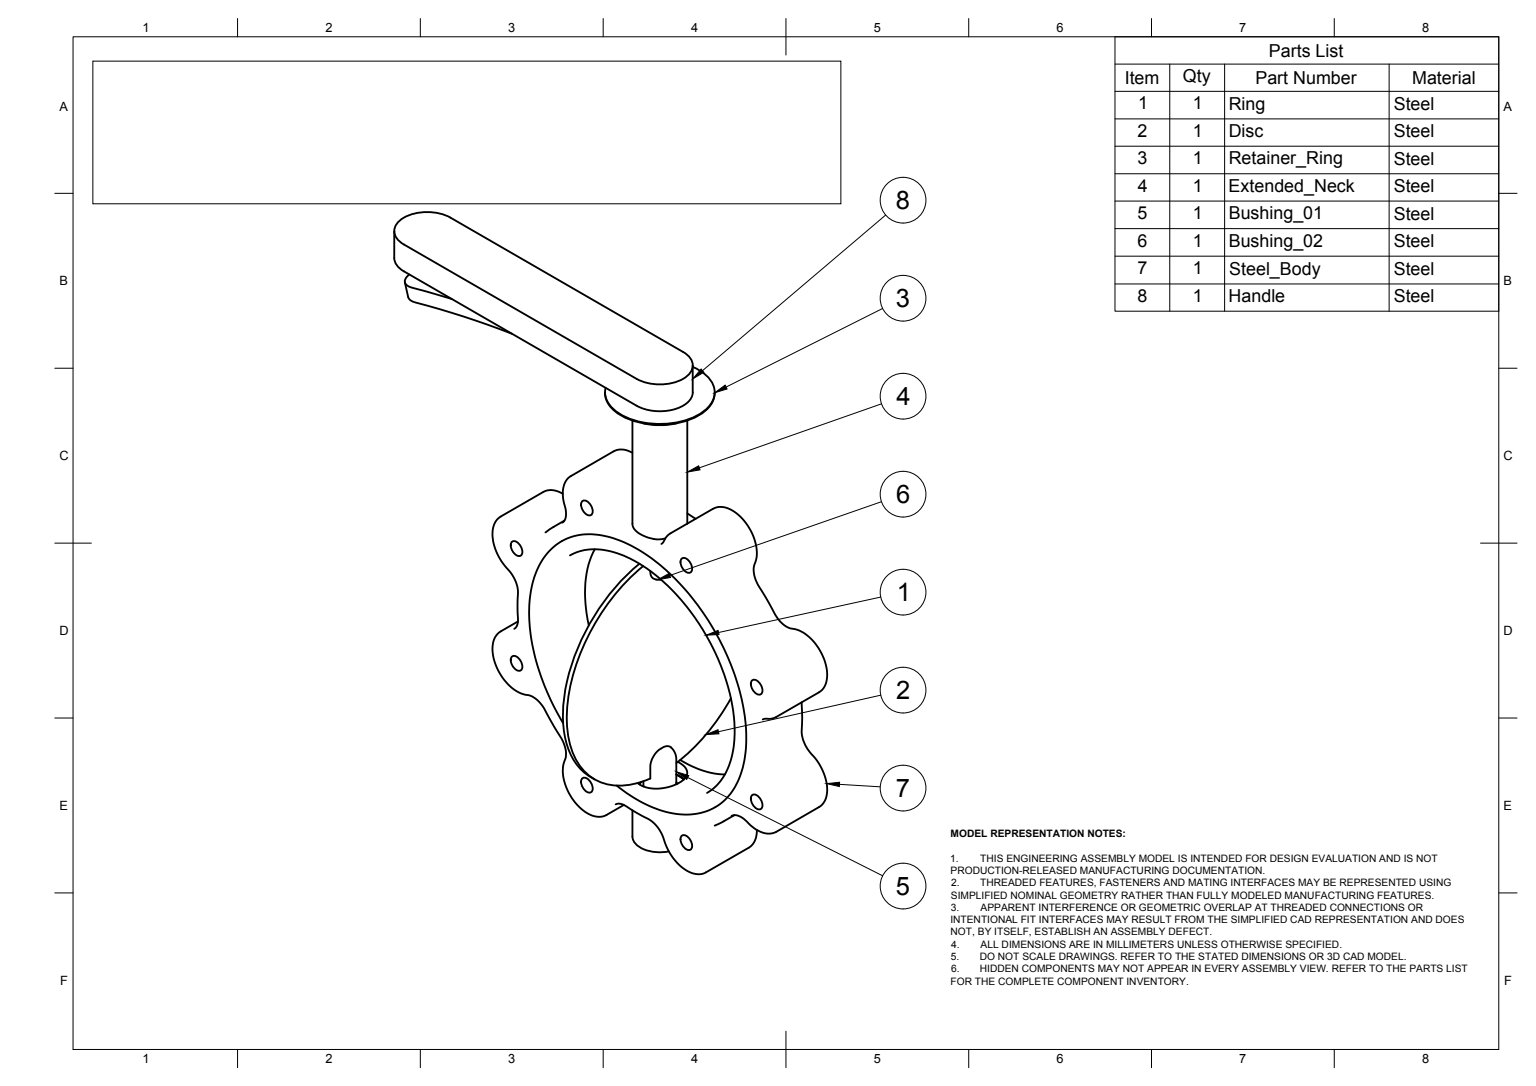
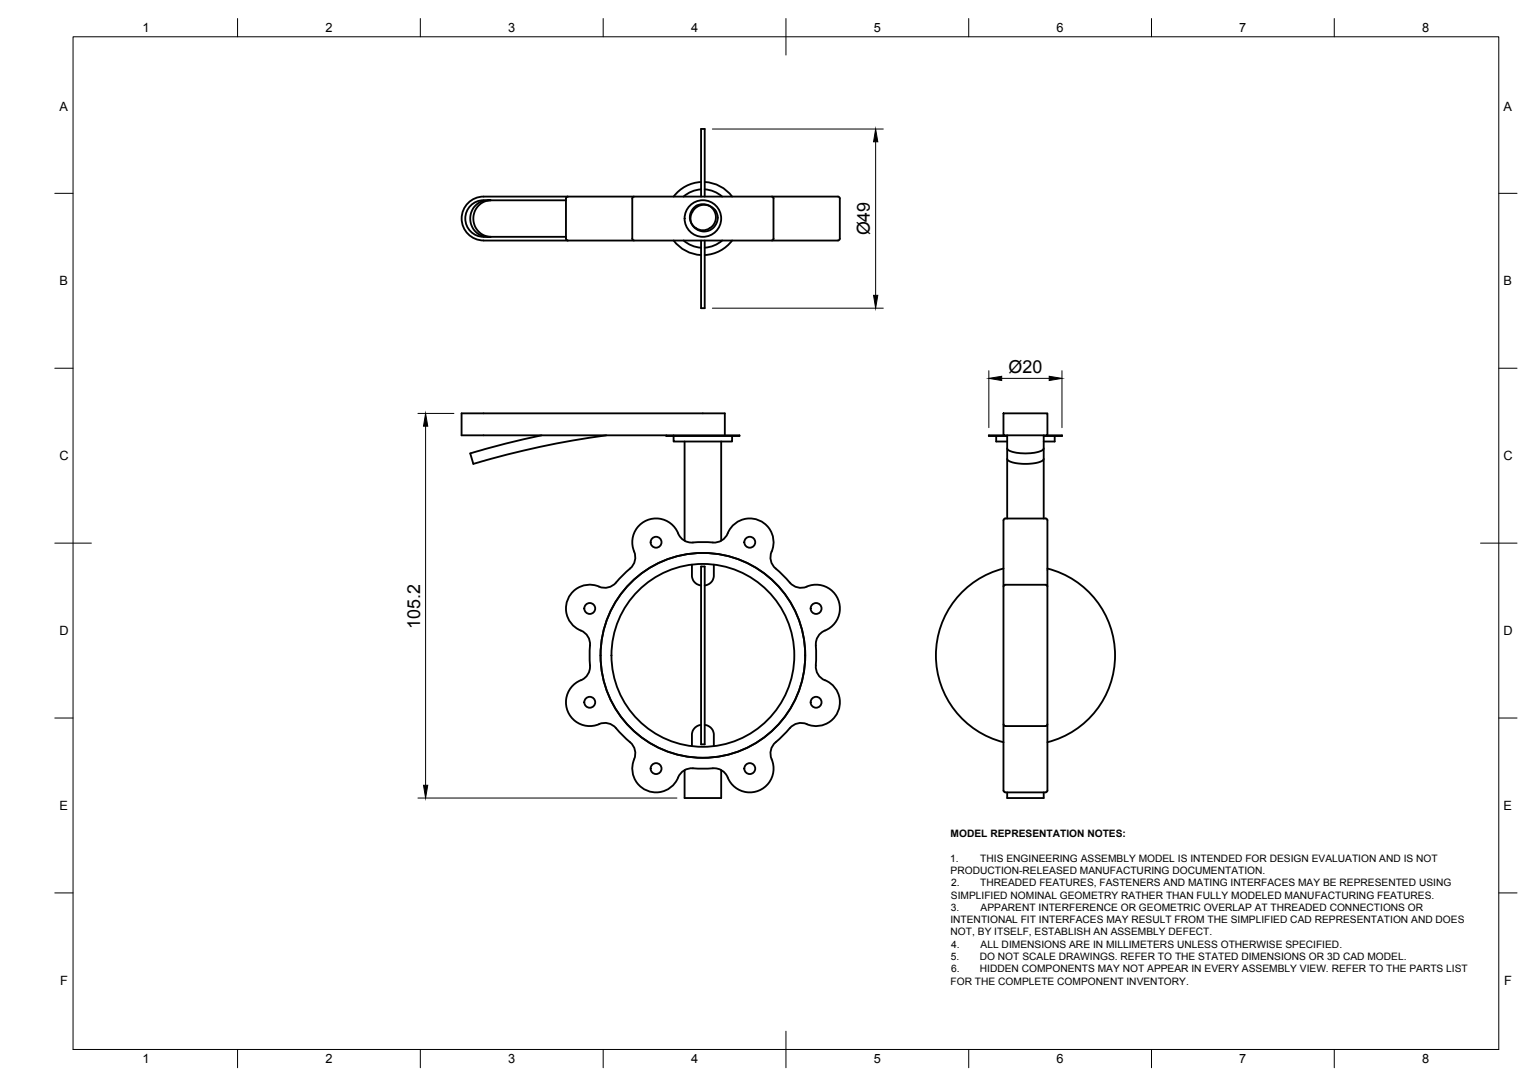
ISO-10303-21;
HEADER;
/* Generated by software containing ST-Developer
 * from STEP Tools, Inc. (www.steptools.com) 
 */

FILE_DESCRIPTION(
/* description */ (''),
/* implementation_level */ '2;1');

FILE_NAME(
/* name */ 'BR-303',
/* time_stamp */ '2026-10-06T12:52:28-07:00',
/* author */ (''),
/* organization */ (''),
/* preprocessor_version */ 'ST-DEVELOPER v20.2',
/* originating_system */ 'Autodesk Translation Framework v15.15.0.0',
/* authorisation */ '');

FILE_SCHEMA (('AUTOMOTIVE_DESIGN { 1 0 10303 214 3 1 1 }'));
ENDSEC;

DATA;
#10=MECHANICAL_DESIGN_GEOMETRIC_PRESENTATION_REPRESENTATION('',(#73,#74,
#75,#76,#77,#78,#79,#80),#34403);
#11=ITEM_DEFINED_TRANSFORMATION($,$,#4480,#4995);
#12=ITEM_DEFINED_TRANSFORMATION($,$,#4507,#4996);
#13=ITEM_DEFINED_TRANSFORMATION($,$,#4513,#4997);
#14=ITEM_DEFINED_TRANSFORMATION($,$,#4522,#4998);
#15=ITEM_DEFINED_TRANSFORMATION($,$,#4557,#4999);
#16=ITEM_DEFINED_TRANSFORMATION($,$,#4579,#5000);
#17=ITEM_DEFINED_TRANSFORMATION($,$,#4604,#5001);
#18=ITEM_DEFINED_TRANSFORMATION($,$,#4956,#5002);
#19=(
REPRESENTATION_RELATIONSHIP($,$,#34435,#34434)
REPRESENTATION_RELATIONSHIP_WITH_TRANSFORMATION(#11)
SHAPE_REPRESENTATION_RELATIONSHIP()
);
#20=(
REPRESENTATION_RELATIONSHIP($,$,#34436,#34434)
REPRESENTATION_RELATIONSHIP_WITH_TRANSFORMATION(#12)
SHAPE_REPRESENTATION_RELATIONSHIP()
);
#21=(
REPRESENTATION_RELATIONSHIP($,$,#34437,#34434)
REPRESENTATION_RELATIONSHIP_WITH_TRANSFORMATION(#13)
SHAPE_REPRESENTATION_RELATIONSHIP()
);
#22=(
REPRESENTATION_RELATIONSHIP($,$,#34438,#34434)
REPRESENTATION_RELATIONSHIP_WITH_TRANSFORMATION(#14)
SHAPE_REPRESENTATION_RELATIONSHIP()
);
#23=(
REPRESENTATION_RELATIONSHIP($,$,#34439,#34434)
REPRESENTATION_RELATIONSHIP_WITH_TRANSFORMATION(#15)
SHAPE_REPRESENTATION_RELATIONSHIP()
);
#24=(
REPRESENTATION_RELATIONSHIP($,$,#34440,#34434)
REPRESENTATION_RELATIONSHIP_WITH_TRANSFORMATION(#16)
SHAPE_REPRESENTATION_RELATIONSHIP()
);
#25=(
REPRESENTATION_RELATIONSHIP($,$,#34441,#34434)
REPRESENTATION_RELATIONSHIP_WITH_TRANSFORMATION(#17)
SHAPE_REPRESENTATION_RELATIONSHIP()
);
#26=(
REPRESENTATION_RELATIONSHIP($,$,#34442,#34434)
REPRESENTATION_RELATIONSHIP_WITH_TRANSFORMATION(#18)
SHAPE_REPRESENTATION_RELATIONSHIP()
);
#27=CONTEXT_DEPENDENT_SHAPE_REPRESENTATION(#19,#34426);
#28=CONTEXT_DEPENDENT_SHAPE_REPRESENTATION(#20,#34427);
#29=CONTEXT_DEPENDENT_SHAPE_REPRESENTATION(#21,#34428);
#30=CONTEXT_DEPENDENT_SHAPE_REPRESENTATION(#22,#34429);
#31=CONTEXT_DEPENDENT_SHAPE_REPRESENTATION(#23,#34430);
#32=CONTEXT_DEPENDENT_SHAPE_REPRESENTATION(#24,#34431);
#33=CONTEXT_DEPENDENT_SHAPE_REPRESENTATION(#25,#34432);
#34=CONTEXT_DEPENDENT_SHAPE_REPRESENTATION(#26,#34433);
#35=NEXT_ASSEMBLY_USAGE_OCCURRENCE('Ring:1','Ring:1','Ring:1',#34444,#34445,
'Ring:1');
#36=NEXT_ASSEMBLY_USAGE_OCCURRENCE('Disc:1','Disc:1','Disc:1',#34444,#34446,
'Disc:1');
#37=NEXT_ASSEMBLY_USAGE_OCCURRENCE('Retainer_Ring:1','Retainer_Ring:1',
'Retainer_Ring:1',#34444,#34447,'Retainer_Ring:1');
#38=NEXT_ASSEMBLY_USAGE_OCCURRENCE('Extended_Neck:1','Extended_Neck:1',
'Extended_Neck:1',#34444,#34448,'Extended_Neck:1');
#39=NEXT_ASSEMBLY_USAGE_OCCURRENCE('Bushing_01:1','Bushing_01:1',
'Bushing_01:1',#34444,#34449,'Bushing_01:1');
#40=NEXT_ASSEMBLY_USAGE_OCCURRENCE('Bushing_02:1','Bushing_02:1',
'Bushing_02:1',#34444,#34450,'Bushing_02:1');
#41=NEXT_ASSEMBLY_USAGE_OCCURRENCE('Steel_Body:1','Steel_Body:1',
'Steel_Body:1',#34444,#34451,'Steel_Body:1');
#42=NEXT_ASSEMBLY_USAGE_OCCURRENCE('Handle:1','Handle:1','Handle:1',#34444,
#34452,'Handle:1');
#43=ELLIPSE('',#4958,16.4522491302287,5.);
#44=ELLIPSE('',#4959,16.4522491302287,5.);
#45=B_SPLINE_SURFACE_WITH_KNOTS('',3,3,((#12810,#12811,#12812,#12813,#12814,
#12815,#12816,#12817,#12818,#12819,#12820,#12821,#12822,#12823,#12824,#12825,
#12826,#12827,#12828,#12829,#12830,#12831,#12832,#12833,#12834,#12835,#12836,
#12837,#12838,#12839,#12840,#12841,#12842,#12843,#12844,#12845,#12846,#12847,
#12848,#12849,#12850,#12851,#12852,#12853,#12854,#12855,#12856,#12857,#12858,
#12859,#12860,#12861,#12862,#12863,#12864,#12865),(#12866,#12867,#12868,
#12869,#12870,#12871,#12872,#12873,#12874,#12875,#12876,#12877,#12878,#12879,
#12880,#12881,#12882,#12883,#12884,#12885,#12886,#12887,#12888,#12889,#12890,
#12891,#12892,#12893,#12894,#12895,#12896,#12897,#12898,#12899,#12900,#12901,
#12902,#12903,#12904,#12905,#12906,#12907,#12908,#12909,#12910,#12911,#12912,
#12913,#12914,#12915,#12916,#12917,#12918,#12919,#12920,#12921),(#12922,
#12923,#12924,#12925,#12926,#12927,#12928,#12929,#12930,#12931,#12932,#12933,
#12934,#12935,#12936,#12937,#12938,#12939,#12940,#12941,#12942,#12943,#12944,
#12945,#12946,#12947,#12948,#12949,#12950,#12951,#12952,#12953,#12954,#12955,
#12956,#12957,#12958,#12959,#12960,#12961,#12962,#12963,#12964,#12965,#12966,
#12967,#12968,#12969,#12970,#12971,#12972,#12973,#12974,#12975,#12976,#12977),
(#12978,#12979,#12980,#12981,#12982,#12983,#12984,#12985,#12986,#12987,
#12988,#12989,#12990,#12991,#12992,#12993,#12994,#12995,#12996,#12997,#12998,
#12999,#13000,#13001,#13002,#13003,#13004,#13005,#13006,#13007,#13008,#13009,
#13010,#13011,#13012,#13013,#13014,#13015,#13016,#13017,#13018,#13019,#13020,
#13021,#13022,#13023,#13024,#13025,#13026,#13027,#13028,#13029,#13030,#13031,
#13032,#13033)),.UNSPECIFIED.,.F.,.F.,.F.,(4,4),(4,1,1,1,1,1,1,1,1,1,1,
1,1,1,1,1,1,1,1,1,1,1,1,1,1,1,1,1,1,1,1,1,1,1,1,1,1,1,1,1,1,1,1,1,1,1,1,
1,1,1,1,1,1,4),(-0.00052867975577478,0.0806738746488675),(15.627449007124,
16.6139235895809,17.6003981720377,18.5868727544945,19.5733473369513,20.5598219194081,
21.5462965018649,22.5327710843217,23.5192456667785,24.5057202492353,25.4921948316921,
26.4786694141489,27.4651439966058,28.4516185790626,29.4380931615194,30.4245677439762,
31.411042326433,32.3975169088898,33.3839914913466,34.3704660738034,35.3569406562602,
36.343415238717,37.3298898211739,38.3163644036307,39.3028389860875,40.2893135685443,
41.2757881510011,42.2622627334579,43.2487373159147,44.2352118983715,45.2216864808283,
46.2081610632851,47.1946356457419,48.1811102281988,49.1675848106556,50.1540593931124,
51.1405339755692,52.127008558026,53.1134831404828,54.0999577229396,55.0864323053964,
56.0729068878532,57.05938147031,58.0458560527669,59.0323306352237,60.0188052176805,
61.0052798001373,61.9917543825941,62.9782289650509,63.9647035475077,64.9511781299645,
65.9376527124213,66.9241272948781,67.9106018773349),.UNSPECIFIED.);
#46=B_SPLINE_SURFACE_WITH_KNOTS('',3,3,((#13314,#13315,#13316,#13317,#13318,
#13319,#13320,#13321,#13322,#13323,#13324,#13325,#13326,#13327,#13328,#13329,
#13330,#13331,#13332,#13333,#13334,#13335,#13336,#13337,#13338,#13339,#13340,
#13341,#13342,#13343,#13344,#13345,#13346,#13347,#13348,#13349,#13350,#13351,
#13352,#13353,#13354,#13355,#13356,#13357,#13358,#13359,#13360,#13361,#13362,
#13363,#13364,#13365,#13366,#13367,#13368,#13369),(#13370,#13371,#13372,
#13373,#13374,#13375,#13376,#13377,#13378,#13379,#13380,#13381,#13382,#13383,
#13384,#13385,#13386,#13387,#13388,#13389,#13390,#13391,#13392,#13393,#13394,
#13395,#13396,#13397,#13398,#13399,#13400,#13401,#13402,#13403,#13404,#13405,
#13406,#13407,#13408,#13409,#13410,#13411,#13412,#13413,#13414,#13415,#13416,
#13417,#13418,#13419,#13420,#13421,#13422,#13423,#13424,#13425),(#13426,
#13427,#13428,#13429,#13430,#13431,#13432,#13433,#13434,#13435,#13436,#13437,
#13438,#13439,#13440,#13441,#13442,#13443,#13444,#13445,#13446,#13447,#13448,
#13449,#13450,#13451,#13452,#13453,#13454,#13455,#13456,#13457,#13458,#13459,
#13460,#13461,#13462,#13463,#13464,#13465,#13466,#13467,#13468,#13469,#13470,
#13471,#13472,#13473,#13474,#13475,#13476,#13477,#13478,#13479,#13480,#13481),
(#13482,#13483,#13484,#13485,#13486,#13487,#13488,#13489,#13490,#13491,
#13492,#13493,#13494,#13495,#13496,#13497,#13498,#13499,#13500,#13501,#13502,
#13503,#13504,#13505,#13506,#13507,#13508,#13509,#13510,#13511,#13512,#13513,
#13514,#13515,#13516,#13517,#13518,#13519,#13520,#13521,#13522,#13523,#13524,
#13525,#13526,#13527,#13528,#13529,#13530,#13531,#13532,#13533,#13534,#13535,
#13536,#13537)),.UNSPECIFIED.,.F.,.F.,.F.,(4,4),(4,1,1,1,1,1,1,1,1,1,1,
1,1,1,1,1,1,1,1,1,1,1,1,1,1,1,1,1,1,1,1,1,1,1,1,1,1,1,1,1,1,1,1,1,1,1,1,
1,1,1,1,1,1,4),(-0.000393360025247636,0.0809589398657946),(18.1690368310252,
19.155511413482,20.1419859959388,21.1284605783956,22.1149351608524,23.1014097433092,
24.087884325766,25.0743589082228,26.0608334906796,27.0473080731364,28.0337826555933,
29.0202572380501,30.0067318205069,30.9932064029637,31.9796809854205,32.9661555678773,
33.9526301503341,34.9391047327909,35.9255793152477,36.9120538977045,37.8985284801614,
38.8850030626182,39.871477645075,40.8579522275318,41.8444268099886,42.8309013924454,
43.8173759749022,44.803850557359,45.7903251398158,46.7767997222726,47.7632743047295,
48.7497488871863,49.7362234696431,50.7226980520999,51.7091726345567,52.6956472170135,
53.6821217994703,54.6685963819271,55.6550709643839,56.6415455468407,57.6280201292976,
58.6144947117544,59.6009692942112,60.587443876668,61.5739184591248,62.5603930415816,
63.5468676240384,64.5333422064952,65.519816788952,66.5062913714088,67.4927659538656,
68.4792405363225,69.4657151187793,70.452868086171),.UNSPECIFIED.);
#47=B_SPLINE_SURFACE_WITH_KNOTS('',3,3,((#18145,#18146,#18147,#18148,#18149,
#18150,#18151,#18152,#18153),(#18154,#18155,#18156,#18157,#18158,#18159,
#18160,#18161,#18162),(#18163,#18164,#18165,#18166,#18167,#18168,#18169,
#18170,#18171),(#18172,#18173,#18174,#18175,#18176,#18177,#18178,#18179,
#18180),(#18181,#18182,#18183,#18184,#18185,#18186,#18187,#18188,#18189)),
 .UNSPECIFIED.,.F.,.F.,.F.,(4,1,4),(4,1,1,1,1,1,4),(-2.31295147948379E-5,
0.571428571428571,1.),(-0.0392722280793192,-0.0280568740573752,-0.00562616601348723,
0.00558918800845676,0.0168045420304008,0.0280198960523448,0.0392352500742888),
 .UNSPECIFIED.);
#48=B_SPLINE_SURFACE_WITH_KNOTS('',3,3,((#18360,#18361,#18362,#18363,#18364,
#18365,#18366,#18367,#18368,#18369),(#18370,#18371,#18372,#18373,#18374,
#18375,#18376,#18377,#18378,#18379),(#18380,#18381,#18382,#18383,#18384,
#18385,#18386,#18387,#18388,#18389),(#18390,#18391,#18392,#18393,#18394,
#18395,#18396,#18397,#18398,#18399),(#18400,#18401,#18402,#18403,#18404,
#18405,#18406,#18407,#18408,#18409)),.UNSPECIFIED.,.F.,.F.,.F.,(4,1,4),
(4,1,1,1,1,1,1,4),(-2.35337788502184E-5,0.571428571428571,1.),(-0.0392722280793192,
-0.0280568740573752,-0.0168415200354311,-0.00562616601348712,0.0055891880084569,
0.0168045420304009,0.0280198960523449,0.0392352500742889),.UNSPECIFIED.);
#49=B_SPLINE_SURFACE_WITH_KNOTS('',3,3,((#18444,#18445,#18446,#18447,#18448,
#18449,#18450,#18451,#18452,#18453,#18454,#18455,#18456,#18457,#18458,#18459,
#18460,#18461,#18462,#18463,#18464,#18465,#18466,#18467,#18468,#18469,#18470,
#18471,#18472,#18473,#18474,#18475,#18476,#18477,#18478,#18479,#18480,#18481,
#18482,#18483,#18484,#18485,#18486,#18487,#18488,#18489),(#18490,#18491,
#18492,#18493,#18494,#18495,#18496,#18497,#18498,#18499,#18500,#18501,#18502,
#18503,#18504,#18505,#18506,#18507,#18508,#18509,#18510,#18511,#18512,#18513,
#18514,#18515,#18516,#18517,#18518,#18519,#18520,#18521,#18522,#18523,#18524,
#18525,#18526,#18527,#18528,#18529,#18530,#18531,#18532,#18533,#18534,#18535),
(#18536,#18537,#18538,#18539,#18540,#18541,#18542,#18543,#18544,#18545,
#18546,#18547,#18548,#18549,#18550,#18551,#18552,#18553,#18554,#18555,#18556,
#18557,#18558,#18559,#18560,#18561,#18562,#18563,#18564,#18565,#18566,#18567,
#18568,#18569,#18570,#18571,#18572,#18573,#18574,#18575,#18576,#18577,#18578,
#18579,#18580,#18581),(#18582,#18583,#18584,#18585,#18586,#18587,#18588,
#18589,#18590,#18591,#18592,#18593,#18594,#18595,#18596,#18597,#18598,#18599,
#18600,#18601,#18602,#18603,#18604,#18605,#18606,#18607,#18608,#18609,#18610,
#18611,#18612,#18613,#18614,#18615,#18616,#18617,#18618,#18619,#18620,#18621,
#18622,#18623,#18624,#18625,#18626,#18627)),.UNSPECIFIED.,.F.,.F.,.F.,(4,
4),(4,1,1,1,1,1,1,1,1,1,1,1,1,1,1,1,1,1,1,1,1,1,1,1,1,1,1,1,1,1,1,1,1,1,
1,1,1,1,1,1,1,1,1,4),(-0.000633807887895752,0.0823317564776454),(8.31473274985803,
9.29783943738047,10.2809461249029,11.2640528124254,12.2471594999478,13.2302661874702,
14.2133728749927,15.1964795625151,16.1795862500376,17.16269293756,18.1457996250825,
19.1289063126049,20.1120130001274,21.0951196876498,22.0782263751723,23.0613330626947,
24.0444397502171,25.0275464377396,26.010653125262,26.9937598127845,27.9768665003069,
28.9599731878294,29.9430798753518,30.9261865628743,31.9092932503967,32.8923999379191,
33.8755066254416,34.858613312964,35.8417200004865,36.8248266880089,37.8079333755314,
38.7910400630538,39.7741467505763,40.7572534380987,41.7403601256211,42.7234668131436,
43.706573500666,44.6896801881885,45.6727868757109,46.6558935632334,47.6390002507558,
48.6221069382783,49.6052136258007,50.5889541212111),.UNSPECIFIED.);
#50=B_SPLINE_SURFACE_WITH_KNOTS('',3,3,((#18809,#18810,#18811,#18812,#18813,
#18814,#18815,#18816,#18817,#18818,#18819,#18820,#18821,#18822,#18823,#18824,
#18825,#18826,#18827,#18828,#18829,#18830,#18831,#18832,#18833,#18834,#18835,
#18836,#18837,#18838,#18839,#18840,#18841,#18842,#18843,#18844,#18845,#18846,
#18847,#18848,#18849,#18850,#18851,#18852,#18853,#18854),(#18855,#18856,
#18857,#18858,#18859,#18860,#18861,#18862,#18863,#18864,#18865,#18866,#18867,
#18868,#18869,#18870,#18871,#18872,#18873,#18874,#18875,#18876,#18877,#18878,
#18879,#18880,#18881,#18882,#18883,#18884,#18885,#18886,#18887,#18888,#18889,
#18890,#18891,#18892,#18893,#18894,#18895,#18896,#18897,#18898,#18899,#18900),
(#18901,#18902,#18903,#18904,#18905,#18906,#18907,#18908,#18909,#18910,
#18911,#18912,#18913,#18914,#18915,#18916,#18917,#18918,#18919,#18920,#18921,
#18922,#18923,#18924,#18925,#18926,#18927,#18928,#18929,#18930,#18931,#18932,
#18933,#18934,#18935,#18936,#18937,#18938,#18939,#18940,#18941,#18942,#18943,
#18944,#18945,#18946),(#18947,#18948,#18949,#18950,#18951,#18952,#18953,
#18954,#18955,#18956,#18957,#18958,#18959,#18960,#18961,#18962,#18963,#18964,
#18965,#18966,#18967,#18968,#18969,#18970,#18971,#18972,#18973,#18974,#18975,
#18976,#18977,#18978,#18979,#18980,#18981,#18982,#18983,#18984,#18985,#18986,
#18987,#18988,#18989,#18990,#18991,#18992)),.UNSPECIFIED.,.F.,.F.,.F.,(4,
4),(4,1,1,1,1,1,1,1,1,1,1,1,1,1,1,1,1,1,1,1,1,1,1,1,1,1,1,1,1,1,1,1,1,1,
1,1,1,1,1,1,1,1,1,4),(-0.000319018948610172,0.0826465308545402),(11.6145803026385,
12.5983209152772,13.5814276027996,14.564534290322,15.5476409778445,16.5307476653669,
17.5138543528894,18.4969610404118,19.4800677279343,20.4631744154567,21.4462811029792,
22.4293877905016,23.4124944780241,24.3956011655465,25.3787078530689,26.3618145405914,
27.3449212281138,28.3280279156363,29.3111346031587,30.2942412906812,31.2773479782036,
32.2604546657261,33.2435613532485,34.226668040771,35.2097747282934,36.1928814158158,
37.1759881033383,38.1590947908607,39.1422014783832,40.1253081659056,41.1084148534281,
42.0915215409505,43.074628228473,44.0577349159954,45.0408416035178,46.0239482910403,
47.0070549785627,47.9901616660852,48.9732683536076,49.9563750411301,50.9394817286525,
51.922588416175,52.9056951036974,53.8888017912198),.UNSPECIFIED.);
#51=B_SPLINE_SURFACE_WITH_KNOTS('',3,3,((#24901,#24902,#24903,#24904,#24905,
#24906,#24907,#24908,#24909),(#24910,#24911,#24912,#24913,#24914,#24915,
#24916,#24917,#24918),(#24919,#24920,#24921,#24922,#24923,#24924,#24925,
#24926,#24927),(#24928,#24929,#24930,#24931,#24932,#24933,#24934,#24935,
#24936),(#24937,#24938,#24939,#24940,#24941,#24942,#24943,#24944,#24945)),
 .UNSPECIFIED.,.F.,.F.,.F.,(4,1,4),(4,1,1,1,1,1,4),(-2.3129491492736E-5,
0.571428571428571,1.),(-0.0392722361364195,-0.0280568820761978,-0.00562617395575443,
0.00558918010446727,0.016804534164689,0.0280198882249107,0.0392352422851324),
 .UNSPECIFIED.);
#52=B_SPLINE_SURFACE_WITH_KNOTS('',3,3,((#25116,#25117,#25118,#25119,#25120,
#25121,#25122,#25123,#25124,#25125),(#25126,#25127,#25128,#25129,#25130,
#25131,#25132,#25133,#25134,#25135),(#25136,#25137,#25138,#25139,#25140,
#25141,#25142,#25143,#25144,#25145),(#25146,#25147,#25148,#25149,#25150,
#25151,#25152,#25153,#25154,#25155),(#25156,#25157,#25158,#25159,#25160,
#25161,#25162,#25163,#25164,#25165)),.UNSPECIFIED.,.F.,.F.,.F.,(4,1,4),
(4,1,1,1,1,1,1,4),(-2.35337502838191E-5,0.571428571428571,1.),(-0.0392722361364195,
-0.0280568820761979,-0.0168415280159762,-0.00562617395575452,0.00558918010446715,
0.0168045341646888,0.0280198882249105,0.0392352422851322),.UNSPECIFIED.);
#53=B_SPLINE_SURFACE_WITH_KNOTS('',3,3,((#25200,#25201,#25202,#25203,#25204,
#25205,#25206,#25207,#25208,#25209,#25210,#25211,#25212,#25213,#25214,#25215,
#25216,#25217,#25218,#25219,#25220,#25221,#25222,#25223,#25224,#25225,#25226,
#25227,#25228,#25229,#25230,#25231,#25232,#25233,#25234,#25235,#25236,#25237,
#25238,#25239,#25240,#25241,#25242,#25243,#25244,#25245,#25246,#25247,#25248,
#25249,#25250,#25251,#25252,#25253,#25254,#25255),(#25256,#25257,#25258,
#25259,#25260,#25261,#25262,#25263,#25264,#25265,#25266,#25267,#25268,#25269,
#25270,#25271,#25272,#25273,#25274,#25275,#25276,#25277,#25278,#25279,#25280,
#25281,#25282,#25283,#25284,#25285,#25286,#25287,#25288,#25289,#25290,#25291,
#25292,#25293,#25294,#25295,#25296,#25297,#25298,#25299,#25300,#25301,#25302,
#25303,#25304,#25305,#25306,#25307,#25308,#25309,#25310,#25311),(#25312,
#25313,#25314,#25315,#25316,#25317,#25318,#25319,#25320,#25321,#25322,#25323,
#25324,#25325,#25326,#25327,#25328,#25329,#25330,#25331,#25332,#25333,#25334,
#25335,#25336,#25337,#25338,#25339,#25340,#25341,#25342,#25343,#25344,#25345,
#25346,#25347,#25348,#25349,#25350,#25351,#25352,#25353,#25354,#25355,#25356,
#25357,#25358,#25359,#25360,#25361,#25362,#25363,#25364,#25365,#25366,#25367),
(#25368,#25369,#25370,#25371,#25372,#25373,#25374,#25375,#25376,#25377,
#25378,#25379,#25380,#25381,#25382,#25383,#25384,#25385,#25386,#25387,#25388,
#25389,#25390,#25391,#25392,#25393,#25394,#25395,#25396,#25397,#25398,#25399,
#25400,#25401,#25402,#25403,#25404,#25405,#25406,#25407,#25408,#25409,#25410,
#25411,#25412,#25413,#25414,#25415,#25416,#25417,#25418,#25419,#25420,#25421,
#25422,#25423)),.UNSPECIFIED.,.F.,.F.,.F.,(4,4),(4,1,1,1,1,1,1,1,1,1,1,
1,1,1,1,1,1,1,1,1,1,1,1,1,1,1,1,1,1,1,1,1,1,1,1,1,1,1,1,1,1,1,1,1,1,1,1,
1,1,1,1,1,1,4),(-0.000662226835936772,0.0823162805313219),(-97.5343202090122,
-96.5415235325365,-95.5487268560609,-94.5559301795852,-93.5631335031096,
-92.570336826634,-91.5775401501583,-90.5847434736827,-89.591946797207,-88.5991501207314,
-87.6063534442557,-86.6135567677801,-85.6207600913045,-84.6279634148288,
-83.6351667383532,-82.6423700618775,-81.6495733854019,-80.6567767089262,
-79.6639800324506,-78.671183355975,-77.6783866794993,-76.6855900030237,
-75.692793326548,-74.6999966500724,-73.7071999735967,-72.7144032971211,
-71.7216066206455,-70.7288099441698,-69.7360132676942,-68.7432165912185,
-67.7504199147429,-66.7576232382672,-65.7648265617916,-64.772029885316,
-63.7792332088403,-62.7864365323647,-61.793639855889,-60.8008431794134,
-59.8080465029377,-58.8152498264621,-57.8224531499865,-56.8296564735108,
-55.8368597970352,-54.8440631205595,-53.8512664440839,-52.8584697676082,
-51.8656730911326,-50.872876414657,-49.8800797381813,-48.8872830617057,
-47.89448638523,-46.9016897087544,-45.9088930322787,-44.9154341289673),
 .UNSPECIFIED.);
#54=B_SPLINE_SURFACE_WITH_KNOTS('',3,3,((#25626,#25627,#25628,#25629,#25630,
#25631,#25632,#25633,#25634,#25635,#25636,#25637,#25638,#25639,#25640,#25641,
#25642,#25643,#25644,#25645,#25646,#25647,#25648,#25649,#25650,#25651,#25652,
#25653,#25654,#25655,#25656,#25657,#25658,#25659,#25660,#25661,#25662,#25663,
#25664,#25665,#25666,#25667,#25668,#25669,#25670,#25671,#25672,#25673,#25674,
#25675,#25676,#25677,#25678,#25679,#25680,#25681),(#25682,#25683,#25684,
#25685,#25686,#25687,#25688,#25689,#25690,#25691,#25692,#25693,#25694,#25695,
#25696,#25697,#25698,#25699,#25700,#25701,#25702,#25703,#25704,#25705,#25706,
#25707,#25708,#25709,#25710,#25711,#25712,#25713,#25714,#25715,#25716,#25717,
#25718,#25719,#25720,#25721,#25722,#25723,#25724,#25725,#25726,#25727,#25728,
#25729,#25730,#25731,#25732,#25733,#25734,#25735,#25736,#25737),(#25738,
#25739,#25740,#25741,#25742,#25743,#25744,#25745,#25746,#25747,#25748,#25749,
#25750,#25751,#25752,#25753,#25754,#25755,#25756,#25757,#25758,#25759,#25760,
#25761,#25762,#25763,#25764,#25765,#25766,#25767,#25768,#25769,#25770,#25771,
#25772,#25773,#25774,#25775,#25776,#25777,#25778,#25779,#25780,#25781,#25782,
#25783,#25784,#25785,#25786,#25787,#25788,#25789,#25790,#25791,#25792,#25793),
(#25794,#25795,#25796,#25797,#25798,#25799,#25800,#25801,#25802,#25803,
#25804,#25805,#25806,#25807,#25808,#25809,#25810,#25811,#25812,#25813,#25814,
#25815,#25816,#25817,#25818,#25819,#25820,#25821,#25822,#25823,#25824,#25825,
#25826,#25827,#25828,#25829,#25830,#25831,#25832,#25833,#25834,#25835,#25836,
#25837,#25838,#25839,#25840,#25841,#25842,#25843,#25844,#25845,#25846,#25847,
#25848,#25849)),.UNSPECIFIED.,.F.,.F.,.F.,(4,4),(4,1,1,1,1,1,1,1,1,1,1,
1,1,1,1,1,1,1,1,1,1,1,1,1,1,1,1,1,1,1,1,1,1,1,1,1,1,1,1,1,1,1,1,1,1,1,1,
1,1,1,1,1,1,4),(-0.000307057037193035,0.0826748885905267),(-94.2345010139676,
-93.2410420546399,-92.2482453781643,-91.2554487016887,-90.2626520252132,
-89.2698553487376,-88.277058672262,-87.2842619957864,-86.2914653193108,
-85.2986686428353,-84.3058719663597,-83.3130752898841,-82.3202786134085,
-81.327481936933,-80.3346852604574,-79.3418885839818,-78.3490919075062,
-77.3562952310307,-76.3634985545551,-75.3707018780795,-74.3779052016039,
-73.3851085251283,-72.3923118486528,-71.3995151721772,-70.4067184957016,
-69.413921819226,-68.4211251427505,-67.4283284662749,-66.4355317897993,
-65.4427351133237,-64.4499384368482,-63.4571417603726,-62.464345083897,
-61.4715484074214,-60.4787517309458,-59.4859550544703,-58.4931583779947,
-57.5003617015191,-56.5075650250435,-55.514768348568,-54.5219716720924,
-53.5291749956168,-52.5363783191412,-51.5435816426657,-50.5507849661901,
-49.5579882897145,-48.5651916132389,-47.5723949367633,-46.5795982602878,
-45.5868015838122,-44.5940049073366,-43.601208230861,-42.6084115543855,
-41.6156148779099),.UNSPECIFIED.);
#55=B_SPLINE_SURFACE_WITH_KNOTS('',3,3,((#32660,#32661,#32662,#32663,#32664,
#32665,#32666,#32667,#32668,#32669,#32670,#32671,#32672,#32673,#32674,#32675,
#32676,#32677,#32678,#32679,#32680,#32681,#32682,#32683,#32684,#32685,#32686,
#32687,#32688,#32689,#32690,#32691,#32692,#32693,#32694,#32695,#32696,#32697,
#32698,#32699,#32700,#32701,#32702,#32703,#32704,#32705,#32706,#32707,#32708,
#32709,#32710,#32711,#32712,#32713,#32714,#32715,#32716,#32717,#32718,#32719,
#32720),(#32721,#32722,#32723,#32724,#32725,#32726,#32727,#32728,#32729,
#32730,#32731,#32732,#32733,#32734,#32735,#32736,#32737,#32738,#32739,#32740,
#32741,#32742,#32743,#32744,#32745,#32746,#32747,#32748,#32749,#32750,#32751,
#32752,#32753,#32754,#32755,#32756,#32757,#32758,#32759,#32760,#32761,#32762,
#32763,#32764,#32765,#32766,#32767,#32768,#32769,#32770,#32771,#32772,#32773,
#32774,#32775,#32776,#32777,#32778,#32779,#32780,#32781),(#32782,#32783,
#32784,#32785,#32786,#32787,#32788,#32789,#32790,#32791,#32792,#32793,#32794,
#32795,#32796,#32797,#32798,#32799,#32800,#32801,#32802,#32803,#32804,#32805,
#32806,#32807,#32808,#32809,#32810,#32811,#32812,#32813,#32814,#32815,#32816,
#32817,#32818,#32819,#32820,#32821,#32822,#32823,#32824,#32825,#32826,#32827,
#32828,#32829,#32830,#32831,#32832,#32833,#32834,#32835,#32836,#32837,#32838,
#32839,#32840,#32841,#32842),(#32843,#32844,#32845,#32846,#32847,#32848,
#32849,#32850,#32851,#32852,#32853,#32854,#32855,#32856,#32857,#32858,#32859,
#32860,#32861,#32862,#32863,#32864,#32865,#32866,#32867,#32868,#32869,#32870,
#32871,#32872,#32873,#32874,#32875,#32876,#32877,#32878,#32879,#32880,#32881,
#32882,#32883,#32884,#32885,#32886,#32887,#32888,#32889,#32890,#32891,#32892,
#32893,#32894,#32895,#32896,#32897,#32898,#32899,#32900,#32901,#32902,#32903)),
 .UNSPECIFIED.,.F.,.F.,.F.,(4,4),(4,1,1,1,1,1,1,1,1,1,1,1,1,1,1,1,1,1,1,
1,1,1,1,1,1,1,1,1,1,1,1,1,1,1,1,1,1,1,1,1,1,1,1,1,1,1,1,1,1,1,1,1,1,1,1,
1,1,1,4),(-0.000677904662105755,0.0806892635940671),(11.8568599181543,12.8456361179191,
13.8337344130217,14.8218327081244,15.8099310032271,16.7980292983297,17.7861275934324,
18.774225888535,19.7623241836377,20.7504224787404,21.738520773843,22.7266190689457,
23.7147173640484,24.702815659151,25.6909139542537,26.6790122493564,27.667110544459,
28.6552088395617,29.6433071346644,30.631405429767,31.6195037248697,32.6076020199723,
33.595700315075,34.5837986101777,35.5718969052803,36.559995200383,37.5480934954857,
38.5361917905883,39.524290085691,40.5123883807937,41.5004866758963,42.488584970999,
43.4766832661016,44.4647815612043,45.452879856307,46.4409781514096,47.4290764465123,
48.417174741615,49.4052730367176,50.3933713318203,51.381469626923,52.3695679220256,
53.3576662171283,54.345764512231,55.3338628073336,56.3219611024363,57.3100593975389,
58.2981576926416,59.2862559877443,60.2743542828469,61.2624525779496,62.2505508730523,
63.2386491681549,64.2267474632576,65.2148457583603,66.2029440534629,67.1910423485656,
68.1791406436682,69.1672389387709),.UNSPECIFIED.);
#56=B_SPLINE_SURFACE_WITH_KNOTS('',3,3,((#33092,#33093,#33094,#33095,#33096,
#33097,#33098,#33099,#33100,#33101,#33102,#33103,#33104,#33105,#33106,#33107,
#33108,#33109,#33110,#33111,#33112,#33113,#33114,#33115,#33116,#33117,#33118,
#33119,#33120,#33121,#33122,#33123,#33124,#33125,#33126,#33127,#33128,#33129,
#33130,#33131,#33132,#33133,#33134,#33135,#33136,#33137,#33138,#33139,#33140,
#33141,#33142,#33143,#33144,#33145,#33146,#33147,#33148,#33149,#33150,#33151,
#33152),(#33153,#33154,#33155,#33156,#33157,#33158,#33159,#33160,#33161,
#33162,#33163,#33164,#33165,#33166,#33167,#33168,#33169,#33170,#33171,#33172,
#33173,#33174,#33175,#33176,#33177,#33178,#33179,#33180,#33181,#33182,#33183,
#33184,#33185,#33186,#33187,#33188,#33189,#33190,#33191,#33192,#33193,#33194,
#33195,#33196,#33197,#33198,#33199,#33200,#33201,#33202,#33203,#33204,#33205,
#33206,#33207,#33208,#33209,#33210,#33211,#33212,#33213),(#33214,#33215,
#33216,#33217,#33218,#33219,#33220,#33221,#33222,#33223,#33224,#33225,#33226,
#33227,#33228,#33229,#33230,#33231,#33232,#33233,#33234,#33235,#33236,#33237,
#33238,#33239,#33240,#33241,#33242,#33243,#33244,#33245,#33246,#33247,#33248,
#33249,#33250,#33251,#33252,#33253,#33254,#33255,#33256,#33257,#33258,#33259,
#33260,#33261,#33262,#33263,#33264,#33265,#33266,#33267,#33268,#33269,#33270,
#33271,#33272,#33273,#33274),(#33275,#33276,#33277,#33278,#33279,#33280,
#33281,#33282,#33283,#33284,#33285,#33286,#33287,#33288,#33289,#33290,#33291,
#33292,#33293,#33294,#33295,#33296,#33297,#33298,#33299,#33300,#33301,#33302,
#33303,#33304,#33305,#33306,#33307,#33308,#33309,#33310,#33311,#33312,#33313,
#33314,#33315,#33316,#33317,#33318,#33319,#33320,#33321,#33322,#33323,#33324,
#33325,#33326,#33327,#33328,#33329,#33330,#33331,#33332,#33333,#33334,#33335)),
 .UNSPECIFIED.,.F.,.F.,.F.,(4,4),(4,1,1,1,1,1,1,1,1,1,1,1,1,1,1,1,1,1,1,
1,1,1,1,1,1,1,1,1,1,1,1,1,1,1,1,1,1,1,1,1,1,1,1,1,1,1,1,1,1,1,1,1,1,1,1,
1,1,1,4),(-0.000408738892527466,0.0809585600709479),(14.3991256467175,15.3872239418202,
16.3753222369229,17.3634205320255,18.3515188271282,19.3396171222308,20.3277154173335,
21.3158137124362,22.3039120075388,23.2920103026415,24.2801085977442,25.2682068928468,
26.2563051879495,27.2444034830521,28.2325017781548,29.2206000732575,30.2086983683601,
31.1967966634628,32.1848949585655,33.1729932536681,34.1610915487708,35.1491898438735,
36.1372881389761,37.1253864340788,38.1134847291814,39.1015830242841,40.0896813193868,
41.0777796144894,42.0658779095921,43.0539762046948,44.0420744997974,45.0301727949001,
46.0182710900028,47.0063693851054,47.9944676802081,48.9825659753107,49.9706642704134,
50.9587625655161,51.9468608606187,52.9349591557214,53.9230574508241,54.9111557459267,
55.8992540410294,56.8873523361321,57.8754506312347,58.8635489263374,59.85164722144,
60.8397455165427,61.8278438116454,62.815942106748,63.8040404018507,64.7921386969534,
65.780236992056,66.7683352871587,67.7564335822614,68.744531877364,69.7326301724667,
70.7207284675693,71.7095047678121),.UNSPECIFIED.);
#57=SHAPE_REPRESENTATION_RELATIONSHIP('SRR','None',#34435,#65);
#58=SHAPE_REPRESENTATION_RELATIONSHIP('SRR','None',#34436,#66);
#59=SHAPE_REPRESENTATION_RELATIONSHIP('SRR','None',#34437,#67);
#60=SHAPE_REPRESENTATION_RELATIONSHIP('SRR','None',#34438,#68);
#61=SHAPE_REPRESENTATION_RELATIONSHIP('SRR','None',#34439,#69);
#62=SHAPE_REPRESENTATION_RELATIONSHIP('SRR','None',#34440,#70);
#63=SHAPE_REPRESENTATION_RELATIONSHIP('SRR','None',#34441,#71);
#64=SHAPE_REPRESENTATION_RELATIONSHIP('SRR','None',#34442,#72);
#65=ADVANCED_BREP_SHAPE_REPRESENTATION('',(#81),#34395);
#66=ADVANCED_BREP_SHAPE_REPRESENTATION('',(#82),#34396);
#67=ADVANCED_BREP_SHAPE_REPRESENTATION('',(#83),#34397);
#68=ADVANCED_BREP_SHAPE_REPRESENTATION('',(#84),#34398);
#69=ADVANCED_BREP_SHAPE_REPRESENTATION('',(#85),#34399);
#70=ADVANCED_BREP_SHAPE_REPRESENTATION('',(#86),#34400);
#71=ADVANCED_BREP_SHAPE_REPRESENTATION('',(#87),#34401);
#72=ADVANCED_BREP_SHAPE_REPRESENTATION('',(#88),#34402);
#73=STYLED_ITEM('',(#34484),#81);
#74=STYLED_ITEM('',(#34484),#82);
#75=STYLED_ITEM('',(#34484),#83);
#76=STYLED_ITEM('',(#34484),#84);
#77=STYLED_ITEM('',(#34484),#85);
#78=STYLED_ITEM('',(#34484),#86);
#79=STYLED_ITEM('',(#34484),#87);
#80=STYLED_ITEM('',(#34484),#88);
#81=MANIFOLD_SOLID_BREP('Body1',#4382);
#82=MANIFOLD_SOLID_BREP('Body1',#4383);
#83=MANIFOLD_SOLID_BREP('Body1',#4384);
#84=MANIFOLD_SOLID_BREP('Body1',#4385);
#85=MANIFOLD_SOLID_BREP('Body1',#4386);
#86=MANIFOLD_SOLID_BREP('Body1',#4387);
#87=MANIFOLD_SOLID_BREP('Body1',#4388);
#88=MANIFOLD_SOLID_BREP('Body1',#4389);
#89=FACE_BOUND('',#751,.T.);
#90=FACE_BOUND('',#753,.T.);
#91=FACE_BOUND('',#754,.T.);
#92=FACE_BOUND('',#757,.T.);
#93=FACE_BOUND('',#758,.T.);
#94=FACE_BOUND('',#761,.T.);
#95=FACE_BOUND('',#769,.T.);
#96=FACE_BOUND('',#771,.T.);
#97=FACE_BOUND('',#795,.T.);
#98=FACE_BOUND('',#797,.T.);
#99=FACE_BOUND('',#800,.T.);
#100=FACE_BOUND('',#818,.T.);
#101=FACE_BOUND('',#839,.T.);
#102=FACE_BOUND('',#855,.T.);
#103=FACE_BOUND('',#858,.T.);
#104=FACE_BOUND('',#914,.T.);
#105=FACE_BOUND('',#915,.T.);
#106=FACE_BOUND('',#916,.T.);
#107=FACE_BOUND('',#917,.T.);
#108=FACE_BOUND('',#918,.T.);
#109=FACE_BOUND('',#919,.T.);
#110=FACE_BOUND('',#920,.T.);
#111=FACE_BOUND('',#921,.T.);
#112=FACE_BOUND('',#922,.T.);
#113=FACE_BOUND('',#970,.T.);
#114=FACE_BOUND('',#971,.T.);
#115=FACE_BOUND('',#972,.T.);
#116=FACE_BOUND('',#973,.T.);
#117=FACE_BOUND('',#974,.T.);
#118=FACE_BOUND('',#975,.T.);
#119=FACE_BOUND('',#976,.T.);
#120=FACE_BOUND('',#977,.T.);
#121=FACE_BOUND('',#978,.T.);
#122=FACE_BOUND('',#981,.T.);
#123=FACE_BOUND('',#982,.T.);
#124=FACE_BOUND('',#1013,.T.);
#125=PLANE('',#4488);
#126=PLANE('',#4503);
#127=PLANE('',#4511);
#128=PLANE('',#4512);
#129=PLANE('',#4520);
#130=PLANE('',#4521);
#131=PLANE('',#4547);
#132=PLANE('',#4551);
#133=PLANE('',#4553);
#134=PLANE('',#4556);
#135=PLANE('',#4570);
#136=PLANE('',#4574);
#137=PLANE('',#4577);
#138=PLANE('',#4578);
#139=PLANE('',#4595);
#140=PLANE('',#4601);
#141=PLANE('',#4602);
#142=PLANE('',#4603);
#143=PLANE('',#4620);
#144=PLANE('',#4625);
#145=PLANE('',#4794);
#146=PLANE('',#4928);
#147=PLANE('',#4957);
#148=PLANE('',#4971);
#149=PLANE('',#4972);
#150=PLANE('',#4973);
#151=PLANE('',#4974);
#152=PLANE('',#4976);
#153=PLANE('',#4977);
#154=PLANE('',#4980);
#155=PLANE('',#4984);
#156=PLANE('',#4985);
#157=PLANE('',#4989);
#158=PLANE('',#4993);
#159=PLANE('',#4994);
#160=CIRCLE('',#4484,25.5);
#161=CIRCLE('',#4485,0.5);
#162=CIRCLE('',#4486,25.);
#163=CIRCLE('',#4487,25.);
#164=CIRCLE('',#4489,27.5);
#165=CIRCLE('',#4491,25.);
#166=CIRCLE('',#4492,25.);
#167=CIRCLE('',#4494,0.5);
#168=CIRCLE('',#4495,28.);
#169=CIRCLE('',#4496,28.);
#170=CIRCLE('',#4498,28.);
#171=CIRCLE('',#4499,28.);
#172=CIRCLE('',#4501,27.5);
#173=CIRCLE('',#4502,0.5);
#174=CIRCLE('',#4504,25.5);
#175=CIRCLE('',#4506,0.5);
#176=CIRCLE('',#4509,24.5);
#177=CIRCLE('',#4510,24.5);
#178=CIRCLE('',#4515,4.);
#179=CIRCLE('',#4516,4.);
#180=CIRCLE('',#4518,10.);
#181=CIRCLE('',#4519,10.);
#182=CIRCLE('',#4524,4.085);
#183=CIRCLE('',#4532,4.085);
#184=CIRCLE('',#4534,3.38975);
#185=CIRCLE('',#4542,3.38975);
#186=CIRCLE('',#4543,3.38975);
#187=CIRCLE('',#4544,3.38975);
#188=CIRCLE('',#4549,8.);
#189=CIRCLE('',#4550,8.);
#190=CIRCLE('',#4552,5.);
#191=CIRCLE('',#4554,5.);
#192=CIRCLE('',#4559,3.22275);
#193=CIRCLE('',#4566,3.933);
#194=CIRCLE('',#4567,3.933);
#195=CIRCLE('',#4569,3.22275);
#196=CIRCLE('',#4571,24.5);
#197=CIRCLE('',#4573,3.);
#198=CIRCLE('',#4575,24.5);
#199=CIRCLE('',#4581,3.22275);
#200=CIRCLE('',#4590,3.933);
#201=CIRCLE('',#4591,3.94307276060078);
#202=CIRCLE('',#4592,3.933);
#203=CIRCLE('',#4594,3.22275);
#204=CIRCLE('',#4596,24.5);
#205=CIRCLE('',#4598,3.);
#206=CIRCLE('',#4600,24.5);
#207=CIRCLE('',#4606,4.085);
#208=CIRCLE('',#4615,4.085);
#209=CIRCLE('',#4617,3.38975);
#210=CIRCLE('',#4618,3.38975);
#211=CIRCLE('',#4621,5.);
#212=CIRCLE('',#4622,5.);
#213=CIRCLE('',#4624,5.);
#214=CIRCLE('',#4630,4.);
#215=CIRCLE('',#4631,4.);
#216=CIRCLE('',#4633,31.);
#217=CIRCLE('',#4635,4.);
#218=CIRCLE('',#4636,4.);
#219=CIRCLE('',#4638,31.);
#220=CIRCLE('',#4640,0.499999999999994);
#221=CIRCLE('',#4641,4.5);
#222=CIRCLE('',#4642,0.5);
#223=CIRCLE('',#4644,0.5);
#224=CIRCLE('',#4645,6.5);
#225=CIRCLE('',#4646,6.);
#226=CIRCLE('',#4648,0.5);
#227=CIRCLE('',#4649,4.);
#228=CIRCLE('',#4650,4.5);
#229=CIRCLE('',#4652,0.5);
#230=CIRCLE('',#4653,31.);
#231=CIRCLE('',#4654,30.5);
#232=CIRCLE('',#4656,0.5);
#233=CIRCLE('',#4657,4.);
#234=CIRCLE('',#4658,4.5);
#235=CIRCLE('',#4660,0.5);
#236=CIRCLE('',#4661,6.5);
#237=CIRCLE('',#4662,6.);
#238=CIRCLE('',#4664,0.5);
#239=CIRCLE('',#4665,4.);
#240=CIRCLE('',#4666,4.5);
#241=CIRCLE('',#4668,0.5);
#242=CIRCLE('',#4669,31.);
#243=CIRCLE('',#4670,30.5);
#244=CIRCLE('',#4672,0.5);
#245=CIRCLE('',#4673,4.);
#246=CIRCLE('',#4674,4.5);
#247=CIRCLE('',#4676,0.5);
#248=CIRCLE('',#4677,6.5);
#249=CIRCLE('',#4678,6.);
#250=CIRCLE('',#4680,0.5);
#251=CIRCLE('',#4681,4.);
#252=CIRCLE('',#4682,4.5);
#253=CIRCLE('',#4684,0.5);
#254=CIRCLE('',#4685,31.);
#255=CIRCLE('',#4686,30.5);
#256=CIRCLE('',#4688,0.5);
#257=CIRCLE('',#4689,4.);
#258=CIRCLE('',#4690,4.5);
#259=CIRCLE('',#4692,0.5);
#260=CIRCLE('',#4693,6.5);
#261=CIRCLE('',#4694,6.);
#262=CIRCLE('',#4696,0.5);
#263=CIRCLE('',#4697,4.5);
#264=CIRCLE('',#4699,0.5);
#265=CIRCLE('',#4700,31.);
#266=CIRCLE('',#4701,30.5);
#267=CIRCLE('',#4703,0.5);
#268=CIRCLE('',#4704,4.);
#269=CIRCLE('',#4705,4.5);
#270=CIRCLE('',#4707,0.5);
#271=CIRCLE('',#4708,6.5);
#272=CIRCLE('',#4709,6.);
#273=CIRCLE('',#4711,0.5);
#274=CIRCLE('',#4712,4.);
#275=CIRCLE('',#4713,4.5);
#276=CIRCLE('',#4715,0.5);
#277=CIRCLE('',#4716,31.);
#278=CIRCLE('',#4717,30.5);
#279=CIRCLE('',#4719,0.5);
#280=CIRCLE('',#4720,4.);
#281=CIRCLE('',#4721,4.5);
#282=CIRCLE('',#4723,0.5);
#283=CIRCLE('',#4724,6.5);
#284=CIRCLE('',#4725,6.);
#285=CIRCLE('',#4727,0.5);
#286=CIRCLE('',#4728,4.);
#287=CIRCLE('',#4729,4.5);
#288=CIRCLE('',#4731,0.5);
#289=CIRCLE('',#4732,31.);
#290=CIRCLE('',#4733,30.5);
#291=CIRCLE('',#4735,0.5);
#292=CIRCLE('',#4736,4.);
#293=CIRCLE('',#4737,4.5);
#294=CIRCLE('',#4739,0.5);
#295=CIRCLE('',#4740,6.5);
#296=CIRCLE('',#4741,6.);
#297=CIRCLE('',#4743,0.5);
#298=CIRCLE('',#4744,4.);
#299=CIRCLE('',#4745,4.5);
#300=CIRCLE('',#4747,0.5);
#301=CIRCLE('',#4748,31.);
#302=CIRCLE('',#4749,30.5);
#303=CIRCLE('',#4751,0.5);
#304=CIRCLE('',#4752,4.);
#305=CIRCLE('',#4753,4.5);
#306=CIRCLE('',#4755,0.5);
#307=CIRCLE('',#4756,6.5);
#308=CIRCLE('',#4757,6.);
#309=CIRCLE('',#4759,0.5);
#310=CIRCLE('',#4760,4.);
#311=CIRCLE('',#4761,4.5);
#312=CIRCLE('',#4763,30.5);
#313=CIRCLE('',#4765,6.5);
#314=CIRCLE('',#4767,4.);
#315=CIRCLE('',#4769,31.);
#316=CIRCLE('',#4771,4.);
#317=CIRCLE('',#4773,6.5);
#318=CIRCLE('',#4775,4.);
#319=CIRCLE('',#4777,31.);
#320=CIRCLE('',#4779,4.);
#321=CIRCLE('',#4781,6.5);
#322=CIRCLE('',#4783,4.);
#323=CIRCLE('',#4785,31.);
#324=CIRCLE('',#4787,4.);
#325=CIRCLE('',#4789,6.5);
#326=CIRCLE('',#4791,4.);
#327=CIRCLE('',#4793,31.);
#328=CIRCLE('',#4795,28.5);
#329=CIRCLE('',#4796,1.5);
#330=CIRCLE('',#4797,1.5);
#331=CIRCLE('',#4798,1.5);
#332=CIRCLE('',#4799,1.5);
#333=CIRCLE('',#4800,1.5);
#334=CIRCLE('',#4801,1.5);
#335=CIRCLE('',#4802,1.5);
#336=CIRCLE('',#4803,1.5);
#337=CIRCLE('',#4805,0.500000000000001);
#338=CIRCLE('',#4806,4.5);
#339=CIRCLE('',#4807,0.5);
#340=CIRCLE('',#4808,4.);
#341=CIRCLE('',#4810,0.5);
#342=CIRCLE('',#4811,6.5);
#343=CIRCLE('',#4812,6.);
#344=CIRCLE('',#4814,0.5);
#345=CIRCLE('',#4815,4.5);
#346=CIRCLE('',#4817,0.5);
#347=CIRCLE('',#4818,30.5);
#348=CIRCLE('',#4820,0.5);
#349=CIRCLE('',#4821,4.5);
#350=CIRCLE('',#4823,0.5);
#351=CIRCLE('',#4824,6.);
#352=CIRCLE('',#4826,0.5);
#353=CIRCLE('',#4827,4.5);
#354=CIRCLE('',#4829,0.5);
#355=CIRCLE('',#4830,30.5);
#356=CIRCLE('',#4832,0.5);
#357=CIRCLE('',#4833,4.5);
#358=CIRCLE('',#4835,0.5);
#359=CIRCLE('',#4836,6.);
#360=CIRCLE('',#4838,0.5);
#361=CIRCLE('',#4839,4.5);
#362=CIRCLE('',#4841,0.5);
#363=CIRCLE('',#4842,30.5);
#364=CIRCLE('',#4844,0.5);
#365=CIRCLE('',#4845,4.5);
#366=CIRCLE('',#4847,0.5);
#367=CIRCLE('',#4848,6.);
#368=CIRCLE('',#4850,0.5);
#369=CIRCLE('',#4851,4.5);
#370=CIRCLE('',#4853,0.5);
#371=CIRCLE('',#4854,30.5);
#372=CIRCLE('',#4856,0.5);
#373=CIRCLE('',#4857,4.5);
#374=CIRCLE('',#4859,0.5);
#375=CIRCLE('',#4860,6.);
#376=CIRCLE('',#4862,0.5);
#377=CIRCLE('',#4863,4.);
#378=CIRCLE('',#4864,4.5);
#379=CIRCLE('',#4866,0.5);
#380=CIRCLE('',#4867,30.5);
#381=CIRCLE('',#4869,0.5);
#382=CIRCLE('',#4870,4.5);
#383=CIRCLE('',#4872,0.5);
#384=CIRCLE('',#4873,6.5);
#385=CIRCLE('',#4874,6.);
#386=CIRCLE('',#4876,0.5);
#387=CIRCLE('',#4877,4.);
#388=CIRCLE('',#4878,4.5);
#389=CIRCLE('',#4880,0.5);
#390=CIRCLE('',#4881,31.);
#391=CIRCLE('',#4882,30.5);
#392=CIRCLE('',#4884,0.5);
#393=CIRCLE('',#4885,4.);
#394=CIRCLE('',#4886,4.5);
#395=CIRCLE('',#4888,0.5);
#396=CIRCLE('',#4889,6.5);
#397=CIRCLE('',#4890,6.);
#398=CIRCLE('',#4892,0.5);
#399=CIRCLE('',#4893,4.);
#400=CIRCLE('',#4894,4.5);
#401=CIRCLE('',#4896,0.5);
#402=CIRCLE('',#4897,31.);
#403=CIRCLE('',#4898,30.5);
#404=CIRCLE('',#4900,0.5);
#405=CIRCLE('',#4901,4.);
#406=CIRCLE('',#4902,4.5);
#407=CIRCLE('',#4904,0.5);
#408=CIRCLE('',#4905,6.5);
#409=CIRCLE('',#4906,6.);
#410=CIRCLE('',#4908,0.5);
#411=CIRCLE('',#4909,4.);
#412=CIRCLE('',#4910,4.5);
#413=CIRCLE('',#4912,30.5);
#414=CIRCLE('',#4913,31.);
#415=CIRCLE('',#4929,28.5);
#416=CIRCLE('',#4930,1.5);
#417=CIRCLE('',#4931,1.5);
#418=CIRCLE('',#4932,1.5);
#419=CIRCLE('',#4933,1.5);
#420=CIRCLE('',#4934,1.5);
#421=CIRCLE('',#4935,1.5);
#422=CIRCLE('',#4936,1.5);
#423=CIRCLE('',#4937,1.5);
#424=CIRCLE('',#4939,0.5);
#425=CIRCLE('',#4940,28.);
#426=CIRCLE('',#4941,28.);
#427=CIRCLE('',#4943,28.);
#428=CIRCLE('',#4944,28.);
#429=CIRCLE('',#4946,0.5);
#430=CIRCLE('',#4961,241.305156942645);
#431=CIRCLE('',#4962,241.305156942645);
#432=CIRCLE('',#4963,241.305156942645);
#433=CIRCLE('',#4964,241.305156942645);
#434=CIRCLE('',#4967,238.305156942645);
#435=CIRCLE('',#4968,238.305156942645);
#436=CIRCLE('',#4969,238.305156942645);
#437=CIRCLE('',#4970,238.305156942645);
#438=CIRCLE('',#4975,5.);
#439=CIRCLE('',#4979,5.);
#440=CIRCLE('',#4982,5.);
#441=CIRCLE('',#4983,5.);
#442=CIRCLE('',#4987,6.);
#443=CIRCLE('',#4988,6.);
#444=CIRCLE('',#4991,6.);
#445=CIRCLE('',#4992,6.);
#446=TOROIDAL_SURFACE('',#4483,25.5,0.5);
#447=TOROIDAL_SURFACE('',#4493,27.5,0.5);
#448=TOROIDAL_SURFACE('',#4500,27.5,0.5);
#449=TOROIDAL_SURFACE('',#4505,25.5,0.5);
#450=TOROIDAL_SURFACE('',#4639,4.5,0.5);
#451=TOROIDAL_SURFACE('',#4643,6.,0.5);
#452=TOROIDAL_SURFACE('',#4647,4.5,0.5);
#453=TOROIDAL_SURFACE('',#4651,30.5,0.5);
#454=TOROIDAL_SURFACE('',#4655,4.5,0.5);
#455=TOROIDAL_SURFACE('',#4659,6.,0.5);
#456=TOROIDAL_SURFACE('',#4663,4.5,0.5);
#457=TOROIDAL_SURFACE('',#4667,30.5,0.5);
#458=TOROIDAL_SURFACE('',#4671,4.5,0.5);
#459=TOROIDAL_SURFACE('',#4675,6.,0.5);
#460=TOROIDAL_SURFACE('',#4679,4.5,0.5);
#461=TOROIDAL_SURFACE('',#4683,30.5,0.5);
#462=TOROIDAL_SURFACE('',#4687,4.5,0.5);
#463=TOROIDAL_SURFACE('',#4691,6.,0.5);
#464=TOROIDAL_SURFACE('',#4695,4.5,0.5);
#465=TOROIDAL_SURFACE('',#4698,30.5,0.5);
#466=TOROIDAL_SURFACE('',#4702,4.5,0.5);
#467=TOROIDAL_SURFACE('',#4706,6.,0.5);
#468=TOROIDAL_SURFACE('',#4710,4.5,0.5);
#469=TOROIDAL_SURFACE('',#4714,30.5,0.5);
#470=TOROIDAL_SURFACE('',#4718,4.5,0.5);
#471=TOROIDAL_SURFACE('',#4722,6.,0.5);
#472=TOROIDAL_SURFACE('',#4726,4.5,0.5);
#473=TOROIDAL_SURFACE('',#4730,30.5,0.5);
#474=TOROIDAL_SURFACE('',#4734,4.5,0.5);
#475=TOROIDAL_SURFACE('',#4738,6.,0.5);
#476=TOROIDAL_SURFACE('',#4742,4.5,0.5);
#477=TOROIDAL_SURFACE('',#4746,30.5,0.5);
#478=TOROIDAL_SURFACE('',#4750,4.5,0.5);
#479=TOROIDAL_SURFACE('',#4754,6.,0.5);
#480=TOROIDAL_SURFACE('',#4758,4.5,0.5);
#481=TOROIDAL_SURFACE('',#4762,30.5,0.5);
#482=TOROIDAL_SURFACE('',#4804,4.5,0.5);
#483=TOROIDAL_SURFACE('',#4809,6.,0.5);
#484=TOROIDAL_SURFACE('',#4813,4.5,0.5);
#485=TOROIDAL_SURFACE('',#4816,30.5,0.5);
#486=TOROIDAL_SURFACE('',#4819,4.5,0.5);
#487=TOROIDAL_SURFACE('',#4822,6.,0.5);
#488=TOROIDAL_SURFACE('',#4825,4.5,0.5);
#489=TOROIDAL_SURFACE('',#4828,30.5,0.5);
#490=TOROIDAL_SURFACE('',#4831,4.5,0.5);
#491=TOROIDAL_SURFACE('',#4834,6.,0.5);
#492=TOROIDAL_SURFACE('',#4837,4.5,0.5);
#493=TOROIDAL_SURFACE('',#4840,30.5,0.5);
#494=TOROIDAL_SURFACE('',#4843,4.5,0.5);
#495=TOROIDAL_SURFACE('',#4846,6.,0.5);
#496=TOROIDAL_SURFACE('',#4849,4.5,0.5);
#497=TOROIDAL_SURFACE('',#4852,30.5,0.5);
#498=TOROIDAL_SURFACE('',#4855,4.5,0.5);
#499=TOROIDAL_SURFACE('',#4858,6.,0.5);
#500=TOROIDAL_SURFACE('',#4861,4.5,0.5);
#501=TOROIDAL_SURFACE('',#4865,30.5,0.5);
#502=TOROIDAL_SURFACE('',#4868,4.5,0.5);
#503=TOROIDAL_SURFACE('',#4871,6.,0.5);
#504=TOROIDAL_SURFACE('',#4875,4.5,0.5);
#505=TOROIDAL_SURFACE('',#4879,30.5,0.5);
#506=TOROIDAL_SURFACE('',#4883,4.5,0.5);
#507=TOROIDAL_SURFACE('',#4887,6.,0.5);
#508=TOROIDAL_SURFACE('',#4891,4.5,0.5);
#509=TOROIDAL_SURFACE('',#4895,30.5,0.5);
#510=TOROIDAL_SURFACE('',#4899,4.5,0.5);
#511=TOROIDAL_SURFACE('',#4903,6.,0.5);
#512=TOROIDAL_SURFACE('',#4907,4.5,0.5);
#513=TOROIDAL_SURFACE('',#4911,30.5,0.5);
#514=TOROIDAL_SURFACE('',#4938,28.5,0.5);
#515=TOROIDAL_SURFACE('',#4945,28.5,0.5);
#516=FACE_OUTER_BOUND('',#747,.T.);
#517=FACE_OUTER_BOUND('',#748,.T.);
#518=FACE_OUTER_BOUND('',#749,.T.);
#519=FACE_OUTER_BOUND('',#750,.T.);
#520=FACE_OUTER_BOUND('',#752,.T.);
#521=FACE_OUTER_BOUND('',#755,.T.);
#522=FACE_OUTER_BOUND('',#756,.T.);
#523=FACE_OUTER_BOUND('',#759,.T.);
#524=FACE_OUTER_BOUND('',#760,.T.);
#525=FACE_OUTER_BOUND('',#762,.T.);
#526=FACE_OUTER_BOUND('',#763,.T.);
#527=FACE_OUTER_BOUND('',#764,.T.);
#528=FACE_OUTER_BOUND('',#765,.T.);
#529=FACE_OUTER_BOUND('',#766,.T.);
#530=FACE_OUTER_BOUND('',#767,.T.);
#531=FACE_OUTER_BOUND('',#768,.T.);
#532=FACE_OUTER_BOUND('',#770,.T.);
#533=FACE_OUTER_BOUND('',#772,.T.);
#534=FACE_OUTER_BOUND('',#773,.T.);
#535=FACE_OUTER_BOUND('',#774,.T.);
#536=FACE_OUTER_BOUND('',#775,.T.);
#537=FACE_OUTER_BOUND('',#776,.T.);
#538=FACE_OUTER_BOUND('',#777,.T.);
#539=FACE_OUTER_BOUND('',#778,.T.);
#540=FACE_OUTER_BOUND('',#779,.T.);
#541=FACE_OUTER_BOUND('',#780,.T.);
#542=FACE_OUTER_BOUND('',#781,.T.);
#543=FACE_OUTER_BOUND('',#782,.T.);
#544=FACE_OUTER_BOUND('',#783,.T.);
#545=FACE_OUTER_BOUND('',#784,.T.);
#546=FACE_OUTER_BOUND('',#785,.T.);
#547=FACE_OUTER_BOUND('',#786,.T.);
#548=FACE_OUTER_BOUND('',#787,.T.);
#549=FACE_OUTER_BOUND('',#788,.T.);
#550=FACE_OUTER_BOUND('',#789,.T.);
#551=FACE_OUTER_BOUND('',#790,.T.);
#552=FACE_OUTER_BOUND('',#791,.T.);
#553=FACE_OUTER_BOUND('',#792,.T.);
#554=FACE_OUTER_BOUND('',#793,.T.);
#555=FACE_OUTER_BOUND('',#794,.T.);
#556=FACE_OUTER_BOUND('',#796,.T.);
#557=FACE_OUTER_BOUND('',#798,.T.);
#558=FACE_OUTER_BOUND('',#799,.T.);
#559=FACE_OUTER_BOUND('',#801,.T.);
#560=FACE_OUTER_BOUND('',#802,.T.);
#561=FACE_OUTER_BOUND('',#803,.T.);
#562=FACE_OUTER_BOUND('',#804,.T.);
#563=FACE_OUTER_BOUND('',#805,.T.);
#564=FACE_OUTER_BOUND('',#806,.T.);
#565=FACE_OUTER_BOUND('',#807,.T.);
#566=FACE_OUTER_BOUND('',#808,.T.);
#567=FACE_OUTER_BOUND('',#809,.T.);
#568=FACE_OUTER_BOUND('',#810,.T.);
#569=FACE_OUTER_BOUND('',#811,.T.);
#570=FACE_OUTER_BOUND('',#812,.T.);
#571=FACE_OUTER_BOUND('',#813,.T.);
#572=FACE_OUTER_BOUND('',#814,.T.);
#573=FACE_OUTER_BOUND('',#815,.T.);
#574=FACE_OUTER_BOUND('',#816,.T.);
#575=FACE_OUTER_BOUND('',#817,.T.);
#576=FACE_OUTER_BOUND('',#819,.T.);
#577=FACE_OUTER_BOUND('',#820,.T.);
#578=FACE_OUTER_BOUND('',#821,.T.);
#579=FACE_OUTER_BOUND('',#822,.T.);
#580=FACE_OUTER_BOUND('',#823,.T.);
#581=FACE_OUTER_BOUND('',#824,.T.);
#582=FACE_OUTER_BOUND('',#825,.T.);
#583=FACE_OUTER_BOUND('',#826,.T.);
#584=FACE_OUTER_BOUND('',#827,.T.);
#585=FACE_OUTER_BOUND('',#828,.T.);
#586=FACE_OUTER_BOUND('',#829,.T.);
#587=FACE_OUTER_BOUND('',#830,.T.);
#588=FACE_OUTER_BOUND('',#831,.T.);
#589=FACE_OUTER_BOUND('',#832,.T.);
#590=FACE_OUTER_BOUND('',#833,.T.);
#591=FACE_OUTER_BOUND('',#834,.T.);
#592=FACE_OUTER_BOUND('',#835,.T.);
#593=FACE_OUTER_BOUND('',#836,.T.);
#594=FACE_OUTER_BOUND('',#837,.T.);
#595=FACE_OUTER_BOUND('',#838,.T.);
#596=FACE_OUTER_BOUND('',#840,.T.);
#597=FACE_OUTER_BOUND('',#841,.T.);
#598=FACE_OUTER_BOUND('',#842,.T.);
#599=FACE_OUTER_BOUND('',#843,.T.);
#600=FACE_OUTER_BOUND('',#844,.T.);
#601=FACE_OUTER_BOUND('',#845,.T.);
#602=FACE_OUTER_BOUND('',#846,.T.);
#603=FACE_OUTER_BOUND('',#847,.T.);
#604=FACE_OUTER_BOUND('',#848,.T.);
#605=FACE_OUTER_BOUND('',#849,.T.);
#606=FACE_OUTER_BOUND('',#850,.T.);
#607=FACE_OUTER_BOUND('',#851,.T.);
#608=FACE_OUTER_BOUND('',#852,.T.);
#609=FACE_OUTER_BOUND('',#853,.T.);
#610=FACE_OUTER_BOUND('',#854,.T.);
#611=FACE_OUTER_BOUND('',#856,.T.);
#612=FACE_OUTER_BOUND('',#857,.T.);
#613=FACE_OUTER_BOUND('',#859,.T.);
#614=FACE_OUTER_BOUND('',#860,.T.);
#615=FACE_OUTER_BOUND('',#861,.T.);
#616=FACE_OUTER_BOUND('',#862,.T.);
#617=FACE_OUTER_BOUND('',#863,.T.);
#618=FACE_OUTER_BOUND('',#864,.T.);
#619=FACE_OUTER_BOUND('',#865,.T.);
#620=FACE_OUTER_BOUND('',#866,.T.);
#621=FACE_OUTER_BOUND('',#867,.T.);
#622=FACE_OUTER_BOUND('',#868,.T.);
#623=FACE_OUTER_BOUND('',#869,.T.);
#624=FACE_OUTER_BOUND('',#870,.T.);
#625=FACE_OUTER_BOUND('',#871,.T.);
#626=FACE_OUTER_BOUND('',#872,.T.);
#627=FACE_OUTER_BOUND('',#873,.T.);
#628=FACE_OUTER_BOUND('',#874,.T.);
#629=FACE_OUTER_BOUND('',#875,.T.);
#630=FACE_OUTER_BOUND('',#876,.T.);
#631=FACE_OUTER_BOUND('',#877,.T.);
#632=FACE_OUTER_BOUND('',#878,.T.);
#633=FACE_OUTER_BOUND('',#879,.T.);
#634=FACE_OUTER_BOUND('',#880,.T.);
#635=FACE_OUTER_BOUND('',#881,.T.);
#636=FACE_OUTER_BOUND('',#882,.T.);
#637=FACE_OUTER_BOUND('',#883,.T.);
#638=FACE_OUTER_BOUND('',#884,.T.);
#639=FACE_OUTER_BOUND('',#885,.T.);
#640=FACE_OUTER_BOUND('',#886,.T.);
#641=FACE_OUTER_BOUND('',#887,.T.);
#642=FACE_OUTER_BOUND('',#888,.T.);
#643=FACE_OUTER_BOUND('',#889,.T.);
#644=FACE_OUTER_BOUND('',#890,.T.);
#645=FACE_OUTER_BOUND('',#891,.T.);
#646=FACE_OUTER_BOUND('',#892,.T.);
#647=FACE_OUTER_BOUND('',#893,.T.);
#648=FACE_OUTER_BOUND('',#894,.T.);
#649=FACE_OUTER_BOUND('',#895,.T.);
#650=FACE_OUTER_BOUND('',#896,.T.);
#651=FACE_OUTER_BOUND('',#897,.T.);
#652=FACE_OUTER_BOUND('',#898,.T.);
#653=FACE_OUTER_BOUND('',#899,.T.);
#654=FACE_OUTER_BOUND('',#900,.T.);
#655=FACE_OUTER_BOUND('',#901,.T.);
#656=FACE_OUTER_BOUND('',#902,.T.);
#657=FACE_OUTER_BOUND('',#903,.T.);
#658=FACE_OUTER_BOUND('',#904,.T.);
#659=FACE_OUTER_BOUND('',#905,.T.);
#660=FACE_OUTER_BOUND('',#906,.T.);
#661=FACE_OUTER_BOUND('',#907,.T.);
#662=FACE_OUTER_BOUND('',#908,.T.);
#663=FACE_OUTER_BOUND('',#909,.T.);
#664=FACE_OUTER_BOUND('',#910,.T.);
#665=FACE_OUTER_BOUND('',#911,.T.);
#666=FACE_OUTER_BOUND('',#912,.T.);
#667=FACE_OUTER_BOUND('',#913,.T.);
#668=FACE_OUTER_BOUND('',#923,.T.);
#669=FACE_OUTER_BOUND('',#924,.T.);
#670=FACE_OUTER_BOUND('',#925,.T.);
#671=FACE_OUTER_BOUND('',#926,.T.);
#672=FACE_OUTER_BOUND('',#927,.T.);
#673=FACE_OUTER_BOUND('',#928,.T.);
#674=FACE_OUTER_BOUND('',#929,.T.);
#675=FACE_OUTER_BOUND('',#930,.T.);
#676=FACE_OUTER_BOUND('',#931,.T.);
#677=FACE_OUTER_BOUND('',#932,.T.);
#678=FACE_OUTER_BOUND('',#933,.T.);
#679=FACE_OUTER_BOUND('',#934,.T.);
#680=FACE_OUTER_BOUND('',#935,.T.);
#681=FACE_OUTER_BOUND('',#936,.T.);
#682=FACE_OUTER_BOUND('',#937,.T.);
#683=FACE_OUTER_BOUND('',#938,.T.);
#684=FACE_OUTER_BOUND('',#939,.T.);
#685=FACE_OUTER_BOUND('',#940,.T.);
#686=FACE_OUTER_BOUND('',#941,.T.);
#687=FACE_OUTER_BOUND('',#942,.T.);
#688=FACE_OUTER_BOUND('',#943,.T.);
#689=FACE_OUTER_BOUND('',#944,.T.);
#690=FACE_OUTER_BOUND('',#945,.T.);
#691=FACE_OUTER_BOUND('',#946,.T.);
#692=FACE_OUTER_BOUND('',#947,.T.);
#693=FACE_OUTER_BOUND('',#948,.T.);
#694=FACE_OUTER_BOUND('',#949,.T.);
#695=FACE_OUTER_BOUND('',#950,.T.);
#696=FACE_OUTER_BOUND('',#951,.T.);
#697=FACE_OUTER_BOUND('',#952,.T.);
#698=FACE_OUTER_BOUND('',#953,.T.);
#699=FACE_OUTER_BOUND('',#954,.T.);
#700=FACE_OUTER_BOUND('',#955,.T.);
#701=FACE_OUTER_BOUND('',#956,.T.);
#702=FACE_OUTER_BOUND('',#957,.T.);
#703=FACE_OUTER_BOUND('',#958,.T.);
#704=FACE_OUTER_BOUND('',#959,.T.);
#705=FACE_OUTER_BOUND('',#960,.T.);
#706=FACE_OUTER_BOUND('',#961,.T.);
#707=FACE_OUTER_BOUND('',#962,.T.);
#708=FACE_OUTER_BOUND('',#963,.T.);
#709=FACE_OUTER_BOUND('',#964,.T.);
#710=FACE_OUTER_BOUND('',#965,.T.);
#711=FACE_OUTER_BOUND('',#966,.T.);
#712=FACE_OUTER_BOUND('',#967,.T.);
#713=FACE_OUTER_BOUND('',#968,.T.);
#714=FACE_OUTER_BOUND('',#969,.T.);
#715=FACE_OUTER_BOUND('',#979,.T.);
#716=FACE_OUTER_BOUND('',#980,.T.);
#717=FACE_OUTER_BOUND('',#983,.T.);
#718=FACE_OUTER_BOUND('',#984,.T.);
#719=FACE_OUTER_BOUND('',#985,.T.);
#720=FACE_OUTER_BOUND('',#986,.T.);
#721=FACE_OUTER_BOUND('',#987,.T.);
#722=FACE_OUTER_BOUND('',#988,.T.);
#723=FACE_OUTER_BOUND('',#989,.T.);
#724=FACE_OUTER_BOUND('',#990,.T.);
#725=FACE_OUTER_BOUND('',#991,.T.);
#726=FACE_OUTER_BOUND('',#992,.T.);
#727=FACE_OUTER_BOUND('',#993,.T.);
#728=FACE_OUTER_BOUND('',#994,.T.);
#729=FACE_OUTER_BOUND('',#995,.T.);
#730=FACE_OUTER_BOUND('',#996,.T.);
#731=FACE_OUTER_BOUND('',#997,.T.);
#732=FACE_OUTER_BOUND('',#998,.T.);
#733=FACE_OUTER_BOUND('',#999,.T.);
#734=FACE_OUTER_BOUND('',#1000,.T.);
#735=FACE_OUTER_BOUND('',#1001,.T.);
#736=FACE_OUTER_BOUND('',#1002,.T.);
#737=FACE_OUTER_BOUND('',#1003,.T.);
#738=FACE_OUTER_BOUND('',#1004,.T.);
#739=FACE_OUTER_BOUND('',#1005,.T.);
#740=FACE_OUTER_BOUND('',#1006,.T.);
#741=FACE_OUTER_BOUND('',#1007,.T.);
#742=FACE_OUTER_BOUND('',#1008,.T.);
#743=FACE_OUTER_BOUND('',#1009,.T.);
#744=FACE_OUTER_BOUND('',#1010,.T.);
#745=FACE_OUTER_BOUND('',#1011,.T.);
#746=FACE_OUTER_BOUND('',#1012,.T.);
#747=EDGE_LOOP('',(#2683,#2684,#2685,#2686,#2687,#2688));
#748=EDGE_LOOP('',(#2689,#2690,#2691,#2692,#2693,#2694));
#749=EDGE_LOOP('',(#2695,#2696,#2697,#2698,#2699));
#750=EDGE_LOOP('',(#2700));
#751=EDGE_LOOP('',(#2701));
#752=EDGE_LOOP('',(#2702,#2703,#2704,#2705,#2706,#2707));
#753=EDGE_LOOP('',(#2708,#2709));
#754=EDGE_LOOP('',(#2710,#2711));
#755=EDGE_LOOP('',(#2712,#2713,#2714,#2715,#2716));
#756=EDGE_LOOP('',(#2717,#2718,#2719,#2720,#2721,#2722));
#757=EDGE_LOOP('',(#2723,#2724));
#758=EDGE_LOOP('',(#2725,#2726));
#759=EDGE_LOOP('',(#2727,#2728,#2729,#2730,#2731));
#760=EDGE_LOOP('',(#2732));
#761=EDGE_LOOP('',(#2733));
#762=EDGE_LOOP('',(#2734,#2735,#2736,#2737,#2738));
#763=EDGE_LOOP('',(#2739,#2740,#2741,#2742));
#764=EDGE_LOOP('',(#2743));
#765=EDGE_LOOP('',(#2744));
#766=EDGE_LOOP('',(#2745,#2746,#2747,#2748));
#767=EDGE_LOOP('',(#2749,#2750,#2751,#2752));
#768=EDGE_LOOP('',(#2753));
#769=EDGE_LOOP('',(#2754));
#770=EDGE_LOOP('',(#2755));
#771=EDGE_LOOP('',(#2756));
#772=EDGE_LOOP('',(#2757,#2758,#2759,#2760));
#773=EDGE_LOOP('',(#2761,#2762,#2763,#2764,#2765,#2766));
#774=EDGE_LOOP('',(#2767,#2768,#2769,#2770,#2771,#2772));
#775=EDGE_LOOP('',(#2773,#2774,#2775,#2776,#2777,#2778));
#776=EDGE_LOOP('',(#2779,#2780,#2781,#2782,#2783,#2784));
#777=EDGE_LOOP('',(#2785,#2786,#2787,#2788,#2789,#2790));
#778=EDGE_LOOP('',(#2791,#2792,#2793,#2794,#2795,#2796));
#779=EDGE_LOOP('',(#2797,#2798,#2799,#2800,#2801,#2802));
#780=EDGE_LOOP('',(#2803,#2804,#2805,#2806,#2807,#2808));
#781=EDGE_LOOP('',(#2809,#2810,#2811,#2812,#2813,#2814));
#782=EDGE_LOOP('',(#2815,#2816,#2817,#2818,#2819,#2820));
#783=EDGE_LOOP('',(#2821,#2822,#2823,#2824,#2825));
#784=EDGE_LOOP('',(#2826,#2827,#2828,#2829,#2830,#2831));
#785=EDGE_LOOP('',(#2832,#2833,#2834,#2835,#2836));
#786=EDGE_LOOP('',(#2837,#2838,#2839,#2840,#2841,#2842));
#787=EDGE_LOOP('',(#2843,#2844,#2845,#2846,#2847,#2848,#2849,#2850));
#788=EDGE_LOOP('',(#2851,#2852,#2853,#2854,#2855));
#789=EDGE_LOOP('',(#2856,#2857,#2858,#2859,#2860,#2861));
#790=EDGE_LOOP('',(#2862,#2863,#2864,#2865,#2866,#2867,#2868,#2869,#2870,
#2871,#2872,#2873,#2874,#2875,#2876,#2877,#2878,#2879,#2880,#2881,#2882,
#2883,#2884,#2885,#2886,#2887,#2888,#2889,#2890,#2891,#2892,#2893,#2894,
#2895,#2896,#2897));
#791=EDGE_LOOP('',(#2898,#2899,#2900,#2901,#2902));
#792=EDGE_LOOP('',(#2903,#2904,#2905,#2906,#2907,#2908,#2909,#2910,#2911,
#2912,#2913,#2914,#2915,#2916,#2917,#2918,#2919,#2920,#2921,#2922,#2923,
#2924,#2925,#2926,#2927,#2928,#2929,#2930,#2931,#2932,#2933,#2934,#2935));
#793=EDGE_LOOP('',(#2936,#2937,#2938,#2939));
#794=EDGE_LOOP('',(#2940));
#795=EDGE_LOOP('',(#2941));
#796=EDGE_LOOP('',(#2942));
#797=EDGE_LOOP('',(#2943));
#798=EDGE_LOOP('',(#2944,#2945,#2946,#2947));
#799=EDGE_LOOP('',(#2948));
#800=EDGE_LOOP('',(#2949,#2950,#2951,#2952));
#801=EDGE_LOOP('',(#2953,#2954,#2955,#2956));
#802=EDGE_LOOP('',(#2957,#2958,#2959,#2960));
#803=EDGE_LOOP('',(#2961,#2962,#2963,#2964));
#804=EDGE_LOOP('',(#2965,#2966,#2967,#2968));
#805=EDGE_LOOP('',(#2969,#2970,#2971,#2972));
#806=EDGE_LOOP('',(#2973,#2974,#2975,#2976));
#807=EDGE_LOOP('',(#2977,#2978,#2979,#2980,#2981,#2982,#2983,#2984,#2985,
#2986,#2987,#2988,#2989,#2990,#2991,#2992,#2993,#2994));
#808=EDGE_LOOP('',(#2995,#2996,#2997,#2998));
#809=EDGE_LOOP('',(#2999,#3000,#3001,#3002));
#810=EDGE_LOOP('',(#3003,#3004,#3005,#3006,#3007,#3008));
#811=EDGE_LOOP('',(#3009,#3010,#3011,#3012,#3013,#3014,#3015,#3016,#3017,
#3018,#3019,#3020));
#812=EDGE_LOOP('',(#3021,#3022,#3023,#3024,#3025));
#813=EDGE_LOOP('',(#3026,#3027,#3028,#3029,#3030,#3031));
#814=EDGE_LOOP('',(#3032,#3033,#3034,#3035));
#815=EDGE_LOOP('',(#3036,#3037,#3038,#3039,#3040,#3041,#3042,#3043,#3044,
#3045,#3046,#3047,#3048,#3049,#3050,#3051,#3052,#3053));
#816=EDGE_LOOP('',(#3054,#3055,#3056,#3057,#3058,#3059,#3060,#3061,#3062,
#3063,#3064,#3065,#3066,#3067,#3068,#3069,#3070,#3071));
#817=EDGE_LOOP('',(#3072,#3073,#3074,#3075,#3076));
#818=EDGE_LOOP('',(#3077));
#819=EDGE_LOOP('',(#3078,#3079,#3080,#3081,#3082));
#820=EDGE_LOOP('',(#3083,#3084,#3085,#3086));
#821=EDGE_LOOP('',(#3087,#3088,#3089,#3090,#3091));
#822=EDGE_LOOP('',(#3092,#3093,#3094,#3095,#3096,#3097));
#823=EDGE_LOOP('',(#3098,#3099,#3100,#3101));
#824=EDGE_LOOP('',(#3102,#3103,#3104,#3105,#3106,#3107));
#825=EDGE_LOOP('',(#3108,#3109,#3110,#3111));
#826=EDGE_LOOP('',(#3112,#3113,#3114,#3115,#3116,#3117));
#827=EDGE_LOOP('',(#3118,#3119,#3120,#3121,#3122));
#828=EDGE_LOOP('',(#3123,#3124,#3125,#3126,#3127,#3128,#3129,#3130,#3131,
#3132,#3133,#3134,#3135,#3136,#3137,#3138,#3139,#3140,#3141,#3142,#3143));
#829=EDGE_LOOP('',(#3144,#3145,#3146,#3147,#3148));
#830=EDGE_LOOP('',(#3149,#3150,#3151,#3152));
#831=EDGE_LOOP('',(#3153,#3154,#3155,#3156,#3157,#3158));
#832=EDGE_LOOP('',(#3159,#3160,#3161,#3162,#3163,#3164,#3165,#3166,#3167,
#3168,#3169,#3170));
#833=EDGE_LOOP('',(#3171,#3172,#3173,#3174,#3175));
#834=EDGE_LOOP('',(#3176,#3177,#3178,#3179));
#835=EDGE_LOOP('',(#3180,#3181,#3182,#3183,#3184,#3185));
#836=EDGE_LOOP('',(#3186,#3187,#3188,#3189,#3190,#3191,#3192,#3193,#3194,
#3195,#3196,#3197,#3198,#3199,#3200,#3201,#3202,#3203,#3204,#3205,#3206,
#3207,#3208,#3209,#3210,#3211));
#837=EDGE_LOOP('',(#3212,#3213,#3214,#3215,#3216,#3217,#3218,#3219,#3220,
#3221,#3222,#3223,#3224,#3225,#3226,#3227,#3228,#3229,#3230,#3231,#3232,
#3233,#3234,#3235,#3236,#3237));
#838=EDGE_LOOP('',(#3238,#3239,#3240,#3241,#3242));
#839=EDGE_LOOP('',(#3243));
#840=EDGE_LOOP('',(#3244,#3245,#3246,#3247,#3248));
#841=EDGE_LOOP('',(#3249,#3250,#3251,#3252));
#842=EDGE_LOOP('',(#3253,#3254,#3255,#3256,#3257,#3258));
#843=EDGE_LOOP('',(#3259,#3260,#3261,#3262,#3263,#3264));
#844=EDGE_LOOP('',(#3265,#3266,#3267,#3268,#3269,#3270));
#845=EDGE_LOOP('',(#3271,#3272,#3273,#3274,#3275,#3276));
#846=EDGE_LOOP('',(#3277,#3278,#3279,#3280,#3281,#3282));
#847=EDGE_LOOP('',(#3283,#3284,#3285,#3286,#3287,#3288));
#848=EDGE_LOOP('',(#3289,#3290,#3291,#3292,#3293,#3294));
#849=EDGE_LOOP('',(#3295,#3296,#3297,#3298,#3299,#3300));
#850=EDGE_LOOP('',(#3301,#3302,#3303,#3304,#3305,#3306,#3307,#3308,#3309,
#3310,#3311,#3312,#3313,#3314,#3315));
#851=EDGE_LOOP('',(#3316,#3317,#3318,#3319,#3320,#3321));
#852=EDGE_LOOP('',(#3322,#3323,#3324,#3325,#3326,#3327,#3328,#3329,#3330,
#3331,#3332,#3333,#3334,#3335,#3336,#3337,#3338,#3339,#3340,#3341,#3342,
#3343,#3344,#3345,#3346,#3347,#3348,#3349));
#853=EDGE_LOOP('',(#3350,#3351,#3352,#3353,#3354,#3355,#3356,#3357,#3358,
#3359,#3360,#3361,#3362,#3363,#3364,#3365,#3366,#3367,#3368,#3369,#3370,
#3371,#3372,#3373,#3374,#3375,#3376));
#854=EDGE_LOOP('',(#3377,#3378));
#855=EDGE_LOOP('',(#3379,#3380,#3381,#3382));
#856=EDGE_LOOP('',(#3383,#3384,#3385,#3386,#3387,#3388,#3389,#3390));
#857=EDGE_LOOP('',(#3391));
#858=EDGE_LOOP('',(#3392,#3393,#3394,#3395));
#859=EDGE_LOOP('',(#3396,#3397));
#860=EDGE_LOOP('',(#3398,#3399));
#861=EDGE_LOOP('',(#3400,#3401,#3402,#3403,#3404,#3405,#3406,#3407));
#862=EDGE_LOOP('',(#3408,#3409,#3410,#3411,#3412,#3413,#3414));
#863=EDGE_LOOP('',(#3415,#3416,#3417,#3418));
#864=EDGE_LOOP('',(#3419,#3420,#3421,#3422,#3423,#3424,#3425));
#865=EDGE_LOOP('',(#3426,#3427,#3428,#3429));
#866=EDGE_LOOP('',(#3430,#3431,#3432,#3433));
#867=EDGE_LOOP('',(#3434,#3435,#3436,#3437));
#868=EDGE_LOOP('',(#3438,#3439,#3440,#3441));
#869=EDGE_LOOP('',(#3442,#3443,#3444,#3445));
#870=EDGE_LOOP('',(#3446,#3447,#3448,#3449));
#871=EDGE_LOOP('',(#3450,#3451,#3452,#3453));
#872=EDGE_LOOP('',(#3454,#3455,#3456,#3457));
#873=EDGE_LOOP('',(#3458,#3459,#3460,#3461));
#874=EDGE_LOOP('',(#3462,#3463,#3464,#3465));
#875=EDGE_LOOP('',(#3466,#3467,#3468,#3469));
#876=EDGE_LOOP('',(#3470,#3471,#3472,#3473));
#877=EDGE_LOOP('',(#3474,#3475,#3476,#3477));
#878=EDGE_LOOP('',(#3478,#3479,#3480,#3481));
#879=EDGE_LOOP('',(#3482,#3483,#3484,#3485));
#880=EDGE_LOOP('',(#3486,#3487,#3488,#3489));
#881=EDGE_LOOP('',(#3490,#3491,#3492,#3493));
#882=EDGE_LOOP('',(#3494,#3495,#3496,#3497));
#883=EDGE_LOOP('',(#3498,#3499,#3500,#3501));
#884=EDGE_LOOP('',(#3502,#3503,#3504,#3505));
#885=EDGE_LOOP('',(#3506,#3507,#3508,#3509));
#886=EDGE_LOOP('',(#3510,#3511,#3512,#3513));
#887=EDGE_LOOP('',(#3514,#3515,#3516,#3517));
#888=EDGE_LOOP('',(#3518,#3519,#3520,#3521));
#889=EDGE_LOOP('',(#3522,#3523,#3524,#3525));
#890=EDGE_LOOP('',(#3526,#3527,#3528,#3529));
#891=EDGE_LOOP('',(#3530,#3531,#3532,#3533));
#892=EDGE_LOOP('',(#3534,#3535,#3536,#3537));
#893=EDGE_LOOP('',(#3538,#3539,#3540,#3541));
#894=EDGE_LOOP('',(#3542,#3543,#3544,#3545));
#895=EDGE_LOOP('',(#3546,#3547,#3548,#3549));
#896=EDGE_LOOP('',(#3550,#3551,#3552,#3553));
#897=EDGE_LOOP('',(#3554,#3555,#3556,#3557));
#898=EDGE_LOOP('',(#3558,#3559,#3560,#3561));
#899=EDGE_LOOP('',(#3562,#3563,#3564,#3565));
#900=EDGE_LOOP('',(#3566,#3567,#3568,#3569));
#901=EDGE_LOOP('',(#3570,#3571,#3572,#3573));
#902=EDGE_LOOP('',(#3574,#3575,#3576,#3577));
#903=EDGE_LOOP('',(#3578,#3579,#3580,#3581));
#904=EDGE_LOOP('',(#3582,#3583,#3584,#3585));
#905=EDGE_LOOP('',(#3586,#3587,#3588,#3589));
#906=EDGE_LOOP('',(#3590,#3591,#3592,#3593));
#907=EDGE_LOOP('',(#3594,#3595,#3596,#3597));
#908=EDGE_LOOP('',(#3598,#3599,#3600,#3601));
#909=EDGE_LOOP('',(#3602,#3603,#3604,#3605));
#910=EDGE_LOOP('',(#3606,#3607,#3608,#3609));
#911=EDGE_LOOP('',(#3610,#3611,#3612,#3613,#3614,#3615));
#912=EDGE_LOOP('',(#3616,#3617,#3618,#3619));
#913=EDGE_LOOP('',(#3620,#3621,#3622,#3623,#3624,#3625,#3626,#3627,#3628,
#3629,#3630,#3631,#3632,#3633,#3634,#3635,#3636,#3637,#3638,#3639,#3640,
#3641,#3642,#3643,#3644,#3645,#3646,#3647,#3648,#3649,#3650,#3651));
#914=EDGE_LOOP('',(#3652));
#915=EDGE_LOOP('',(#3653));
#916=EDGE_LOOP('',(#3654));
#917=EDGE_LOOP('',(#3655));
#918=EDGE_LOOP('',(#3656));
#919=EDGE_LOOP('',(#3657));
#920=EDGE_LOOP('',(#3658));
#921=EDGE_LOOP('',(#3659));
#922=EDGE_LOOP('',(#3660));
#923=EDGE_LOOP('',(#3661,#3662,#3663,#3664));
#924=EDGE_LOOP('',(#3665,#3666,#3667,#3668));
#925=EDGE_LOOP('',(#3669,#3670,#3671,#3672));
#926=EDGE_LOOP('',(#3673,#3674,#3675,#3676));
#927=EDGE_LOOP('',(#3677,#3678,#3679,#3680));
#928=EDGE_LOOP('',(#3681,#3682,#3683,#3684));
#929=EDGE_LOOP('',(#3685,#3686,#3687,#3688));
#930=EDGE_LOOP('',(#3689,#3690,#3691,#3692));
#931=EDGE_LOOP('',(#3693,#3694,#3695,#3696));
#932=EDGE_LOOP('',(#3697,#3698,#3699,#3700));
#933=EDGE_LOOP('',(#3701,#3702,#3703,#3704));
#934=EDGE_LOOP('',(#3705,#3706,#3707,#3708));
#935=EDGE_LOOP('',(#3709,#3710,#3711,#3712));
#936=EDGE_LOOP('',(#3713,#3714,#3715,#3716));
#937=EDGE_LOOP('',(#3717,#3718,#3719,#3720));
#938=EDGE_LOOP('',(#3721,#3722,#3723,#3724));
#939=EDGE_LOOP('',(#3725,#3726,#3727,#3728));
#940=EDGE_LOOP('',(#3729,#3730,#3731,#3732));
#941=EDGE_LOOP('',(#3733,#3734,#3735,#3736));
#942=EDGE_LOOP('',(#3737,#3738,#3739,#3740));
#943=EDGE_LOOP('',(#3741,#3742,#3743,#3744));
#944=EDGE_LOOP('',(#3745,#3746,#3747,#3748));
#945=EDGE_LOOP('',(#3749,#3750,#3751,#3752));
#946=EDGE_LOOP('',(#3753,#3754,#3755,#3756));
#947=EDGE_LOOP('',(#3757,#3758,#3759,#3760));
#948=EDGE_LOOP('',(#3761,#3762,#3763,#3764));
#949=EDGE_LOOP('',(#3765,#3766,#3767,#3768));
#950=EDGE_LOOP('',(#3769,#3770,#3771,#3772));
#951=EDGE_LOOP('',(#3773,#3774,#3775,#3776));
#952=EDGE_LOOP('',(#3777,#3778,#3779,#3780));
#953=EDGE_LOOP('',(#3781,#3782,#3783,#3784));
#954=EDGE_LOOP('',(#3785,#3786,#3787,#3788));
#955=EDGE_LOOP('',(#3789,#3790,#3791,#3792,#3793,#3794));
#956=EDGE_LOOP('',(#3795,#3796,#3797,#3798));
#957=EDGE_LOOP('',(#3799,#3800,#3801,#3802));
#958=EDGE_LOOP('',(#3803,#3804,#3805,#3806));
#959=EDGE_LOOP('',(#3807,#3808,#3809,#3810));
#960=EDGE_LOOP('',(#3811,#3812,#3813,#3814));
#961=EDGE_LOOP('',(#3815,#3816,#3817,#3818));
#962=EDGE_LOOP('',(#3819,#3820,#3821,#3822));
#963=EDGE_LOOP('',(#3823,#3824,#3825,#3826));
#964=EDGE_LOOP('',(#3827,#3828,#3829,#3830));
#965=EDGE_LOOP('',(#3831,#3832,#3833,#3834));
#966=EDGE_LOOP('',(#3835,#3836,#3837,#3838));
#967=EDGE_LOOP('',(#3839,#3840,#3841,#3842));
#968=EDGE_LOOP('',(#3843,#3844,#3845,#3846));
#969=EDGE_LOOP('',(#3847,#3848,#3849,#3850,#3851,#3852,#3853,#3854,#3855,
#3856,#3857,#3858,#3859,#3860,#3861,#3862,#3863,#3864,#3865,#3866,#3867,
#3868,#3869,#3870,#3871,#3872,#3873,#3874,#3875,#3876,#3877,#3878));
#970=EDGE_LOOP('',(#3879));
#971=EDGE_LOOP('',(#3880));
#972=EDGE_LOOP('',(#3881));
#973=EDGE_LOOP('',(#3882));
#974=EDGE_LOOP('',(#3883));
#975=EDGE_LOOP('',(#3884));
#976=EDGE_LOOP('',(#3885));
#977=EDGE_LOOP('',(#3886));
#978=EDGE_LOOP('',(#3887));
#979=EDGE_LOOP('',(#3888,#3889,#3890,#3891,#3892));
#980=EDGE_LOOP('',(#3893,#3894,#3895,#3896,#3897,#3898));
#981=EDGE_LOOP('',(#3899));
#982=EDGE_LOOP('',(#3900,#3901));
#983=EDGE_LOOP('',(#3902,#3903,#3904,#3905,#3906));
#984=EDGE_LOOP('',(#3907,#3908,#3909,#3910));
#985=EDGE_LOOP('',(#3911,#3912,#3913,#3914));
#986=EDGE_LOOP('',(#3915,#3916,#3917,#3918));
#987=EDGE_LOOP('',(#3919,#3920,#3921,#3922));
#988=EDGE_LOOP('',(#3923,#3924,#3925,#3926));
#989=EDGE_LOOP('',(#3927,#3928,#3929,#3930));
#990=EDGE_LOOP('',(#3931,#3932,#3933,#3934));
#991=EDGE_LOOP('',(#3935,#3936,#3937,#3938));
#992=EDGE_LOOP('',(#3939,#3940,#3941,#3942));
#993=EDGE_LOOP('',(#3943,#3944,#3945,#3946,#3947,#3948));
#994=EDGE_LOOP('',(#3949,#3950,#3951,#3952,#3953,#3954));
#995=EDGE_LOOP('',(#3955,#3956,#3957,#3958));
#996=EDGE_LOOP('',(#3959,#3960,#3961,#3962,#3963,#3964));
#997=EDGE_LOOP('',(#3965,#3966,#3967,#3968));
#998=EDGE_LOOP('',(#3969,#3970,#3971,#3972));
#999=EDGE_LOOP('',(#3973,#3974,#3975,#3976));
#1000=EDGE_LOOP('',(#3977,#3978,#3979,#3980));
#1001=EDGE_LOOP('',(#3981,#3982,#3983,#3984));
#1002=EDGE_LOOP('',(#3985,#3986,#3987,#3988));
#1003=EDGE_LOOP('',(#3989,#3990,#3991,#3992));
#1004=EDGE_LOOP('',(#3993,#3994,#3995,#3996));
#1005=EDGE_LOOP('',(#3997,#3998,#3999,#4000,#4001,#4002));
#1006=EDGE_LOOP('',(#4003,#4004));
#1007=EDGE_LOOP('',(#4005,#4006,#4007,#4008));
#1008=EDGE_LOOP('',(#4009,#4010,#4011,#4012));
#1009=EDGE_LOOP('',(#4013,#4014,#4015,#4016));
#1010=EDGE_LOOP('',(#4017,#4018,#4019,#4020));
#1011=EDGE_LOOP('',(#4021,#4022,#4023,#4024));
#1012=EDGE_LOOP('',(#4025,#4026,#4027,#4028));
#1013=EDGE_LOOP('',(#4029,#4030,#4031,#4032,#4033,#4034,#4035,#4036));
#1014=LINE('',#6230,#1151);
#1015=LINE('',#6308,#1152);
#1016=LINE('',#6362,#1153);
#1017=LINE('',#6371,#1154);
#1018=LINE('',#6389,#1155);
#1019=LINE('',#6398,#1156);
#1020=LINE('',#6404,#1157);
#1021=LINE('',#6412,#1158);
#1022=LINE('',#6478,#1159);
#1023=LINE('',#6912,#1160);
#1024=LINE('',#7381,#1161);
#1025=LINE('',#7847,#1162);
#1026=LINE('',#8319,#1163);
#1027=LINE('',#8782,#1164);
#1028=LINE('',#9248,#1165);
#1029=LINE('',#9489,#1166);
#1030=LINE('',#9865,#1167);
#1031=LINE('',#10100,#1168);
#1032=LINE('',#10536,#1169);
#1033=LINE('',#10928,#1170);
#1034=LINE('',#11325,#1171);
#1035=LINE('',#11705,#1172);
#1036=LINE('',#11896,#1173);
#1037=LINE('',#11943,#1174);
#1038=LINE('',#13633,#1175);
#1039=LINE('',#13642,#1176);
#1040=LINE('',#13648,#1177);
#1041=LINE('',#13847,#1178);
#1042=LINE('',#14169,#1179);
#1043=LINE('',#14491,#1180);
#1044=LINE('',#14817,#1181);
#1045=LINE('',#15137,#1182);
#1046=LINE('',#18231,#1183);
#1047=LINE('',#18234,#1184);
#1048=LINE('',#18237,#1185);
#1049=LINE('',#18291,#1186);
#1050=LINE('',#18307,#1187);
#1051=LINE('',#18358,#1188);
#1052=LINE('',#18440,#1189);
#1053=LINE('',#19195,#1190);
#1054=LINE('',#19338,#1191);
#1055=LINE('',#19566,#1192);
#1056=LINE('',#19867,#1193);
#1057=LINE('',#20213,#1194);
#1058=LINE('',#20565,#1195);
#1059=LINE('',#20897,#1196);
#1060=LINE('',#21274,#1197);
#1061=LINE('',#24987,#1198);
#1062=LINE('',#24990,#1199);
#1063=LINE('',#24993,#1200);
#1064=LINE('',#25047,#1201);
#1065=LINE('',#25063,#1202);
#1066=LINE('',#25114,#1203);
#1067=LINE('',#25196,#1204);
#1068=LINE('',#26046,#1205);
#1069=LINE('',#26112,#1206);
#1070=LINE('',#26503,#1207);
#1071=LINE('',#26969,#1208);
#1072=LINE('',#27435,#1209);
#1073=LINE('',#27755,#1210);
#1074=LINE('',#28145,#1211);
#1075=LINE('',#28611,#1212);
#1076=LINE('',#29077,#1213);
#1077=LINE('',#33533,#1214);
#1078=LINE('',#33665,#1215);
#1079=LINE('',#33722,#1216);
#1080=LINE('',#33726,#1217);
#1081=LINE('',#33729,#1218);
#1082=LINE('',#33732,#1219);
#1083=LINE('',#33736,#1220);
#1084=LINE('',#33740,#1221);
#1085=LINE('',#33743,#1222);
#1086=LINE('',#33746,#1223);
#1087=LINE('',#33934,#1224);
#1088=LINE('',#33937,#1225);
#1089=LINE('',#33940,#1226);
#1090=LINE('',#33944,#1227);
#1091=LINE('',#33948,#1228);
#1092=LINE('',#33952,#1229);
#1093=LINE('',#33956,#1230);
#1094=LINE('',#33960,#1231);
#1095=LINE('',#33964,#1232);
#1096=LINE('',#33968,#1233);
#1097=LINE('',#33972,#1234);
#1098=LINE('',#33976,#1235);
#1099=LINE('',#33980,#1236);
#1100=LINE('',#33984,#1237);
#1101=LINE('',#33988,#1238);
#1102=LINE('',#34166,#1239);
#1103=LINE('',#34169,#1240);
#1104=LINE('',#34171,#1241);
#1105=LINE('',#34173,#1242);
#1106=LINE('',#34175,#1243);
#1107=LINE('',#34177,#1244);
#1108=LINE('',#34179,#1245);
#1109=LINE('',#34181,#1246);
#1110=LINE('',#34183,#1247);
#1111=LINE('',#34185,#1248);
#1112=LINE('',#34187,#1249);
#1113=LINE('',#34189,#1250);
#1114=LINE('',#34191,#1251);
#1115=LINE('',#34219,#1252);
#1116=LINE('',#34227,#1253);
#1117=LINE('',#34229,#1254);
#1118=LINE('',#34231,#1255);
#1119=LINE('',#34233,#1256);
#1120=LINE('',#34235,#1257);
#1121=LINE('',#34237,#1258);
#1122=LINE('',#34239,#1259);
#1123=LINE('',#34241,#1260);
#1124=LINE('',#34248,#1261);
#1125=LINE('',#34252,#1262);
#1126=LINE('',#34254,#1263);
#1127=LINE('',#34255,#1264);
#1128=LINE('',#34259,#1265);
#1129=LINE('',#34309,#1266);
#1130=LINE('',#34310,#1267);
#1131=LINE('',#34319,#1268);
#1132=LINE('',#34321,#1269);
#1133=LINE('',#34324,#1270);
#1134=LINE('',#34326,#1271);
#1135=LINE('',#34327,#1272);
#1136=LINE('',#34330,#1273);
#1137=LINE('',#34334,#1274);
#1138=LINE('',#34335,#1275);
#1139=LINE('',#34338,#1276);
#1140=LINE('',#34339,#1277);
#1141=LINE('',#34344,#1278);
#1142=LINE('',#34345,#1279);
#1143=LINE('',#34353,#1280);
#1144=LINE('',#34355,#1281);
#1145=LINE('',#34357,#1282);
#1146=LINE('',#34358,#1283);
#1147=LINE('',#34364,#1284);
#1148=LINE('',#34367,#1285);
#1149=LINE('',#34369,#1286);
#1150=LINE('',#34370,#1287);
#1151=VECTOR('',#5009,5.);
#1152=VECTOR('',#5012,5.);
#1153=VECTOR('',#5033,25.);
#1154=VECTOR('',#5044,28.);
#1155=VECTOR('',#5069,24.5);
#1156=VECTOR('',#5082,4.);
#1157=VECTOR('',#5089,10.);
#1158=VECTOR('',#5100,4.085);
#1159=VECTOR('',#5105,4.085);
#1160=VECTOR('',#5108,4.085);
#1161=VECTOR('',#5111,4.085);
#1162=VECTOR('',#5114,4.085);
#1163=VECTOR('',#5117,4.085);
#1164=VECTOR('',#5120,4.085);
#1165=VECTOR('',#5123,4.085);
#1166=VECTOR('',#5128,3.38975);
#1167=VECTOR('',#5133,3.38975);
#1168=VECTOR('',#5136,3.38975);
#1169=VECTOR('',#5139,3.38975);
#1170=VECTOR('',#5142,3.38975);
#1171=VECTOR('',#5145,3.38975);
#1172=VECTOR('',#5148,3.38975);
#1173=VECTOR('',#5153,3.38975);
#1174=VECTOR('',#5156,3.38975);
#1175=VECTOR('',#5169,8.);
#1176=VECTOR('',#5182,5.);
#1177=VECTOR('',#5189,3.22275);
#1178=VECTOR('',#5194,3.22275);
#1179=VECTOR('',#5197,3.22275);
#1180=VECTOR('',#5200,3.22275);
#1181=VECTOR('',#5203,3.22275);
#1182=VECTOR('',#5206,3.22275);
#1183=VECTOR('',#5217,10.);
#1184=VECTOR('',#5220,10.);
#1185=VECTOR('',#5223,10.);
#1186=VECTOR('',#5226,10.);
#1187=VECTOR('',#5227,10.);
#1188=VECTOR('',#5228,3.);
#1189=VECTOR('',#5231,10.);
#1190=VECTOR('',#5246,3.22275);
#1191=VECTOR('',#5251,3.22275);
#1192=VECTOR('',#5254,3.22275);
#1193=VECTOR('',#5257,3.22275);
#1194=VECTOR('',#5260,3.22275);
#1195=VECTOR('',#5263,3.22275);
#1196=VECTOR('',#5266,3.22275);
#1197=VECTOR('',#5269,3.22275);
#1198=VECTOR('',#5282,10.);
#1199=VECTOR('',#5285,10.);
#1200=VECTOR('',#5288,10.);
#1201=VECTOR('',#5291,10.);
#1202=VECTOR('',#5292,10.);
#1203=VECTOR('',#5293,3.);
#1204=VECTOR('',#5296,10.);
#1205=VECTOR('',#5311,4.085);
#1206=VECTOR('',#5316,4.085);
#1207=VECTOR('',#5319,4.085);
#1208=VECTOR('',#5322,4.085);
#1209=VECTOR('',#5325,4.085);
#1210=VECTOR('',#5328,4.085);
#1211=VECTOR('',#5331,4.085);
#1212=VECTOR('',#5334,4.085);
#1213=VECTOR('',#5337,4.085);
#1214=VECTOR('',#5358,5.);
#1215=VECTOR('',#5367,5.);
#1216=VECTOR('',#5370,10.);
#1217=VECTOR('',#5373,10.);
#1218=VECTOR('',#5376,10.);
#1219=VECTOR('',#5379,10.);
#1220=VECTOR('',#5384,10.);
#1221=VECTOR('',#5387,10.);
#1222=VECTOR('',#5390,10.);
#1223=VECTOR('',#5393,10.);
#1224=VECTOR('',#5648,10.);
#1225=VECTOR('',#5651,10.);
#1226=VECTOR('',#5654,10.);
#1227=VECTOR('',#5659,10.);
#1228=VECTOR('',#5664,10.);
#1229=VECTOR('',#5669,10.);
#1230=VECTOR('',#5674,10.);
#1231=VECTOR('',#5679,10.);
#1232=VECTOR('',#5684,10.);
#1233=VECTOR('',#5689,10.);
#1234=VECTOR('',#5694,10.);
#1235=VECTOR('',#5699,10.);
#1236=VECTOR('',#5704,10.);
#1237=VECTOR('',#5709,10.);
#1238=VECTOR('',#5714,10.);
#1239=VECTOR('',#5963,10.);
#1240=VECTOR('',#5968,10.);
#1241=VECTOR('',#5971,10.);
#1242=VECTOR('',#5974,10.);
#1243=VECTOR('',#5977,10.);
#1244=VECTOR('',#5980,10.);
#1245=VECTOR('',#5983,10.);
#1246=VECTOR('',#5986,10.);
#1247=VECTOR('',#5989,10.);
#1248=VECTOR('',#5992,10.);
#1249=VECTOR('',#5995,10.);
#1250=VECTOR('',#5998,10.);
#1251=VECTOR('',#6001,10.);
#1252=VECTOR('',#6032,28.);
#1253=VECTOR('',#6045,1.5);
#1254=VECTOR('',#6048,1.5);
#1255=VECTOR('',#6051,1.5);
#1256=VECTOR('',#6054,1.5);
#1257=VECTOR('',#6057,1.5);
#1258=VECTOR('',#6060,1.5);
#1259=VECTOR('',#6063,1.5);
#1260=VECTOR('',#6066,1.5);
#1261=VECTOR('',#6073,10.);
#1262=VECTOR('',#6076,10.);
#1263=VECTOR('',#6077,10.);
#1264=VECTOR('',#6078,10.);
#1265=VECTOR('',#6081,10.);
#1266=VECTOR('',#6092,10.);
#1267=VECTOR('',#6093,10.);
#1268=VECTOR('',#6106,10.);
#1269=VECTOR('',#6109,10.);
#1270=VECTOR('',#6112,10.);
#1271=VECTOR('',#6113,10.);
#1272=VECTOR('',#6114,10.);
#1273=VECTOR('',#6117,10.);
#1274=VECTOR('',#6122,10.);
#1275=VECTOR('',#6123,10.);
#1276=VECTOR('',#6126,10.);
#1277=VECTOR('',#6127,10.);
#1278=VECTOR('',#6134,10.);
#1279=VECTOR('',#6135,10.);
#1280=VECTOR('',#6146,10.);
#1281=VECTOR('',#6147,10.);
#1282=VECTOR('',#6148,10.);
#1283=VECTOR('',#6149,10.);
#1284=VECTOR('',#6156,10.);
#1285=VECTOR('',#6159,10.);
#1286=VECTOR('',#6160,10.);
#1287=VECTOR('',#6161,10.);
#1288=B_SPLINE_CURVE_WITH_KNOTS('',3,(#6193,#6194,#6195,#6196,#6197,#6198,
#6199,#6200,#6201,#6202,#6203,#6204,#6205,#6206,#6207,#6208,#6209,#6210),
 .UNSPECIFIED.,.F.,.F.,(4,2,2,2,2,2,2,2,4),(0.,0.188782577961406,0.377565155922812,
0.566341063168598,0.755116970414385,0.94389287766017,1.13266878490596,1.32145136286736,
1.51023394082877),.UNSPECIFIED.);
#1289=B_SPLINE_CURVE_WITH_KNOTS('',3,(#6211,#6212,#6213,#6214,#6215,#6216,
#6217,#6218,#6219,#6220,#6221,#6222,#6223,#6224,#6225,#6226,#6227,#6228),
 .UNSPECIFIED.,.F.,.F.,(4,2,2,2,2,2,2,2,4),(1.51023394082877,1.69901651879018,
1.88779909675158,2.07657500399737,2.26535091124315,2.45412681848894,2.64290272573473,
2.83168530369613,3.02046788165754),.UNSPECIFIED.);
#1290=B_SPLINE_CURVE_WITH_KNOTS('',3,(#6232,#6233,#6234,#6235,#6236,#6237,
#6238,#6239,#6240,#6241,#6242,#6243,#6244,#6245,#6246,#6247,#6248,#6249),
 .UNSPECIFIED.,.F.,.F.,(4,2,2,2,2,2,2,2,4),(-3.02227736861757,-2.83337974067247,
-2.64448211272738,-2.45559506959528,-2.26670802646318,-2.07782098333108,
-1.88893394019898,-1.70003631225388,-1.51113868430879),.UNSPECIFIED.);
#1291=B_SPLINE_CURVE_WITH_KNOTS('',3,(#6250,#6251,#6252,#6253,#6254,#6255,
#6256,#6257,#6258,#6259,#6260,#6261,#6262,#6263,#6264,#6265,#6266,#6267),
 .UNSPECIFIED.,.F.,.F.,(4,2,2,2,2,2,2,2,4),(-1.51113868430879,-1.32224105636369,
-1.13334342841859,-0.944456385286492,-0.755569342154393,-0.566682299022294,
-0.377795255890194,-0.188897627945097,0.),.UNSPECIFIED.);
#1292=B_SPLINE_CURVE_WITH_KNOTS('',3,(#6271,#6272,#6273,#6274,#6275,#6276,
#6277,#6278,#6279,#6280,#6281,#6282,#6283,#6284,#6285,#6286,#6287,#6288),
 .UNSPECIFIED.,.F.,.F.,(4,2,2,2,2,2,2,2,4),(-3.02227736861757,-2.83337974067247,
-2.64448211272738,-2.45559506959528,-2.26670802646318,-2.07782098333108,
-1.88893394019898,-1.70003631225388,-1.51113868430879),.UNSPECIFIED.);
#1293=B_SPLINE_CURVE_WITH_KNOTS('',3,(#6289,#6290,#6291,#6292,#6293,#6294,
#6295,#6296,#6297,#6298,#6299,#6300,#6301,#6302,#6303,#6304,#6305,#6306),
 .UNSPECIFIED.,.F.,.F.,(4,2,2,2,2,2,2,2,4),(-1.51113868430879,-1.32224105636369,
-1.13334342841859,-0.944456385286492,-0.755569342154393,-0.566682299022294,
-0.377795255890194,-0.188897627945097,0.),.UNSPECIFIED.);
#1294=B_SPLINE_CURVE_WITH_KNOTS('',3,(#6310,#6311,#6312,#6313,#6314,#6315,
#6316,#6317,#6318,#6319,#6320,#6321,#6322,#6323,#6324,#6325,#6326,#6327),
 .UNSPECIFIED.,.F.,.F.,(4,2,2,2,2,2,2,2,4),(0.,0.188782577961406,0.377565155922812,
0.566341063168599,0.755116970414385,0.943892877660171,1.13266878490596,
1.32145136286736,1.51023394082877),.UNSPECIFIED.);
#1295=B_SPLINE_CURVE_WITH_KNOTS('',3,(#6328,#6329,#6330,#6331,#6332,#6333,
#6334,#6335,#6336,#6337,#6338,#6339,#6340,#6341,#6342,#6343,#6344,#6345),
 .UNSPECIFIED.,.F.,.F.,(4,2,2,2,2,2,2,2,4),(1.51023394082877,1.69901651879018,
1.88779909675158,2.07657500399737,2.26535091124315,2.45412681848894,2.64290272573473,
2.83168530369613,3.02046788165754),.UNSPECIFIED.);
#1296=B_SPLINE_CURVE_WITH_KNOTS('',3,(#6414,#6415,#6416,#6417),
 .UNSPECIFIED.,.F.,.F.,(4,4),(66.9422038205255,67.9106018773349),
 .UNSPECIFIED.);
#1297=B_SPLINE_CURVE_WITH_KNOTS('',3,(#6420,#6421,#6422,#6423,#6424,#6425,
#6426,#6427,#6428,#6429,#6430,#6431,#6432,#6433,#6434,#6435,#6436,#6437,
#6438,#6439,#6440,#6441,#6442,#6443,#6444,#6445,#6446,#6447,#6448,#6449,
#6450,#6451,#6452,#6453,#6454,#6455,#6456,#6457,#6458,#6459,#6460,#6461,
#6462,#6463,#6464,#6465,#6466,#6467,#6468,#6469,#6470,#6471,#6472,#6473,
#6474),.UNSPECIFIED.,.F.,.F.,(4,3,3,3,3,3,3,3,3,3,3,3,3,3,3,3,3,3,4),(66.9424261296312,
67.0301287110664,67.11783680989,67.2055708646774,67.2933977991414,67.3812798406369,
67.4692836569234,67.4927659538656,67.5800588691701,67.6672436830704,67.7543439714456,
67.8413856927823,67.9283969745756,68.0153990026826,68.1024129513622,68.1895118069197,
68.276654508908,68.3639316760445,68.4345182397239),.UNSPECIFIED.);
#1298=B_SPLINE_CURVE_WITH_KNOTS('',3,(#6480,#6481,#6482,#6483,#6484,#6485,
#6486,#6487,#6488,#6489,#6490,#6491,#6492,#6493,#6494,#6495,#6496,#6497,
#6498,#6499,#6500,#6501,#6502,#6503,#6504,#6505,#6506,#6507,#6508,#6509,
#6510,#6511,#6512,#6513,#6514,#6515,#6516,#6517,#6518,#6519,#6520,#6521,
#6522,#6523,#6524,#6525,#6526,#6527,#6528,#6529,#6530,#6531,#6532,#6533,
#6534,#6535,#6536,#6537,#6538,#6539,#6540,#6541,#6542,#6543,#6544,#6545,
#6546,#6547,#6548,#6549,#6550,#6551,#6552,#6553,#6554,#6555,#6556,#6557,
#6558,#6559,#6560,#6561,#6562,#6563,#6564,#6565,#6566,#6567,#6568,#6569,
#6570,#6571,#6572,#6573,#6574,#6575,#6576,#6577,#6578,#6579,#6580,#6581,
#6582,#6583,#6584,#6585,#6586,#6587,#6588,#6589,#6590,#6591,#6592,#6593,
#6594,#6595,#6596,#6597,#6598,#6599,#6600,#6601,#6602,#6603,#6604,#6605,
#6606,#6607,#6608,#6609,#6610,#6611,#6612,#6613,#6614,#6615,#6616,#6617,
#6618,#6619,#6620,#6621,#6622,#6623,#6624,#6625,#6626,#6627,#6628,#6629,
#6630,#6631,#6632,#6633,#6634,#6635,#6636,#6637,#6638,#6639,#6640,#6641,
#6642,#6643,#6644,#6645,#6646,#6647,#6648,#6649,#6650,#6651,#6652,#6653,
#6654,#6655,#6656,#6657,#6658,#6659,#6660,#6661,#6662,#6663,#6664,#6665,
#6666,#6667,#6668,#6669,#6670,#6671,#6672,#6673,#6674,#6675),
 .UNSPECIFIED.,.F.,.F.,(4,3,3,3,3,3,3,3,3,3,3,3,3,3,3,3,3,3,3,3,3,3,3,3,
3,3,3,3,3,3,3,3,3,3,3,3,3,3,3,3,3,3,3,3,3,3,3,3,3,3,3,3,3,3,3,3,3,3,3,3,
3,3,3,3,3,4),(60.65863305798,60.7462805898925,60.8339724069765,60.9218056826776,
61.0052798001373,61.0931588658759,61.1809279562765,61.268609989713,61.3590030388232,
61.4465878063973,61.5341599134385,61.6217399433751,61.7093484801914,61.7970529682031,
61.8848150467633,61.9727002613834,61.9917543825941,62.0796342468088,62.1674043958499,
62.2550877431606,62.3454803958969,62.4330670954196,62.5206413585054,62.6082237650501,
62.6958348956645,62.783542281868,62.8713074397826,62.9591959709118,62.9782289650509,
63.0659959514938,63.1536528050209,63.2412225781541,63.3316576993233,63.4191308553117,
63.5065917826189,63.5940611841444,63.6815597638258,63.7691558290588,63.8568102574783,
63.944589744661,63.9647035475077,64.052716452029,64.1406191116994,64.2284342850664,
64.3187772656787,64.406493254731,64.4941956385468,64.581904856344,64.6742231747492,
64.7620556467768,64.8499453709517,64.9379542944654,64.9511781299645,65.039109056126,
65.1269316198708,65.2146686503736,65.3050416581296,65.3926847974272,65.4803164125707,
65.5679570124934,65.6556271074234,65.743394281365,65.8312197741986,65.9191689688196,
65.9376527124213,65.9734457253856),.UNSPECIFIED.);
#1299=B_SPLINE_CURVE_WITH_KNOTS('',3,(#6676,#6677,#6678,#6679,#6680),
 .UNSPECIFIED.,.F.,.F.,(4,1,4),(65.9734517999329,66.9241272948781,66.9422038205255),
 .UNSPECIFIED.);
#1300=B_SPLINE_CURVE_WITH_KNOTS('',3,(#6682,#6683,#6684,#6685,#6686,#6687,
#6688,#6689,#6690,#6691,#6692,#6693,#6694,#6695,#6696,#6697,#6698,#6699,
#6700,#6701,#6702,#6703,#6704,#6705,#6706,#6707,#6708,#6709,#6710,#6711,
#6712,#6713,#6714,#6715),.UNSPECIFIED.,.F.,.F.,(4,3,3,3,3,3,3,3,3,3,3,4),
(65.9734457253856,66.0635791722207,66.1537859784836,66.2441584095279,66.3346160682269,
66.4252650574005,66.5062913714088,66.5943110699188,66.6821978307666,66.7700074190229,
66.8577576382145,66.9424261296312),.UNSPECIFIED.);
#1301=B_SPLINE_CURVE_WITH_KNOTS('',3,(#6716,#6717,#6718,#6719,#6720,#6721,
#6722,#6723,#6724,#6725,#6726,#6727,#6728,#6729,#6730,#6731,#6732,#6733,
#6734,#6735,#6736,#6737,#6738,#6739,#6740,#6741,#6742,#6743,#6744,#6745,
#6746,#6747,#6748,#6749,#6750,#6751,#6752,#6753,#6754,#6755,#6756,#6757,
#6758,#6759,#6760,#6761,#6762,#6763,#6764,#6765,#6766,#6767,#6768,#6769,
#6770,#6771,#6772,#6773,#6774,#6775,#6776,#6777,#6778,#6779,#6780,#6781,
#6782,#6783,#6784,#6785,#6786,#6787,#6788,#6789,#6790,#6791,#6792,#6793,
#6794,#6795,#6796,#6797,#6798,#6799,#6800,#6801,#6802,#6803,#6804,#6805,
#6806,#6807,#6808,#6809,#6810,#6811,#6812,#6813,#6814,#6815,#6816,#6817,
#6818,#6819,#6820,#6821,#6822,#6823,#6824,#6825,#6826,#6827,#6828,#6829,
#6830,#6831,#6832,#6833,#6834,#6835,#6836,#6837,#6838,#6839,#6840,#6841,
#6842,#6843,#6844,#6845,#6846,#6847,#6848,#6849,#6850,#6851,#6852,#6853,
#6854,#6855,#6856,#6857,#6858,#6859,#6860,#6861,#6862,#6863,#6864,#6865,
#6866,#6867,#6868,#6869,#6870,#6871,#6872,#6873,#6874,#6875,#6876,#6877,
#6878,#6879,#6880,#6881,#6882,#6883,#6884,#6885,#6886,#6887,#6888,#6889,
#6890,#6891,#6892,#6893,#6894,#6895,#6896,#6897,#6898,#6899,#6900,#6901,
#6902,#6903,#6904,#6905,#6906,#6907,#6908),.UNSPECIFIED.,.F.,.F.,(4,3,3,
3,3,3,3,3,3,3,3,3,3,3,3,3,3,3,3,3,3,3,3,3,3,3,3,3,3,3,3,3,3,3,3,3,3,3,3,
3,3,3,3,3,3,3,3,3,3,3,3,3,3,3,3,3,3,3,3,3,3,3,3,3,4),(60.6593693718721,
60.7471428095145,60.8348250979655,60.922439102879,61.0100156253259,61.0975752044484,
61.1851384398607,61.2727259287143,61.3604075726339,61.4481429995207,61.5360068051033,
61.5739184591248,61.6617852019871,61.7495420513973,61.8372119392129,61.927609577009,
62.015182510545,62.1027429191062,62.1903113984739,62.2779085450996,62.3656019348734,
62.4533530734372,62.541227657696,62.5603930415816,62.6482441716657,62.7359853638815,
62.8236395693427,62.9140430761797,63.001600365264,63.0891451707661,63.1766981055555,
63.2642797832255,63.3519578926021,63.439693843782,63.5275534886173,63.5468676240384,
63.634746673192,63.722515747168,63.810197764357,63.9005908196243,63.9881755714853,
64.0757476630367,64.1633276777229,64.2509361995434,64.3386406730057,64.4264027372613,
64.5142879380342,64.5333422064952,64.621221995123,64.7089920681593,64.7966753391438,
64.8870680203698,64.9746546432615,65.0622288297388,65.1498111597819,65.2374222140876,
65.3251295246472,65.4128946072222,65.5007830640145,65.519816788952,65.6138059465638,
65.707511444738,65.8010451097038,65.8943210633096,65.9734457251906),
 .UNSPECIFIED.);
#1302=B_SPLINE_CURVE_WITH_KNOTS('',3,(#6914,#6915,#6916,#6917,#6918,#6919,
#6920,#6921,#6922,#6923,#6924,#6925,#6926,#6927,#6928,#6929,#6930,#6931,
#6932,#6933,#6934,#6935,#6936,#6937,#6938,#6939,#6940,#6941,#6942,#6943,
#6944,#6945,#6946,#6947,#6948,#6949,#6950,#6951,#6952,#6953,#6954,#6955,
#6956,#6957,#6958,#6959,#6960,#6961,#6962,#6963,#6964,#6965,#6966,#6967,
#6968,#6969,#6970,#6971,#6972,#6973,#6974,#6975,#6976,#6977,#6978,#6979,
#6980,#6981,#6982,#6983,#6984,#6985,#6986,#6987,#6988,#6989,#6990,#6991,
#6992,#6993,#6994,#6995,#6996,#6997,#6998,#6999,#7000,#7001,#7002,#7003,
#7004,#7005,#7006,#7007,#7008,#7009,#7010,#7011,#7012,#7013,#7014,#7015,
#7016,#7017,#7018,#7019,#7020,#7021,#7022,#7023,#7024,#7025,#7026,#7027,
#7028,#7029,#7030,#7031,#7032,#7033,#7034,#7035,#7036,#7037,#7038,#7039,
#7040,#7041,#7042,#7043,#7044,#7045,#7046,#7047,#7048,#7049,#7050,#7051,
#7052,#7053,#7054,#7055,#7056,#7057,#7058,#7059,#7060,#7061,#7062,#7063,
#7064,#7065,#7066,#7067,#7068,#7069,#7070,#7071,#7072,#7073,#7074,#7075,
#7076,#7077,#7078,#7079,#7080,#7081,#7082,#7083,#7084,#7085,#7086,#7087,
#7088,#7089,#7090,#7091,#7092,#7093,#7094,#7095,#7096,#7097,#7098,#7099,
#7100,#7101,#7102,#7103,#7104,#7105,#7106),.UNSPECIFIED.,.F.,.F.,(4,3,3,
3,3,3,3,3,3,3,3,3,3,3,3,3,3,3,3,3,3,3,3,3,3,3,3,3,3,3,3,3,3,3,3,3,3,3,3,
3,3,3,3,3,3,3,3,3,3,3,3,3,3,3,3,3,3,3,3,3,3,3,3,3,4),(54.3763646710769,
54.4651231253668,54.5526899009801,54.6402468478357,54.7278145647135,54.8174689998842,
54.9051667757655,54.9957995405809,55.0864323053964,55.1742960896468,55.2620499541187,
55.3497168345997,55.4401155912564,55.5276854816214,55.615242839173,55.7028082631215,
55.7904023533463,55.8780927007007,55.9658408016046,56.0537123778884,56.0729068878532,
56.1607710647536,56.2485253261876,56.3361926074087,56.4265912152714,56.5141615131015,
56.6017192798774,56.689285114346,56.7768796159245,56.864570373776,56.952318885137,
57.0401908687341,57.05938147031,57.1472435605767,57.2349957310401,57.3226609195071,
57.4130603111646,57.5006285251765,57.5881842150842,57.6757479819056,57.7633404273363,
57.851029156223,57.9387756522291,58.02664565519,58.0458560527669,58.1337211732737,
58.2214763663591,58.3091445663341,58.3995428249453,58.4871140040178,58.5746726366804,
58.6622393207953,58.7498346548823,58.8375262159865,58.9252755144032,59.0131482558552,
59.0323306352237,59.1201349616358,59.2078320873874,59.2954427965408,59.3829878029622,
59.4704935028068,59.5579758209044,59.6454743488502,59.6902604182061),
 .UNSPECIFIED.);
#1303=B_SPLINE_CURVE_WITH_KNOTS('',3,(#7107,#7108,#7109,#7110,#7111,#7112,
#7113,#7114,#7115,#7116,#7117,#7118,#7119,#7120,#7121,#7122,#7123,#7124,
#7125,#7126,#7127,#7128,#7129,#7130,#7131,#7132,#7133,#7134,#7135,#7136,
#7137,#7138,#7139,#7140,#7141,#7142,#7143),.UNSPECIFIED.,.F.,.F.,(4,3,3,
3,3,3,3,3,3,3,3,3,4),(59.6902604184005,59.7919143931213,59.8941560797584,
59.9970488126565,60.0188052176805,60.1066415554168,60.194374903753,60.2820260480705,
60.3696157068656,60.4571706432182,60.544705998586,60.632257830546,60.65863305798),
 .UNSPECIFIED.);
#1304=B_SPLINE_CURVE_WITH_KNOTS('',3,(#7145,#7146,#7147,#7148,#7149,#7150,
#7151,#7152,#7153,#7154,#7155,#7156,#7157,#7158,#7159,#7160,#7161,#7162,
#7163,#7164,#7165,#7166,#7167,#7168,#7169,#7170,#7171,#7172,#7173,#7174,
#7175,#7176,#7177,#7178,#7179,#7180,#7181),.UNSPECIFIED.,.F.,.F.,(4,3,3,
3,3,3,3,3,3,3,3,3,4),(59.69026041841,59.7770684744581,59.8637759910736,
59.9542344767729,60.0408167469363,60.1273775252551,60.2139383758267,60.3005208587838,
60.3871935732878,60.4739195335137,60.5607688817594,60.587443876668,60.6593693718721),
 .UNSPECIFIED.);
#1305=B_SPLINE_CURVE_WITH_KNOTS('',3,(#7182,#7183,#7184,#7185,#7186,#7187,
#7188,#7189,#7190,#7191,#7192,#7193,#7194,#7195,#7196,#7197,#7198,#7199,
#7200,#7201,#7202,#7203,#7204,#7205,#7206,#7207,#7208,#7209,#7210,#7211,
#7212,#7213,#7214,#7215,#7216,#7217,#7218,#7219,#7220,#7221,#7222,#7223,
#7224,#7225,#7226,#7227,#7228,#7229,#7230,#7231,#7232,#7233,#7234,#7235,
#7236,#7237,#7238,#7239,#7240,#7241,#7242,#7243,#7244,#7245,#7246,#7247,
#7248,#7249,#7250,#7251,#7252,#7253,#7254,#7255,#7256,#7257,#7258,#7259,
#7260,#7261,#7262,#7263,#7264,#7265,#7266,#7267,#7268,#7269,#7270,#7271,
#7272,#7273,#7274,#7275,#7276,#7277,#7278,#7279,#7280,#7281,#7282,#7283,
#7284,#7285,#7286,#7287,#7288,#7289,#7290,#7291,#7292,#7293,#7294,#7295,
#7296,#7297,#7298,#7299,#7300,#7301,#7302,#7303,#7304,#7305,#7306,#7307,
#7308,#7309,#7310,#7311,#7312,#7313,#7314,#7315,#7316,#7317,#7318,#7319,
#7320,#7321,#7322,#7323,#7324,#7325,#7326,#7327,#7328,#7329,#7330,#7331,
#7332,#7333,#7334,#7335,#7336,#7337,#7338,#7339,#7340,#7341,#7342,#7343,
#7344,#7345,#7346,#7347,#7348,#7349,#7350,#7351,#7352,#7353,#7354,#7355,
#7356,#7357,#7358,#7359,#7360,#7361,#7362,#7363,#7364,#7365,#7366,#7367,
#7368,#7369,#7370,#7371,#7372,#7373,#7374,#7375,#7376,#7377),
 .UNSPECIFIED.,.F.,.F.,(4,3,3,3,3,3,3,3,3,3,3,3,3,3,3,3,3,3,3,3,3,3,3,3,
3,3,3,3,3,3,3,3,3,3,3,3,3,3,3,3,3,3,3,3,3,3,3,3,3,3,3,3,3,3,3,3,3,3,3,3,
3,3,3,3,3,4),(54.3753548645582,54.4630392923091,54.5507792046392,54.6386454074467,
54.6685963819271,54.7564600562574,54.8442138119439,54.9318805848875,55.0222793823246,
55.1098491689013,55.1974064242269,55.2849717476172,55.3725657390588,55.4602559907231,
55.5480039976374,55.6358754830825,55.6550709643839,55.7429347095602,55.8306885366184,
55.9183553813669,56.0087541520512,56.0963240110393,56.1838813388722,56.2714467347849,
56.3590407986829,56.4467311223415,56.5344792010609,56.6223507574992,56.6415455468407,
56.7294090248321,56.8171625843396,56.9048291614957,56.995228032471,57.0827976254673,
57.170354688365,57.257919820688,57.3455136226315,57.433203688048,57.5209515104051,
57.6088228151113,57.6280201292976,57.7158839134109,57.8036377777518,57.8913046581076,
57.9817034148135,58.069273305069,58.1568306625171,58.2443960863681,58.3319901765016,
58.4196805237739,58.5074286246011,58.5953002008165,58.6144947117544,58.7023588861019,
58.7901131449712,58.8777804236191,58.9681790324431,59.0557493276956,59.1433070918966,
59.2308729237961,59.3184674228137,59.4061581781297,59.4939066869673,59.5817786680768,
59.6009692942112,59.6902604182061),.UNSPECIFIED.);
#1306=B_SPLINE_CURVE_WITH_KNOTS('',3,(#7383,#7384,#7385,#7386,#7387,#7388,
#7389,#7390,#7391,#7392,#7393,#7394,#7395,#7396,#7397,#7398,#7399,#7400,
#7401,#7402,#7403,#7404,#7405,#7406,#7407,#7408,#7409,#7410,#7411,#7412,
#7413,#7414,#7415,#7416,#7417,#7418,#7419,#7420,#7421,#7422,#7423,#7424,
#7425,#7426,#7427,#7428,#7429,#7430,#7431,#7432,#7433,#7434,#7435,#7436,
#7437,#7438,#7439,#7440,#7441,#7442,#7443,#7444,#7445,#7446,#7447,#7448,
#7449,#7450,#7451,#7452,#7453,#7454,#7455,#7456,#7457,#7458,#7459,#7460,
#7461,#7462,#7463,#7464,#7465,#7466,#7467,#7468,#7469,#7470,#7471,#7472,
#7473,#7474,#7475,#7476,#7477,#7478,#7479,#7480,#7481,#7482,#7483,#7484,
#7485,#7486,#7487,#7488,#7489,#7490,#7491,#7492,#7493,#7494,#7495,#7496,
#7497,#7498,#7499,#7500,#7501,#7502,#7503,#7504,#7505,#7506,#7507,#7508,
#7509,#7510,#7511,#7512,#7513,#7514,#7515,#7516,#7517,#7518,#7519,#7520,
#7521,#7522,#7523,#7524,#7525,#7526,#7527,#7528,#7529,#7530,#7531,#7532,
#7533,#7534,#7535,#7536,#7537,#7538,#7539,#7540,#7541,#7542,#7543,#7544,
#7545,#7546,#7547,#7548,#7549,#7550,#7551,#7552,#7553,#7554,#7555,#7556,
#7557,#7558,#7559,#7560,#7561,#7562,#7563,#7564,#7565,#7566,#7567,#7568,
#7569,#7570,#7571,#7572,#7573,#7574,#7575),.UNSPECIFIED.,.F.,.F.,(4,3,3,
3,3,3,3,3,3,3,3,3,3,3,3,3,3,3,3,3,3,3,3,3,3,3,3,3,3,3,3,3,3,3,3,3,3,3,3,
3,3,3,3,3,3,3,3,3,3,3,3,3,3,3,3,3,3,3,3,3,3,3,3,3,4),(48.0922715957158,
48.1811102281988,48.2689738944005,48.356727642146,48.4443944073429,48.534793207757,
48.6223629871136,48.7099202354255,48.7974855520155,48.8850795368768,48.9727697823158,
49.0605177832053,49.1483892629593,49.1675848106556,49.255448478926,49.3432022287112,
49.430868995917,49.5212677955664,49.6088375768429,49.6963948270385,49.7839601454743,
49.8715541321415,49.9592443793189,50.0469923819093,50.1348638632974,50.1540593931124,
50.2419230728153,50.3296768340956,50.4173436128442,50.5077424081848,50.5953122010484,
50.682869462827,50.7704347928287,50.8580287910321,50.9457190496439,51.0334670636219,
51.1213385562451,51.1405339755692,51.2283976218724,51.3161513497307,51.4038180950754,
51.4942169029442,51.5817866626605,51.6693438914446,51.7569091886402,51.8445031542623,
51.9321933807854,52.0199413629268,52.1078128243148,52.127008558026,52.2148722323394,
52.3026259880082,52.3902927609331,52.4806915583768,52.5682613449324,52.6558186002362,
52.743383923604,52.8309779150221,52.9186681666621,53.0064161735513,53.0942876589708,
53.1134831404828,53.2201894401228,53.325638450398,53.4070751108784),
 .UNSPECIFIED.);
#1307=B_SPLINE_CURVE_WITH_KNOTS('',3,(#7576,#7577,#7578,#7579,#7580,#7581,
#7582,#7583,#7584,#7585,#7586,#7587,#7588,#7589,#7590,#7591,#7592,#7593,
#7594,#7595,#7596,#7597,#7598,#7599,#7600,#7601,#7602,#7603,#7604,#7605,
#7606,#7607,#7608,#7609,#7610,#7611,#7612),.UNSPECIFIED.,.F.,.F.,(4,3,3,
3,3,3,3,3,3,3,3,3,4),(53.4070751110265,53.4941360616469,53.5811674224662,
53.668190330731,53.7552259127633,53.8423504842459,53.9295193536601,54.0168313543366,
54.0999577229396,54.18781472203,54.2755749632124,54.3632416699008,54.3763646710769),
 .UNSPECIFIED.);
#1308=B_SPLINE_CURVE_WITH_KNOTS('',3,(#7614,#7615,#7616,#7617,#7618,#7619,
#7620,#7621,#7622,#7623,#7624,#7625,#7626,#7627,#7628,#7629,#7630,#7631,
#7632,#7633,#7634,#7635,#7636,#7637,#7638,#7639,#7640,#7641,#7642,#7643,
#7644,#7645,#7646,#7647),.UNSPECIFIED.,.F.,.F.,(4,3,3,3,3,3,3,3,3,3,3,4),
(53.4070751112481,53.514566858387,53.6236544087936,53.6821217994703,53.7699662995981,
53.8577089201619,53.9453704283004,54.0329715255116,54.1205451319431,54.2080995546255,
54.2956889402079,54.3753548645582),.UNSPECIFIED.);
#1309=B_SPLINE_CURVE_WITH_KNOTS('',3,(#7648,#7649,#7650,#7651,#7652,#7653,
#7654,#7655,#7656,#7657,#7658,#7659,#7660,#7661,#7662,#7663,#7664,#7665,
#7666,#7667,#7668,#7669,#7670,#7671,#7672,#7673,#7674,#7675,#7676,#7677,
#7678,#7679,#7680,#7681,#7682,#7683,#7684,#7685,#7686,#7687,#7688,#7689,
#7690,#7691,#7692,#7693,#7694,#7695,#7696,#7697,#7698,#7699,#7700,#7701,
#7702,#7703,#7704,#7705,#7706,#7707,#7708,#7709,#7710,#7711,#7712,#7713,
#7714,#7715,#7716,#7717,#7718,#7719,#7720,#7721,#7722,#7723,#7724,#7725,
#7726,#7727,#7728,#7729,#7730,#7731,#7732,#7733,#7734,#7735,#7736,#7737,
#7738,#7739,#7740,#7741,#7742,#7743,#7744,#7745,#7746,#7747,#7748,#7749,
#7750,#7751,#7752,#7753,#7754,#7755,#7756,#7757,#7758,#7759,#7760,#7761,
#7762,#7763,#7764,#7765,#7766,#7767,#7768,#7769,#7770,#7771,#7772,#7773,
#7774,#7775,#7776,#7777,#7778,#7779,#7780,#7781,#7782,#7783,#7784,#7785,
#7786,#7787,#7788,#7789,#7790,#7791,#7792,#7793,#7794,#7795,#7796,#7797,
#7798,#7799,#7800,#7801,#7802,#7803,#7804,#7805,#7806,#7807,#7808,#7809,
#7810,#7811,#7812,#7813,#7814,#7815,#7816,#7817,#7818,#7819,#7820,#7821,
#7822,#7823,#7824,#7825,#7826,#7827,#7828,#7829,#7830,#7831,#7832,#7833,
#7834,#7835,#7836,#7837,#7838,#7839,#7840,#7841,#7842,#7843),
 .UNSPECIFIED.,.F.,.F.,(4,3,3,3,3,3,3,3,3,3,3,3,3,3,3,3,3,3,3,3,3,3,3,3,
3,3,3,3,3,3,3,3,3,3,3,3,3,3,3,3,3,3,3,3,3,3,3,3,3,3,3,3,3,3,3,3,3,3,3,3,
3,3,3,3,3,4),(48.0930924415186,48.1806692098407,48.2682278326461,48.3557889116037,
48.4433730450696,48.5310507770843,48.6187812155429,48.7066414710093,48.7497488871863,
48.8376125557049,48.92536630576,49.0130330732565,49.1034318728048,49.1910016544217,
49.2785589049755,49.3661242237864,49.4537182108454,49.5414084584371,49.6291564614553,
49.7170279432874,49.7362234696431,49.8240871398504,49.9118408916014,49.9995076607984,
50.0899064597111,50.1774762430298,50.2650334952829,50.3525988157889,50.4401928045367,
50.5278830537994,50.6156310584803,50.7035025419507,50.7226980520999,50.8105617183162,
50.8983154660761,50.9859822312877,51.0763810316963,51.1639508110672,51.2515080593933,
51.3390733759977,51.4266673608728,51.5143576063255,51.6021056072286,51.6899770869957,
51.7091726345567,51.7970363028357,51.88479005263,51.9724568198442,52.0628556194904,
52.1504254007761,52.2379826509813,52.3255479694264,52.4131419561032,52.5008322032902,
52.5885802058899,52.6764516872875,52.6956472170135,52.7845757037651,52.8715739991427,
52.9584927489579,53.0453533763273,53.1357838100021,53.222609258072,53.3094383650151,
53.3963131402274,53.4070751110265),.UNSPECIFIED.);
#1310=B_SPLINE_CURVE_WITH_KNOTS('',3,(#7849,#7850,#7851,#7852,#7853,#7854,
#7855,#7856,#7857,#7858,#7859,#7860,#7861,#7862,#7863,#7864,#7865,#7866,
#7867,#7868,#7869,#7870,#7871,#7872,#7873,#7874,#7875,#7876,#7877,#7878,
#7879,#7880,#7881,#7882,#7883,#7884,#7885,#7886,#7887,#7888,#7889,#7890,
#7891,#7892,#7893,#7894,#7895,#7896,#7897,#7898,#7899,#7900,#7901,#7902,
#7903,#7904,#7905,#7906,#7907,#7908,#7909,#7910,#7911,#7912,#7913,#7914,
#7915,#7916,#7917,#7918,#7919,#7920,#7921,#7922,#7923,#7924,#7925,#7926,
#7927,#7928,#7929,#7930,#7931,#7932,#7933,#7934,#7935,#7936,#7937,#7938,
#7939,#7940,#7941,#7942,#7943,#7944,#7945,#7946,#7947,#7948,#7949,#7950,
#7951,#7952,#7953,#7954,#7955,#7956,#7957,#7958,#7959,#7960,#7961,#7962,
#7963,#7964,#7965,#7966,#7967,#7968,#7969,#7970,#7971,#7972,#7973,#7974,
#7975,#7976,#7977,#7978,#7979,#7980,#7981,#7982,#7983,#7984,#7985,#7986,
#7987,#7988,#7989,#7990,#7991,#7992,#7993,#7994,#7995,#7996,#7997,#7998,
#7999,#8000,#8001,#8002,#8003,#8004,#8005,#8006,#8007,#8008,#8009,#8010,
#8011,#8012,#8013,#8014,#8015,#8016,#8017,#8018,#8019,#8020,#8021,#8022,
#8023,#8024,#8025,#8026,#8027,#8028,#8029,#8030,#8031,#8032,#8033,#8034,
#8035,#8036,#8037,#8038,#8039,#8040,#8041,#8042,#8043,#8044),
 .UNSPECIFIED.,.F.,.F.,(4,3,3,3,3,3,3,3,3,3,3,3,3,3,3,3,3,3,3,3,3,3,3,3,
3,3,3,3,3,3,3,3,3,3,3,3,3,3,3,3,3,3,3,3,3,3,3,3,3,3,3,3,3,3,3,3,3,3,3,3,
3,3,3,3,3,4),(41.8093593517908,41.896925700064,41.9882599584125,42.0759549956636,
42.1637095871173,42.2515854767932,42.2622627334579,42.35012640214,42.4378801523619,
42.5255469200282,42.615945719514,42.7035155013069,42.7910727520387,42.8786380710294,
42.96623205827,43.0539223060446,43.1416703092467,43.229541791263,43.2487373159147,
43.3366009845863,43.4243547347969,43.5120215024516,43.6024203019415,43.6899900837217,
43.7775473344403,43.8651126534175,43.9527066406441,44.0403968884042,44.1281448915917,
44.216016373593,44.2352118983715,44.3230755672879,44.4108293177442,44.4984960856451,
44.588894885043,44.6764646670691,44.7640219180332,44.8515872372552,44.9391812247254,
45.0268714727266,45.1146194761536,45.2024909583908,45.2216864808283,45.3095501492757,
45.3973038992634,45.4849706666966,45.5753694662701,45.6629392478338,45.7504964983383,
45.8380618171039,45.9256558041216,46.0133460516777,46.1010940546639,46.1889655364693,
46.2081610632851,46.2951590562398,46.3820476809983,46.4688508233759,46.5555938060835,
46.6423059132212,46.7290085973227,46.8157232991051,46.9025184488413,46.9893581812461,
47.076320341889,47.1238898036606),.UNSPECIFIED.);
#1311=B_SPLINE_CURVE_WITH_KNOTS('',3,(#8045,#8046,#8047,#8048,#8049,#8050,
#8051,#8052,#8053,#8054,#8055,#8056,#8057,#8058,#8059,#8060,#8061,#8062,
#8063,#8064,#8065,#8066,#8067,#8068,#8069,#8070,#8071,#8072,#8073,#8074,
#8075,#8076,#8077,#8078,#8079,#8080,#8081),.UNSPECIFIED.,.F.,.F.,(4,3,3,
3,3,3,3,3,3,3,3,3,4),(47.1238898038469,47.1946356457419,47.2825045734518,
47.3702623111564,47.4605134717263,47.5481137855468,47.6356791061043,47.7232300467962,
47.8107872053906,47.8984076190842,47.9860664921885,48.0738212559678,48.0922715957158),
 .UNSPECIFIED.);
#1312=B_SPLINE_CURVE_WITH_KNOTS('',3,(#8083,#8084,#8085,#8086,#8087,#8088,
#8089,#8090,#8091,#8092,#8093,#8094,#8095,#8096,#8097,#8098,#8099,#8100,
#8101,#8102,#8103,#8104,#8105,#8106,#8107,#8108,#8109,#8110,#8111,#8112,
#8113,#8114,#8115,#8116,#8117,#8118,#8119),.UNSPECIFIED.,.F.,.F.,(4,3,3,
3,3,3,3,3,3,3,3,3,4),(47.1238898038469,47.2116835861261,47.2994728509267,
47.3872777931941,47.4751186140045,47.5630664520304,47.6510775151526,47.7392218004681,
47.7632743047295,47.8511215254599,47.9388724351879,48.026531246103,48.0930924415186),
 .UNSPECIFIED.);
#1313=B_SPLINE_CURVE_WITH_KNOTS('',3,(#8120,#8121,#8122,#8123,#8124,#8125,
#8126,#8127,#8128,#8129,#8130,#8131,#8132,#8133,#8134,#8135,#8136,#8137,
#8138,#8139,#8140,#8141,#8142,#8143,#8144,#8145,#8146,#8147,#8148,#8149,
#8150,#8151,#8152,#8153,#8154,#8155,#8156,#8157,#8158,#8159,#8160,#8161,
#8162,#8163,#8164,#8165,#8166,#8167,#8168,#8169,#8170,#8171,#8172,#8173,
#8174,#8175,#8176,#8177,#8178,#8179,#8180,#8181,#8182,#8183,#8184,#8185,
#8186,#8187,#8188,#8189,#8190,#8191,#8192,#8193,#8194,#8195,#8196,#8197,
#8198,#8199,#8200,#8201,#8202,#8203,#8204,#8205,#8206,#8207,#8208,#8209,
#8210,#8211,#8212,#8213,#8214,#8215,#8216,#8217,#8218,#8219,#8220,#8221,
#8222,#8223,#8224,#8225,#8226,#8227,#8228,#8229,#8230,#8231,#8232,#8233,
#8234,#8235,#8236,#8237,#8238,#8239,#8240,#8241,#8242,#8243,#8244,#8245,
#8246,#8247,#8248,#8249,#8250,#8251,#8252,#8253,#8254,#8255,#8256,#8257,
#8258,#8259,#8260,#8261,#8262,#8263,#8264,#8265,#8266,#8267,#8268,#8269,
#8270,#8271,#8272,#8273,#8274,#8275,#8276,#8277,#8278,#8279,#8280,#8281,
#8282,#8283,#8284,#8285,#8286,#8287,#8288,#8289,#8290,#8291,#8292,#8293,
#8294,#8295,#8296,#8297,#8298,#8299,#8300,#8301,#8302,#8303,#8304,#8305,
#8306,#8307,#8308,#8309,#8310,#8311,#8312,#8313,#8314,#8315),
 .UNSPECIFIED.,.F.,.F.,(4,3,3,3,3,3,3,3,3,3,3,3,3,3,3,3,3,3,3,3,3,3,3,3,
3,3,3,3,3,3,3,3,3,3,3,3,3,3,3,3,3,3,3,3,3,3,3,3,3,3,3,3,3,3,3,3,3,3,3,3,
3,3,3,3,3,4),(41.8092918158648,41.8444268099886,41.9322904786594,42.0200442288696,
42.107710996524,42.1981097960142,42.2856795777946,42.3732368285137,42.4608021474917,
42.5483961347192,42.6360863824806,42.7238343856694,42.8117058676723,42.8309013924454,
42.918765061131,43.0065188113555,43.094185579024,43.1845843785088,43.2721541603024,
43.3597114110342,43.4472767300246,43.5348707172641,43.6225609650369,43.7103089682367,
43.7981804502501,43.8173759749022,43.9052396436662,43.9929933939702,44.0806601617188,
44.1710589611738,44.258628743049,44.3461859938629,44.4337513129356,44.5213453002577,
44.6090355481129,44.6967835513953,44.7846550334906,44.803850557359,44.8917142260414,
44.9794679762634,45.0671347439299,45.1575335434156,45.2451033252088,45.3326605759407,
45.4202258949318,45.5078198821724,45.5955101299472,45.6832581331496,45.7711296151661,
45.7903251398158,45.8781888084878,45.9659425586989,46.0536093263539,46.1440081258437,
46.2315779076243,46.3191351583433,46.406700477321,46.494294464548,46.5819847123087,
46.6697327154966,46.7576041974983,46.7767997222726,46.8778180388024,46.9784525393735,
47.0783877221767,47.1238898036409),.UNSPECIFIED.);
#1314=B_SPLINE_CURVE_WITH_KNOTS('',3,(#8321,#8322,#8323,#8324,#8325,#8326,
#8327,#8328,#8329,#8330,#8331,#8332,#8333,#8334,#8335,#8336,#8337,#8338,
#8339,#8340,#8341,#8342,#8343,#8344,#8345,#8346,#8347,#8348,#8349,#8350,
#8351,#8352,#8353,#8354,#8355,#8356,#8357,#8358,#8359,#8360,#8361,#8362,
#8363,#8364,#8365,#8366,#8367,#8368,#8369,#8370,#8371,#8372,#8373,#8374,
#8375,#8376,#8377,#8378,#8379,#8380,#8381,#8382,#8383,#8384,#8385,#8386,
#8387,#8388,#8389,#8390,#8391,#8392,#8393,#8394,#8395,#8396,#8397,#8398,
#8399,#8400,#8401,#8402,#8403,#8404,#8405,#8406,#8407,#8408,#8409,#8410,
#8411,#8412,#8413,#8414,#8415,#8416,#8417,#8418,#8419,#8420,#8421,#8422,
#8423,#8424,#8425,#8426,#8427,#8428,#8429,#8430,#8431,#8432,#8433,#8434,
#8435,#8436,#8437,#8438,#8439,#8440,#8441,#8442,#8443,#8444,#8445,#8446,
#8447,#8448,#8449,#8450,#8451,#8452,#8453,#8454,#8455,#8456,#8457,#8458,
#8459,#8460,#8461,#8462,#8463,#8464,#8465,#8466,#8467,#8468,#8469,#8470,
#8471,#8472,#8473,#8474,#8475,#8476,#8477,#8478,#8479,#8480,#8481,#8482,
#8483,#8484,#8485,#8486,#8487,#8488,#8489,#8490,#8491,#8492,#8493,#8494,
#8495,#8496,#8497,#8498,#8499,#8500,#8501,#8502,#8503,#8504,#8505,#8506,
#8507,#8508,#8509,#8510,#8511,#8512,#8513),.UNSPECIFIED.,.F.,.F.,(4,3,3,
3,3,3,3,3,3,3,3,3,3,3,3,3,3,3,3,3,3,3,3,3,3,3,3,3,3,3,3,3,3,3,3,3,3,3,3,
3,3,3,3,3,3,3,3,3,3,3,3,3,3,3,3,3,3,3,3,3,3,3,3,3,4),(35.5268366911762,
35.6145084367687,35.7056217870122,35.7931929079879,35.8807503212151,35.9683146264148,
36.0559064231432,36.1435939353638,36.2313381445587,36.3192071347035,36.343415238717,
36.431278907217,36.5190326572565,36.6066994247405,36.6970982242947,36.784668005907,
36.872225256459,36.9597905752715,37.0473845623344,37.1350748099347,37.2228228129641,
37.3106942948111,37.3298898211739,37.4177534896489,37.505507239659,37.5931740071094,
37.6835728066745,37.7711425882421,37.8586998387456,37.946265157505,38.0338591445114,
38.1215493920497,38.2092973950135,38.2971688767908,38.3163644036307,38.4042280725361,
38.4919818229839,38.5796485908782,38.6700473902794,38.7576171723039,38.8451744232686,
38.9327397424928,39.0203337299674,39.1080239779757,39.1957719814113,39.2836434636597,
39.3028389860875,39.3907026547579,39.4784564049676,39.5661231726209,39.6565219721114,
39.7440917538913,39.8316490046101,39.9192143235875,40.0068083108156,40.0944985585765,
40.1822465617651,40.2701180437678,40.2893135685443,40.3795378388649,40.4696301596092,
40.5623987438737,40.6522493144927,40.74647690558,40.8407044966673),
 .UNSPECIFIED.);
#1315=B_SPLINE_CURVE_WITH_KNOTS('',3,(#8514,#8515,#8516,#8517,#8518,#8519,
#8520,#8521,#8522,#8523,#8524,#8525,#8526,#8527,#8528,#8529,#8530,#8531,
#8532,#8533,#8534,#8535,#8536,#8537,#8538,#8539,#8540,#8541,#8542,#8543,
#8544,#8545,#8546,#8547),.UNSPECIFIED.,.F.,.F.,(4,3,3,3,3,3,3,3,3,3,3,4),
(40.840704496799,40.9348549665562,41.0293618567931,41.1240517300647,41.2190251707754,
41.2757881510011,41.3636473621912,41.451401427047,41.540890908233,41.6284903539905,
41.7189248528907,41.8093593517908),.UNSPECIFIED.);
#1316=B_SPLINE_CURVE_WITH_KNOTS('',3,(#8549,#8550,#8551,#8552,#8553,#8554,
#8555,#8556,#8557,#8558,#8559,#8560,#8561,#8562,#8563,#8564,#8565,#8566,
#8567,#8568,#8569,#8570,#8571,#8572,#8573,#8574,#8575,#8576,#8577,#8578,
#8579,#8580,#8581,#8582,#8583,#8584,#8585),.UNSPECIFIED.,.F.,.F.,(4,3,3,
3,3,3,3,3,3,3,3,3,4),(40.8407044966673,40.8579522275318,40.9458179320816,
41.0335732153263,41.121241015274,41.2088441090132,41.2964126890953,41.3839673694283,
41.4715287488756,41.5591660707284,41.6468417480247,41.7346436206963,41.8092918158648),
 .UNSPECIFIED.);
#1317=B_SPLINE_CURVE_WITH_KNOTS('',3,(#8586,#8587,#8588,#8589,#8590,#8591,
#8592,#8593,#8594,#8595,#8596,#8597,#8598,#8599,#8600,#8601,#8602,#8603,
#8604,#8605,#8606,#8607,#8608,#8609,#8610,#8611,#8612,#8613,#8614,#8615,
#8616,#8617,#8618,#8619,#8620,#8621,#8622,#8623,#8624,#8625,#8626,#8627,
#8628,#8629,#8630,#8631,#8632,#8633,#8634,#8635,#8636,#8637,#8638,#8639,
#8640,#8641,#8642,#8643,#8644,#8645,#8646,#8647,#8648,#8649,#8650,#8651,
#8652,#8653,#8654,#8655,#8656,#8657,#8658,#8659,#8660,#8661,#8662,#8663,
#8664,#8665,#8666,#8667,#8668,#8669,#8670,#8671,#8672,#8673,#8674,#8675,
#8676,#8677,#8678,#8679,#8680,#8681,#8682,#8683,#8684,#8685,#8686,#8687,
#8688,#8689,#8690,#8691,#8692,#8693,#8694,#8695,#8696,#8697,#8698,#8699,
#8700,#8701,#8702,#8703,#8704,#8705,#8706,#8707,#8708,#8709,#8710,#8711,
#8712,#8713,#8714,#8715,#8716,#8717,#8718,#8719,#8720,#8721,#8722,#8723,
#8724,#8725,#8726,#8727,#8728,#8729,#8730,#8731,#8732,#8733,#8734,#8735,
#8736,#8737,#8738,#8739,#8740,#8741,#8742,#8743,#8744,#8745,#8746,#8747,
#8748,#8749,#8750,#8751,#8752,#8753,#8754,#8755,#8756,#8757,#8758,#8759,
#8760,#8761,#8762,#8763,#8764,#8765,#8766,#8767,#8768,#8769,#8770,#8771,
#8772,#8773,#8774,#8775,#8776,#8777,#8778),.UNSPECIFIED.,.F.,.F.,(4,3,3,
3,3,3,3,3,3,3,3,3,3,3,3,3,3,3,3,3,3,3,3,3,3,3,3,3,3,3,3,3,3,3,3,3,3,3,3,
3,3,3,3,3,3,3,3,3,3,3,3,3,3,3,3,3,3,3,3,3,3,3,3,3,4),(35.5260257192705,
35.6136077753379,35.7012827832995,35.7890093143363,35.8768671942592,35.9255793152477,
36.0134429833182,36.1011967329437,36.1888635000296,36.279262299739,36.3668320809955,
36.4543893312083,36.5419546496982,36.6295486364565,36.7172388837792,36.8049868865467,
36.8928583681567,36.9120538977045,36.9999175641475,37.0876713120909,37.1753380774423,
37.2657368777822,37.3533066571848,37.4408639055025,37.5284292220579,37.6160232068443,
37.7037134521494,37.7914614528703,37.8793329324066,37.8985284801614,37.9863921502957,
38.0741459019874,38.1618126711394,38.2522114700742,38.3397812533827,38.4273385056385,
38.51490382616,38.6024978149364,38.6901880642466,38.777936068986,38.8658075525305,
38.8850030626182,38.9728667311203,39.060620481162,39.1482872486483,39.2386860482016,
39.3262558298162,39.4138130803705,39.5013783991851,39.5889723862506,39.6766626338531,
39.7644106368846,39.8522821187338,39.871477645075,39.9590839627409,40.046580472658,
40.1339904231532,40.2223296823268,40.3096449944239,40.3969485865632,40.4842613371711,
40.5733721270138,40.6608118986615,40.7507581976017,40.8407044965419),
 .UNSPECIFIED.);
#1318=B_SPLINE_CURVE_WITH_KNOTS('',3,(#8784,#8785,#8786,#8787,#8788,#8789,
#8790,#8791,#8792,#8793,#8794,#8795,#8796,#8797,#8798,#8799,#8800,#8801,
#8802,#8803,#8804,#8805,#8806,#8807,#8808,#8809,#8810,#8811,#8812,#8813,
#8814,#8815,#8816,#8817,#8818,#8819,#8820,#8821,#8822,#8823,#8824,#8825,
#8826,#8827,#8828,#8829,#8830,#8831,#8832,#8833,#8834,#8835,#8836,#8837,
#8838,#8839,#8840,#8841,#8842,#8843,#8844,#8845,#8846,#8847,#8848,#8849,
#8850,#8851,#8852,#8853,#8854,#8855,#8856,#8857,#8858,#8859,#8860,#8861,
#8862,#8863,#8864,#8865,#8866,#8867,#8868,#8869,#8870,#8871,#8872,#8873,
#8874,#8875,#8876,#8877,#8878,#8879,#8880,#8881,#8882,#8883,#8884,#8885,
#8886,#8887,#8888,#8889,#8890,#8891,#8892,#8893,#8894,#8895,#8896,#8897,
#8898,#8899,#8900,#8901,#8902,#8903,#8904,#8905,#8906,#8907,#8908,#8909,
#8910,#8911,#8912,#8913,#8914,#8915,#8916,#8917,#8918,#8919,#8920,#8921,
#8922,#8923,#8924,#8925,#8926,#8927,#8928,#8929,#8930,#8931,#8932,#8933,
#8934,#8935,#8936,#8937,#8938,#8939,#8940,#8941,#8942,#8943,#8944,#8945,
#8946,#8947,#8948,#8949,#8950,#8951,#8952,#8953,#8954,#8955,#8956,#8957,
#8958,#8959,#8960,#8961,#8962,#8963,#8964,#8965,#8966,#8967,#8968,#8969,
#8970,#8971,#8972,#8973,#8974,#8975,#8976,#8977,#8978,#8979),
 .UNSPECIFIED.,.F.,.F.,(4,3,3,3,3,3,3,3,3,3,3,3,3,3,3,3,3,3,3,3,3,3,3,3,
3,3,3,3,3,3,3,3,3,3,3,3,3,3,3,3,3,3,3,3,3,3,3,3,3,3,3,3,3,3,3,3,3,3,3,3,
3,3,3,3,3,4),(29.2425482859762,29.3302955402787,29.4181664625321,29.4380931615194,
29.525956904785,29.613710730384,29.7013775741223,29.791776345354,29.8793462044527,
29.9669035328111,30.0544689296637,30.1420629949156,30.2297533205319,30.3175014015646,
30.4053729608139,30.4245677439762,30.5124314160683,30.6001851699415,30.687851941495,
30.7782507396122,30.8658205258578,30.9533777812449,31.0409431050895,31.1285370973784,
31.2162273504652,31.3039753591402,31.3918468468228,31.411042326433,31.4989059745539,
31.5866597038815,31.6743264503483,31.764725257666,31.8522950176361,31.9398522463518,
32.0274175431573,32.1150115080668,32.202701733406,32.2904497140863,32.3783211736226,
32.3975169088898,32.4853805881456,32.5731343490644,32.660801127537,32.7511999230132,
32.8387697158143,32.9263269776097,33.0138923077074,33.101486306086,33.1891765649889,
33.2769245793264,33.3647960724051,33.3839914913466,33.4718551594076,33.5596089090236,
33.6472756761,33.737674475813,33.8252442570602,33.9128015072637,34.0003668257444,
34.0879608124935,34.1756510598073,34.2633990625659,34.3512705441674,34.3704660738034,
34.4979605070231,34.5575191894877),.UNSPECIFIED.);
#1319=B_SPLINE_CURVE_WITH_KNOTS('',3,(#8980,#8981,#8982,#8983,#8984,#8985,
#8986,#8987,#8988,#8989,#8990,#8991,#8992,#8993,#8994,#8995,#8996,#8997,
#8998,#8999,#9000,#9001,#9002,#9003,#9004,#9005,#9006,#9007,#9008,#9009,
#9010,#9011,#9012,#9013,#9014,#9015,#9016),.UNSPECIFIED.,.F.,.F.,(4,3,3,
3,3,3,3,3,3,3,3,3,4),(34.5575191896929,34.6439788935642,34.7330991139012,
34.8194341984083,34.9057479013124,34.9920619722673,35.0783981577317,35.1648239857159,
35.2513038501986,35.3379043039037,35.3569406562602,35.4447862511981,35.5268366911762),
 .UNSPECIFIED.);
#1320=B_SPLINE_CURVE_WITH_KNOTS('',3,(#9018,#9019,#9020,#9021,#9022,#9023,
#9024,#9025,#9026,#9027,#9028,#9029,#9030,#9031,#9032,#9033,#9034,#9035,
#9036,#9037,#9038,#9039,#9040,#9041,#9042,#9043,#9044,#9045,#9046,#9047,
#9048,#9049,#9050,#9051),.UNSPECIFIED.,.F.,.F.,(4,3,3,3,3,3,3,3,3,3,3,4),
(34.5575191896899,34.6549831946974,34.7527736528568,34.8510352792918,34.9391047327909,
35.0269585210482,35.1147082551822,35.2023747117386,35.289976688806,35.3775401437585,
35.465101297594,35.5260257192705),.UNSPECIFIED.);
#1321=B_SPLINE_CURVE_WITH_KNOTS('',3,(#9052,#9053,#9054,#9055,#9056,#9057,
#9058,#9059,#9060,#9061,#9062,#9063,#9064,#9065,#9066,#9067,#9068,#9069,
#9070,#9071,#9072,#9073,#9074,#9075,#9076,#9077,#9078,#9079,#9080,#9081,
#9082,#9083,#9084,#9085,#9086,#9087,#9088,#9089,#9090,#9091,#9092,#9093,
#9094,#9095,#9096,#9097,#9098,#9099,#9100,#9101,#9102,#9103,#9104,#9105,
#9106,#9107,#9108,#9109,#9110,#9111,#9112,#9113,#9114,#9115,#9116,#9117,
#9118,#9119,#9120,#9121,#9122,#9123,#9124,#9125,#9126,#9127,#9128,#9129,
#9130,#9131,#9132,#9133,#9134,#9135,#9136,#9137,#9138,#9139,#9140,#9141,
#9142,#9143,#9144,#9145,#9146,#9147,#9148,#9149,#9150,#9151,#9152,#9153,
#9154,#9155,#9156,#9157,#9158,#9159,#9160,#9161,#9162,#9163,#9164,#9165,
#9166,#9167,#9168,#9169,#9170,#9171,#9172,#9173,#9174,#9175,#9176,#9177,
#9178,#9179,#9180,#9181,#9182,#9183,#9184,#9185,#9186,#9187,#9188,#9189,
#9190,#9191,#9192,#9193,#9194,#9195,#9196,#9197,#9198,#9199,#9200,#9201,
#9202,#9203,#9204,#9205,#9206,#9207,#9208,#9209,#9210,#9211,#9212,#9213,
#9214,#9215,#9216,#9217,#9218,#9219,#9220,#9221,#9222,#9223,#9224,#9225,
#9226,#9227,#9228,#9229,#9230,#9231,#9232,#9233,#9234,#9235,#9236,#9237,
#9238,#9239,#9240,#9241,#9242,#9243,#9244),.UNSPECIFIED.,.F.,.F.,(4,3,3,
3,3,3,3,3,3,3,3,3,3,3,3,3,3,3,3,3,3,3,3,3,3,3,3,3,3,3,3,3,3,3,3,3,3,3,3,
3,3,3,3,3,3,3,3,3,3,3,3,3,3,3,3,3,3,3,3,3,3,3,3,3,4),(29.243664967692,29.3312944627721,
29.4188783169648,29.5064396083037,29.5939989404945,29.6815769108029,29.7692462733555,
29.8569643702558,29.9448174904114,30.0067318205069,30.0945955831954,30.1823494302193,
30.2700162973492,30.360415060551,30.447984947815,30.5355423060676,30.6231077345184,
30.7107018330489,30.7983921942754,30.8861403123251,30.9740119103669,30.9932064029637,
31.0810698948999,31.1688234656784,31.2564900514433,31.3468889181904,31.4344585131339,
31.522015575508,31.6095807048371,31.697174501315,31.7848645576492,31.872612368797,
31.9604836592968,31.9796809854205,32.0675447282664,32.1552985534412,32.2429653967515,
32.3333641681422,32.420934026805,32.5084913547255,32.5960567511386,32.6836508159498,
32.771341141126,32.8590892217185,32.9469607805306,32.9661555678773,33.0540192399948,
33.1417729938924,33.2294397654696,33.3198385635777,33.4074083498455,33.4949656052541,
33.5825309291192,33.6701249214278,33.7578151745333,33.8455631832266,33.9334346709259,
33.9526301503341,34.0414524496082,34.1301581696792,34.2187666849647,34.3072860964107,
34.395752460746,34.484192796774,34.5575191894877),.UNSPECIFIED.);
#1322=B_SPLINE_CURVE_WITH_KNOTS('',3,(#9250,#9251,#9252,#9253,#9254,#9255,
#9256,#9257,#9258,#9259,#9260,#9261,#9262,#9263,#9264,#9265,#9266,#9267,
#9268,#9269,#9270,#9271,#9272,#9273,#9274,#9275,#9276,#9277,#9278,#9279,
#9280,#9281,#9282,#9283),.UNSPECIFIED.,.F.,.F.,(4,3,3,3,3,3,3,3,3,3,3,4),
(21.9911485751285,22.1149351608524,22.2027160146711,22.2903837338802,22.3779478024412,
22.4654536992169,22.5529221753128,22.6403739494206,22.7278622838359,22.8153692328211,
22.9029614226615,22.959407626261),.UNSPECIFIED.);
#1323=B_SPLINE_CURVE_WITH_KNOTS('',3,(#9285,#9286,#9287,#9288,#9289,#9290,
#9291),.UNSPECIFIED.,.F.,.F.,(4,1,1,1,4),(18.1690368310252,19.155511413482,
20.1419859959388,21.1284605783956,21.9911407069303),.UNSPECIFIED.);
#1324=B_SPLINE_CURVE_WITH_KNOTS('',3,(#9295,#9296,#9297,#9298,#9299,#9300,
#9301,#9302,#9303,#9304,#9305,#9306,#9307,#9308,#9309,#9310,#9311,#9312,
#9313,#9314,#9315,#9316,#9317,#9318,#9319,#9320,#9321,#9322,#9323,#9324,
#9325,#9326,#9327,#9328,#9329,#9330,#9331,#9332,#9333,#9334,#9335,#9336,
#9337,#9338,#9339,#9340,#9341,#9342,#9343,#9344,#9345,#9346,#9347,#9348,
#9349,#9350,#9351,#9352,#9353,#9354,#9355,#9356,#9357,#9358,#9359,#9360,
#9361,#9362,#9363,#9364,#9365,#9366,#9367,#9368,#9369,#9370,#9371,#9372,
#9373,#9374,#9375,#9376,#9377,#9378,#9379,#9380,#9381,#9382,#9383,#9384,
#9385,#9386,#9387,#9388,#9389,#9390,#9391,#9392,#9393,#9394,#9395,#9396,
#9397,#9398,#9399,#9400,#9401,#9402,#9403,#9404,#9405,#9406,#9407,#9408,
#9409,#9410,#9411,#9412,#9413,#9414,#9415,#9416,#9417,#9418,#9419,#9420,
#9421,#9422,#9423,#9424,#9425,#9426,#9427,#9428,#9429,#9430,#9431,#9432,
#9433,#9434,#9435,#9436,#9437,#9438,#9439,#9440,#9441,#9442,#9443,#9444,
#9445,#9446,#9447,#9448,#9449,#9450,#9451),.UNSPECIFIED.,.F.,.F.,(4,3,3,
3,3,3,3,3,3,3,3,3,3,3,3,3,3,3,3,3,3,3,3,3,3,3,3,3,3,3,3,3,3,3,3,3,3,3,3,
3,3,3,3,3,3,3,3,3,3,3,3,3,4),(17.6451204658269,17.7324138960806,17.8195992142952,
17.9066999959299,17.9937421922357,18.080753937747,18.167756417921,18.2547708066079,
18.3418700810798,18.4290131909813,18.5162907440526,18.5868727544945,18.6748711844211,
18.7627621489718,18.8505683956313,18.9409157632963,19.0286297421553,19.1163326847563,
19.2040450297739,19.2963706065682,19.3842126461842,19.4721141501259,19.5601379184068,
19.5733473369513,19.661119323604,19.7487802196365,19.8363530814819,19.9267866862227,
20.0142605428918,20.1017212859224,20.1891896184029,20.2766862438119,20.3642790579177,
20.4519294732645,20.5397038712882,20.5598219194081,20.6477025677944,20.7354733506331,
20.8231571819731,20.9135495969596,21.0011364059084,21.0887106394504,21.1762928775113,
21.2639037006302,21.3516105759406,21.4393751033165,21.5272628354399,21.5462965018649,
21.6407892334465,21.7349872067073,21.8290035864883,21.9227454576979,21.9911485749053),
 .UNSPECIFIED.);
#1325=B_SPLINE_CURVE_WITH_KNOTS('',3,(#9452,#9453,#9454,#9455,#9456,#9457,
#9458,#9459,#9460,#9461,#9462,#9463,#9464,#9465,#9466,#9467,#9468,#9469,
#9470,#9471,#9472,#9473,#9474,#9475,#9476,#9477,#9478,#9479,#9480,#9481,
#9482,#9483,#9484,#9485),.UNSPECIFIED.,.F.,.F.,(4,3,3,3,3,3,3,3,3,3,3,4),
(21.9911485751285,22.081189059175,22.1712954056986,22.2616643253544,22.3520075127491,
22.442539438158,22.5327710843217,22.6206308683745,22.7083577673478,22.7960076583844,
22.8835975443804,22.9601178369312),.UNSPECIFIED.);
#1326=B_SPLINE_CURVE_WITH_KNOTS('',3,(#9491,#9492,#9493,#9494),
 .UNSPECIFIED.,.F.,.F.,(4,4),(47.7645509873098,47.8044058628387),
 .UNSPECIFIED.);
#1327=B_SPLINE_CURVE_WITH_KNOTS('',3,(#9496,#9497,#9498,#9499,#9500,#9501,
#9502,#9503,#9504,#9505,#9506,#9507,#9508,#9509,#9510,#9511,#9512,#9513,
#9514,#9515,#9516,#9517,#9518,#9519,#9520,#9521,#9522,#9523,#9524,#9525,
#9526,#9527,#9528,#9529,#9530,#9531,#9532,#9533,#9534,#9535,#9536,#9537,
#9538,#9539,#9540,#9541,#9542,#9543,#9544,#9545,#9546,#9547,#9548,#9549,
#9550,#9551,#9552,#9553,#9554,#9555,#9556,#9557,#9558,#9559,#9560,#9561,
#9562,#9563,#9564,#9565,#9566,#9567,#9568,#9569,#9570,#9571,#9572,#9573,
#9574,#9575,#9576,#9577,#9578,#9579,#9580,#9581,#9582,#9583,#9584,#9585,
#9586,#9587,#9588,#9589,#9590,#9591,#9592,#9593,#9594,#9595,#9596,#9597,
#9598,#9599,#9600,#9601,#9602,#9603,#9604,#9605,#9606,#9607,#9608,#9609,
#9610,#9611,#9612,#9613,#9614,#9615,#9616,#9617,#9618,#9619,#9620,#9621,
#9622,#9623,#9624,#9625,#9626,#9627,#9628,#9629,#9630,#9631,#9632,#9633,
#9634,#9635,#9636,#9637,#9638,#9639,#9640,#9641,#9642,#9643,#9644,#9645,
#9646),.UNSPECIFIED.,.F.,.F.,(4,3,3,3,3,3,3,3,3,3,3,3,3,3,3,3,3,3,3,3,3,
3,3,3,3,3,3,3,3,3,3,3,3,3,3,3,3,3,3,3,3,3,3,3,3,3,3,3,3,3,4),(47.8044088943605,
47.8988458715296,47.9933637699636,48.0880590284704,48.1828496682947,48.2778377921346,
48.3372545403837,48.4294696563408,48.5215643431454,48.6135647748162,48.7054993456098,
48.7973996202586,48.889289121424,48.9811913568557,49.0731852010223,49.1652272928627,
49.257412825594,49.3237291228405,49.41585789497,49.5078683040179,49.5997866059479,
49.6916425715041,49.7834664330782,49.8752817926359,49.9671122390392,50.0590383362072,
50.1510148357375,50.243138907479,50.3102037052973,50.4014179770184,50.4925118584179,
50.5835127350798,50.6744535421951,50.7653638250799,50.8562681794588,50.9471911906559,
51.0382208929196,51.1293056432464,51.2205548827498,51.2966782877541,51.3911470133568,
51.4854792917811,51.5796967693301,51.6738054165067,51.7678505381326,51.8618515310768,
51.9558277481792,52.0498237215135,52.1438284502303,52.2378954387847,52.2831528702109),
 .UNSPECIFIED.);
#1328=B_SPLINE_CURVE_WITH_KNOTS('',3,(#9650,#9651,#9652,#9653,#9654,#9655,
#9656,#9657,#9658,#9659,#9660,#9661,#9662,#9663,#9664,#9665,#9666,#9667,
#9668,#9669,#9670,#9671,#9672,#9673,#9674,#9675,#9676,#9677,#9678,#9679,
#9680,#9681,#9682,#9683,#9684,#9685,#9686,#9687,#9688,#9689,#9690,#9691,
#9692,#9693,#9694,#9695,#9696,#9697,#9698,#9699,#9700,#9701,#9702,#9703,
#9704,#9705,#9706,#9707,#9708,#9709,#9710,#9711,#9712,#9713,#9714,#9715,
#9716,#9717,#9718,#9719,#9720,#9721,#9722,#9723,#9724,#9725,#9726,#9727,
#9728,#9729,#9730,#9731,#9732,#9733,#9734,#9735,#9736,#9737,#9738,#9739,
#9740,#9741,#9742,#9743,#9744,#9745,#9746,#9747,#9748,#9749,#9750,#9751,
#9752,#9753,#9754,#9755,#9756,#9757,#9758,#9759,#9760,#9761,#9762,#9763,
#9764,#9765,#9766,#9767,#9768,#9769,#9770,#9771,#9772,#9773,#9774,#9775,
#9776,#9777,#9778,#9779,#9780,#9781,#9782,#9783,#9784,#9785,#9786,#9787,
#9788,#9789,#9790,#9791,#9792,#9793,#9794,#9795,#9796,#9797,#9798,#9799,
#9800,#9801,#9802,#9803,#9804,#9805,#9806,#9807,#9808,#9809,#9810,#9811,
#9812,#9813,#9814,#9815,#9816,#9817,#9818,#9819,#9820,#9821,#9822,#9823,
#9824,#9825,#9826,#9827,#9828,#9829,#9830,#9831,#9832,#9833,#9834,#9835,
#9836,#9837,#9838,#9839,#9840,#9841,#9842,#9843,#9844,#9845,#9846,#9847,
#9848,#9849,#9850,#9851,#9852,#9853,#9854,#9855,#9856,#9857),
 .UNSPECIFIED.,.F.,.F.,(4,3,3,3,3,3,3,3,3,3,3,3,3,3,3,3,3,3,3,3,3,3,3,3,
3,3,3,3,3,3,3,3,3,3,3,3,3,3,3,3,3,3,3,3,3,3,3,3,3,3,3,3,3,3,3,3,3,3,3,3,
3,3,3,3,3,3,3,3,3,4),(-50.2654642069239,-50.174002871108,-50.0826595972117,
-49.9877932879153,-49.8966027347253,-49.8054407495249,-49.7142829692658,
-49.6231050404631,-49.5318321853382,-49.440502858591,-49.3490411078306,
-49.3237291228405,-49.2315291015422,-49.1394464590948,-49.0474550341997,
-48.9555248846661,-48.8636262123592,-48.7717354971473,-48.6798292315804,
-48.5878270327216,-48.4957741651475,-48.4035740334089,-48.3372545403837,
-48.245291774167,-48.1534503585896,-48.0617037771693,-47.9700228870573,
-47.8783760922691,-47.7867395670033,-47.6950894999377,-47.6033450470191,
-47.5115511593569,-47.4196094077833,-47.3507799579269,-47.2587033417908,
-47.1667467351112,-47.0748837851034,-46.9830852378435,-46.8913200370523,
-46.7995644990034,-46.7077949539867,-46.6159310309032,-46.5240175020027,
-46.4319570406068,-46.36430537547,-46.2722322020199,-46.1802787999358,-46.088418812967,
-45.9966228505351,-45.9048600007786,-45.8131065761715,-45.7213389030145,
-45.6294764629031,-45.5375642026684,-45.4455046445268,-45.3778307930132,
-45.285784361828,-45.1938581747992,-45.1020258358177,-45.0102580580154,
-44.9185237121079,-44.8267990763685,-44.7350604431189,-44.6432272555675,
-44.5513444087202,-44.4593142303005,-44.3913562105564,-44.2836645683137,
-44.1732379897799,-44.0628114112462),.UNSPECIFIED.);
#1329=B_SPLINE_CURVE_WITH_KNOTS('',3,(#9858,#9859,#9860,#9861),
 .UNSPECIFIED.,.F.,.F.,(4,4),(-44.062811411082,-44.0219726945388),
 .UNSPECIFIED.);
#1330=B_SPLINE_CURVE_WITH_KNOTS('',3,(#9867,#9868,#9869,#9870),
 .UNSPECIFIED.,.F.,.F.,(4,4),(41.481273340989,41.5212235871809),
 .UNSPECIFIED.);
#1331=B_SPLINE_CURVE_WITH_KNOTS('',3,(#9871,#9872,#9873,#9874,#9875,#9876,
#9877,#9878,#9879,#9880),.UNSPECIFIED.,.F.,.F.,(4,1,1,1,1,1,1,4),(41.5212316192577,
42.4184070456428,43.4048816280996,44.3913562105564,45.3778307930133,46.3643053754701,
47.3507799579269,47.7645509873098),.UNSPECIFIED.);
#1332=B_SPLINE_CURVE_WITH_KNOTS('',3,(#9882,#9883,#9884,#9885,#9886,#9887,
#9888,#9889,#9890,#9891,#9892,#9893,#9894,#9895,#9896,#9897,#9898,#9899,
#9900,#9901,#9902,#9903,#9904,#9905,#9906,#9907,#9908,#9909,#9910,#9911,
#9912,#9913,#9914,#9915,#9916,#9917,#9918,#9919,#9920,#9921,#9922,#9923,
#9924,#9925,#9926,#9927,#9928,#9929,#9930,#9931,#9932,#9933,#9934,#9935,
#9936,#9937,#9938,#9939,#9940,#9941,#9942,#9943,#9944,#9945,#9946,#9947,
#9948,#9949,#9950,#9951,#9952,#9953,#9954,#9955,#9956,#9957,#9958,#9959,
#9960,#9961,#9962,#9963,#9964,#9965,#9966,#9967,#9968,#9969,#9970,#9971,
#9972,#9973,#9974,#9975,#9976,#9977,#9978,#9979,#9980,#9981,#9982,#9983,
#9984,#9985,#9986,#9987,#9988,#9989,#9990,#9991,#9992,#9993,#9994,#9995,
#9996,#9997,#9998,#9999,#10000,#10001,#10002,#10003,#10004,#10005,#10006,
#10007,#10008,#10009,#10010,#10011,#10012,#10013,#10014,#10015,#10016,#10017,
#10018,#10019,#10020,#10021,#10022,#10023,#10024,#10025,#10026,#10027,#10028,
#10029,#10030,#10031,#10032,#10033,#10034,#10035,#10036,#10037,#10038,#10039,
#10040,#10041,#10042,#10043,#10044,#10045,#10046,#10047,#10048,#10049,#10050,
#10051,#10052,#10053,#10054,#10055,#10056,#10057,#10058,#10059,#10060,#10061,
#10062,#10063,#10064,#10065,#10066,#10067,#10068,#10069,#10070,#10071,#10072,
#10073,#10074,#10075,#10076,#10077,#10078,#10079,#10080,#10081,#10082,#10083,
#10084,#10085,#10086,#10087,#10088,#10089,#10090,#10091,#10092),
 .UNSPECIFIED.,.F.,.F.,(4,3,3,3,3,3,3,3,3,3,3,3,3,3,3,3,3,3,3,3,3,3,3,3,
3,3,3,3,3,3,3,3,3,3,3,3,3,3,3,3,3,3,3,3,3,3,3,3,3,3,3,3,3,3,3,3,3,3,3,3,
3,3,3,3,3,3,3,3,3,3,4),(-44.0219726945388,-43.9302993798164,-43.8386303041183,
-43.746941779298,-43.6551507631959,-43.5633054158736,-43.4713063922967,
-43.4048816280996,-43.3128214862464,-43.2208813800638,-43.1290349336417,
-43.0372528238165,-42.9455040132506,-42.8537647976379,-42.7620114866317,
-42.6701635590492,-42.5782659160732,-42.4862209992494,-42.4184070456428,
-42.3263497646008,-42.234412573871,-42.1425690932578,-42.0507900127371,
-41.9590442693662,-41.8673081551732,-41.7755579761731,-41.6837132090212,
-41.5918187468843,-41.4997770122276,-41.431932463186,-41.3398731138376,
-41.2479338264137,-41.1560882237537,-41.0643069919101,-40.9725590800402,
-40.880820782799,-40.7890684088164,-40.6972214416019,-40.6053247733791,
-40.5132808450966,-40.4454578807292,-40.3533989564471,-40.2614600960634,
-40.1696149218158,-40.0778341186257,-39.9860866353904,-39.8943487662328,
-39.8025968192505,-39.7107502747056,-39.6188540273564,-39.5268105127238,
-39.4589832982724,-39.3669246585381,-39.2749860887432,-39.183141210696,
-39.0913607109285,-38.9996135354415,-38.9078759779926,-38.816124346316,
-38.724278120748,-38.6323821948822,-38.5403390025968,-38.4725087158156,
-38.3810288132208,-38.2896616015582,-38.1983825809915,-38.1071673347784,
-38.0159770156749,-37.9248025582061,-37.8335885854587,-37.7796261039024),
 .UNSPECIFIED.);
#1333=B_SPLINE_CURVE_WITH_KNOTS('',3,(#10093,#10094,#10095,#10096),
 .UNSPECIFIED.,.F.,.F.,(4,4),(-37.7796261036537,-37.7402431363199),
 .UNSPECIFIED.);
#1334=B_SPLINE_CURVE_WITH_KNOTS('',3,(#10102,#10103,#10104,#10105),
 .UNSPECIFIED.,.F.,.F.,(4,4),(-0.01489375026152,-0.000951714991103148),
 .UNSPECIFIED.);
#1335=B_SPLINE_CURVE_WITH_KNOTS('',3,(#10106,#10107,#10108,#10109,#10110,
#10111,#10112,#10113,#10114,#10115,#10116,#10117,#10118,#10119,#10120,#10121,
#10122,#10123,#10124,#10125,#10126,#10127,#10128,#10129,#10130,#10131,#10132,
#10133,#10134,#10135,#10136,#10137,#10138,#10139,#10140,#10141,#10142,#10143,
#10144,#10145,#10146,#10147,#10148,#10149,#10150,#10151,#10152,#10153,#10154,
#10155,#10156,#10157,#10158,#10159,#10160,#10161,#10162,#10163,#10164,#10165,
#10166,#10167,#10168,#10169,#10170,#10171,#10172,#10173,#10174,#10175,#10176,
#10177,#10178,#10179,#10180,#10181,#10182,#10183,#10184,#10185,#10186,#10187,
#10188,#10189,#10190,#10191,#10192,#10193,#10194,#10195,#10196,#10197,#10198,
#10199,#10200,#10201,#10202,#10203,#10204,#10205,#10206,#10207,#10208,#10209,
#10210,#10211,#10212,#10213,#10214,#10215,#10216,#10217,#10218,#10219,#10220,
#10221,#10222,#10223,#10224,#10225,#10226,#10227,#10228,#10229,#10230,#10231,
#10232,#10233,#10234,#10235,#10236,#10237,#10238,#10239,#10240,#10241,#10242,
#10243,#10244,#10245,#10246,#10247,#10248,#10249,#10250,#10251,#10252,#10253,
#10254,#10255,#10256,#10257,#10258,#10259,#10260,#10261,#10262,#10263,#10264,
#10265,#10266,#10267,#10268,#10269,#10270,#10271,#10272,#10273,#10274,#10275,
#10276,#10277,#10278,#10279,#10280,#10281,#10282,#10283,#10284,#10285,#10286,
#10287,#10288,#10289,#10290,#10291,#10292,#10293,#10294,#10295,#10296,#10297,
#10298,#10299,#10300,#10301,#10302,#10303,#10304,#10305,#10306,#10307,#10308,
#10309,#10310,#10311,#10312,#10313,#10314,#10315,#10316),.UNSPECIFIED.,
 .F.,.F.,(4,3,3,3,3,3,3,3,3,3,3,3,3,3,3,3,3,3,3,3,3,3,3,3,3,3,3,3,3,3,3,
3,3,3,3,3,3,3,3,3,3,3,3,3,3,3,3,3,3,3,3,3,3,3,3,3,3,3,3,3,3,3,3,3,3,3,3,
3,3,3,4),(35.2380382801875,35.3506623506834,35.4649882294613,35.5130849684452,
35.6051437708323,35.6970825062651,35.7889275526903,35.8807082242548,35.9724555735748,
36.0641933066831,36.1559451156365,36.2477915199073,36.3396876255291,36.4317309974756,
36.499559550902,36.5916183825352,36.683557146995,36.7754022221935,36.8671829220369,
36.9589302993224,37.0506680600512,37.1424198962478,37.2342663270164,37.32616245876,
37.4182058559552,37.4860341333588,37.5780930392207,37.6700318784838,37.7618770289539,
37.8536578044556,37.9454052576079,38.0371430943186,38.1288950065193,38.2207415128571,
38.3126377200377,38.4046811916876,38.4725087158156,38.5645673417354,38.6565059006634,
38.7483507707782,38.8401312670426,38.9318784417468,39.0236160011304,39.1153676374572,
39.2072138718485,39.2991098088712,39.3911530160044,39.4589832982724,39.5510422449303,
39.6429811231728,39.7348263107813,39.8266071205372,39.9183546061647,40.0100924735443,
40.1018444145791,40.1936909467628,40.2855871781657,40.37763067117,40.4454578807292,
40.5375172362535,40.6294565280628,40.7213021333286,40.8130833651009,40.9048312752559,
40.9965695691435,41.0883219381371,41.1801688978633,41.2720655571968,41.3641094743968,
41.431932463186,41.481273340989),.UNSPECIFIED.);
#1336=B_SPLINE_CURVE_WITH_KNOTS('',3,(#10318,#10319,#10320,#10321,#10322,
#10323,#10324,#10325,#10326,#10327,#10328,#10329,#10330,#10331,#10332,#10333,
#10334,#10335,#10336,#10337,#10338,#10339,#10340,#10341,#10342,#10343,#10344,
#10345,#10346,#10347,#10348,#10349,#10350,#10351,#10352,#10353,#10354,#10355,
#10356,#10357,#10358,#10359,#10360,#10361,#10362,#10363,#10364,#10365,#10366,
#10367,#10368,#10369,#10370,#10371,#10372,#10373,#10374,#10375,#10376,#10377,
#10378,#10379,#10380,#10381,#10382,#10383,#10384,#10385,#10386,#10387,#10388,
#10389,#10390,#10391,#10392,#10393,#10394,#10395,#10396,#10397,#10398,#10399,
#10400,#10401,#10402,#10403,#10404,#10405,#10406,#10407,#10408,#10409,#10410,
#10411,#10412,#10413,#10414,#10415,#10416,#10417,#10418,#10419,#10420,#10421,
#10422,#10423,#10424,#10425,#10426,#10427,#10428,#10429,#10430,#10431,#10432,
#10433,#10434,#10435,#10436,#10437,#10438,#10439,#10440,#10441,#10442,#10443,
#10444,#10445,#10446,#10447,#10448,#10449,#10450,#10451,#10452,#10453,#10454,
#10455,#10456,#10457,#10458,#10459,#10460,#10461,#10462,#10463,#10464,#10465,
#10466,#10467,#10468,#10469,#10470,#10471,#10472,#10473,#10474,#10475,#10476,
#10477,#10478,#10479,#10480,#10481,#10482,#10483,#10484,#10485,#10486,#10487,
#10488,#10489,#10490,#10491,#10492,#10493,#10494,#10495,#10496,#10497,#10498,
#10499,#10500,#10501,#10502,#10503,#10504,#10505,#10506,#10507,#10508,#10509,
#10510,#10511,#10512,#10513,#10514,#10515,#10516,#10517,#10518,#10519,#10520,
#10521,#10522,#10523,#10524,#10525,#10526,#10527,#10528),.UNSPECIFIED.,
 .F.,.F.,(4,3,3,3,3,3,3,3,3,3,3,3,3,3,3,3,3,3,3,3,3,3,3,3,3,3,3,3,3,3,3,
3,3,3,3,3,3,3,3,3,3,3,3,3,3,3,3,3,3,3,3,3,3,3,3,3,3,3,3,3,3,3,3,3,3,3,3,
3,3,3,4),(-37.7402431363199,-37.6296257451957,-37.5178108639187,-37.4860341333588,
-37.3939753040707,-37.3020365414895,-37.210191467705,-37.1184107685739,
-37.0266633915695,-36.9349256306911,-36.8431737939141,-36.7513273619022,
-36.6594312285449,-36.5673878291486,-36.4995595509019,-36.4075007467294,
-36.3155620098938,-36.2237169624464,-36.1319362904343,-36.0401889410196,
-35.9484512081691,-35.8566993998259,-35.7648529967065,-35.6729568925387,
-35.580913522525,-35.5130849684451,-35.4210261316512,-35.3290873616942,
-35.2372422806735,-35.1454615745483,-35.0537141907017,-34.9619764231418,
-34.8702245798533,-34.7783781416357,-34.6864820022339,-34.5944385971196,
-34.5266103859883,-34.4345515609237,-34.3426128028142,-34.2507677337424,
-34.1589870396681,-34.0672396679303,-33.9755019125228,-33.883750081415,
-33.7919036553475,-33.7000075280963,-33.6079641350102,-33.5401358035315,
-33.448076980176,-33.3561382238359,-33.2642931565909,-33.1725124644226,
-33.0807650946389,-32.989027341231,-32.8972755121666,-32.8054290881977,
-32.7135329630789,-32.6214895721594,-32.5536612210747,-32.4616023938271,
-32.369663633532,-32.2778185622746,-32.1860378660245,-32.0942904921179,
-32.0025527345512,-31.9108009012964,-31.8189544731144,-31.7270583437636,
-31.635014948624,-31.5671866386179,-31.4964407967228),.UNSPECIFIED.);
#1337=B_SPLINE_CURVE_WITH_KNOTS('',3,(#10529,#10530,#10531,#10532),
 .UNSPECIFIED.,.F.,.F.,(4,4),(-31.4964407964964,-31.4556278135382),
 .UNSPECIFIED.);
#1338=B_SPLINE_CURVE_WITH_KNOTS('',3,(#10537,#10538,#10539,#10540,#10541,
#10542,#10543,#10544,#10545,#10546,#10547,#10548,#10549,#10550,#10551,#10552,
#10553,#10554,#10555,#10556,#10557,#10558,#10559,#10560,#10561,#10562,#10563,
#10564,#10565,#10566,#10567,#10568,#10569,#10570,#10571,#10572,#10573,#10574,
#10575,#10576,#10577,#10578,#10579,#10580,#10581,#10582,#10583,#10584,#10585,
#10586,#10587,#10588,#10589,#10590,#10591,#10592,#10593,#10594,#10595,#10596,
#10597,#10598,#10599,#10600,#10601,#10602,#10603,#10604,#10605,#10606,#10607,
#10608,#10609,#10610,#10611,#10612,#10613,#10614,#10615,#10616,#10617,#10618,
#10619,#10620,#10621,#10622,#10623,#10624,#10625,#10626,#10627,#10628,#10629,
#10630,#10631,#10632,#10633,#10634,#10635,#10636,#10637,#10638,#10639,#10640,
#10641,#10642,#10643,#10644,#10645,#10646,#10647,#10648,#10649,#10650,#10651,
#10652,#10653,#10654,#10655,#10656,#10657,#10658,#10659,#10660,#10661,#10662,
#10663,#10664,#10665,#10666,#10667,#10668,#10669,#10670,#10671,#10672,#10673,
#10674,#10675,#10676,#10677,#10678,#10679,#10680,#10681,#10682,#10683,#10684,
#10685,#10686,#10687,#10688,#10689,#10690,#10691,#10692,#10693,#10694,#10695,
#10696,#10697,#10698,#10699,#10700,#10701,#10702,#10703,#10704,#10705,#10706,
#10707,#10708),.UNSPECIFIED.,.F.,.F.,(4,2,2,2,2,2,2,2,2,2,2,2,2,2,2,2,2,
2,2,2,2,2,2,2,2,2,2,2,2,2,2,2,2,2,2,2,2,2,2,2,2,2,2,2,2,2,2,2,2,2,2,2,2,
2,2,2,2,2,2,2,2,2,2,2,2,2,2,2,2,2,2,2,2,2,2,2,2,2,2,2,2,2,2,2,2,4),(-2.14953858586417,
-2.13610813898098,-2.10687093381457,-2.0935221044845,-2.0831254479754,-2.07149231131417,
-2.05102003132299,-2.00904126853951,-1.93718251534886,-1.92579729579304,
-1.91931651355889,-1.91321297044488,-1.90366780511875,-1.86670492808403,
-1.78240676041869,-1.76404857092553,-1.75282287879321,-1.74230005870951,
-1.72778442760372,-1.68692585622836,-1.64388492520681,-1.60272463552078,
-1.59094892501349,-1.58438844302371,-1.57833165355395,-1.56903538001366,
-1.53604613636689,-1.48940831177372,-1.44101759357861,-1.4257294457842,
-1.4151857264115,-1.40421607879289,-1.38718524602246,-1.33908552311463,
-1.26676466619605,-1.25545930392889,-1.24899494598056,-1.24288080222962,
-1.23328057998228,-1.19528505603487,-1.10808253925909,-1.09174994054149,
-1.08091235409407,-1.07013932885364,-1.05415624803017,-1.03536586910847,
-0.995752605398778,-0.930612136396024,-0.919842288811208,-0.913489215146185,
-0.907293604969757,-0.897281569532202,-0.846083643004777,-0.774843892541429,
-0.757586723106827,-0.746574089308113,-0.735937662077742,-0.720723346769414,
-0.67056321977808,-0.599313589175422,-0.586315801481275,-0.579511648957109,
-0.573555967702531,-0.564864394134943,-0.538903563574624,-0.484576057882175,
-0.435577041749676,-0.420270860093574,-0.409724031026593,-0.398758819190083,
-0.381751445361605,-0.361316527916232,-0.314989293643927,-0.261991215016622,
-0.25031083845285,-0.243769640704525,-0.237702029212099,-0.228347600828176,
-0.194514321580064,-0.106632668467665,-0.0883038156412996,-0.0770840502604572,
-0.0665590960501105,-0.0561515529498116,-0.0359226655579419,-0.01489375026152),
 .UNSPECIFIED.);
#1339=B_SPLINE_CURVE_WITH_KNOTS('',3,(#10710,#10711,#10712,#10713,#10714,
#10715,#10716,#10717,#10718,#10719,#10720,#10721,#10722,#10723,#10724,#10725,
#10726,#10727,#10728,#10729,#10730,#10731,#10732,#10733,#10734,#10735,#10736,
#10737,#10738,#10739,#10740,#10741,#10742,#10743,#10744,#10745,#10746,#10747,
#10748,#10749,#10750,#10751,#10752,#10753,#10754,#10755,#10756,#10757,#10758,
#10759,#10760,#10761,#10762,#10763,#10764,#10765,#10766,#10767,#10768,#10769,
#10770,#10771,#10772,#10773,#10774,#10775,#10776,#10777,#10778,#10779,#10780,
#10781,#10782,#10783,#10784,#10785,#10786,#10787,#10788,#10789,#10790,#10791,
#10792,#10793,#10794,#10795,#10796,#10797,#10798,#10799,#10800,#10801,#10802,
#10803,#10804,#10805,#10806,#10807,#10808,#10809,#10810,#10811,#10812,#10813,
#10814,#10815,#10816,#10817,#10818,#10819,#10820,#10821,#10822,#10823,#10824,
#10825,#10826,#10827,#10828,#10829,#10830,#10831,#10832,#10833,#10834,#10835,
#10836,#10837,#10838,#10839,#10840,#10841,#10842,#10843,#10844,#10845,#10846,
#10847,#10848,#10849,#10850,#10851,#10852,#10853,#10854,#10855,#10856,#10857,
#10858,#10859,#10860,#10861,#10862,#10863,#10864,#10865,#10866,#10867,#10868,
#10869,#10870,#10871,#10872,#10873,#10874,#10875,#10876,#10877,#10878,#10879,
#10880,#10881,#10882,#10883,#10884,#10885,#10886,#10887,#10888,#10889,#10890,
#10891,#10892,#10893,#10894,#10895,#10896,#10897,#10898,#10899,#10900,#10901,
#10902,#10903,#10904,#10905,#10906,#10907,#10908,#10909,#10910,#10911,#10912,
#10913,#10914,#10915,#10916,#10917,#10918,#10919,#10920),.UNSPECIFIED.,
 .F.,.F.,(4,3,3,3,3,3,3,3,3,3,3,3,3,3,3,3,3,3,3,3,3,3,3,3,3,3,3,3,3,3,3,
3,3,3,3,3,3,3,3,3,3,3,3,3,3,3,3,3,3,3,3,3,3,3,3,3,3,3,3,3,3,3,3,3,3,3,3,
3,3,3,4),(-31.4556278135382,-31.3645591435807,-31.2735913846309,-31.1826963684724,
-31.0918391897302,-31.000995169334,-30.9101396451473,-30.8191934310805,
-30.7281979935595,-30.6370606348414,-30.5807120561611,-30.4886532306627,
-30.3967144721414,-30.3048694026802,-30.2130887082518,-30.121341336182,
-30.0296035804647,-29.9378517490699,-29.8460053227535,-29.7541091952737,
-29.6620658019955,-29.5942374737043,-29.5021786477549,-29.410239888775,
-29.3183948188481,-29.2266141239454,-29.134866751396,-29.0431289951948,
-28.9513771633125,-28.8595307365047,-28.7676346085315,-28.6755912147604,
-28.6077628912475,-28.5157040655444,-28.4237653068137,-28.3319202371385,
-28.2401395424906,-28.1483921701978,-28.0566544142547,-27.9649025826313,
-27.8730561560826,-27.7811600283684,-27.6891166348549,-27.6212883087907,
-27.529229483072,-27.4372907243261,-27.3454456546361,-27.2536649599738,
-27.1619175876671,-27.0701798317099,-26.9784280000733,-26.8865815735122,
-26.7946854457863,-26.7026420522615,-26.6348137263339,-26.5427549005322,
-26.4508161417019,-26.3589710719269,-26.2671903771789,-26.1754430047856,
-26.0837052487418,-25.9919534170181,-25.9001069903698,-25.8082108625567,
-25.7161674689453,-25.6483391438771,-25.5487804941692,-25.4495593335883,
-25.3505537169068,-25.2518618478458,-25.2132554897648),.UNSPECIFIED.);
#1340=B_SPLINE_CURVE_WITH_KNOTS('',3,(#10921,#10922,#10923,#10924),
 .UNSPECIFIED.,.F.,.F.,(4,4),(-25.2132554895433,-25.1729131975202),
 .UNSPECIFIED.);
#1341=B_SPLINE_CURVE_WITH_KNOTS('',3,(#10930,#10931,#10932,#10933,#10934,
#10935,#10936,#10937),.UNSPECIFIED.,.F.,.F.,(4,2,2,4),(-0.0146656910965199,
-0.0136853303791787,-0.00578768816179248,-0.000952400549440762),
 .UNSPECIFIED.);
#1342=B_SPLINE_CURVE_WITH_KNOTS('',3,(#10938,#10939,#10940,#10941,#10942,
#10943,#10944,#10945,#10946,#10947,#10948,#10949,#10950,#10951,#10952,#10953,
#10954,#10955,#10956,#10957,#10958,#10959,#10960,#10961,#10962,#10963,#10964,
#10965,#10966,#10967,#10968,#10969,#10970,#10971,#10972,#10973,#10974,#10975,
#10976,#10977,#10978,#10979,#10980,#10981,#10982,#10983,#10984,#10985,#10986,
#10987,#10988,#10989,#10990,#10991,#10992,#10993,#10994,#10995,#10996,#10997,
#10998,#10999,#11000,#11001,#11002,#11003,#11004,#11005,#11006,#11007,#11008,
#11009,#11010,#11011,#11012,#11013,#11014,#11015,#11016,#11017,#11018,#11019,
#11020,#11021,#11022,#11023,#11024,#11025,#11026,#11027,#11028,#11029,#11030,
#11031,#11032,#11033,#11034,#11035,#11036,#11037,#11038,#11039,#11040,#11041,
#11042,#11043,#11044,#11045,#11046,#11047,#11048,#11049,#11050,#11051,#11052,
#11053,#11054,#11055,#11056,#11057,#11058,#11059,#11060,#11061,#11062,#11063,
#11064,#11065,#11066,#11067,#11068,#11069,#11070,#11071,#11072,#11073,#11074,
#11075,#11076,#11077,#11078,#11079,#11080,#11081,#11082,#11083,#11084,#11085,
#11086,#11087,#11088,#11089,#11090,#11091,#11092,#11093,#11094,#11095,#11096,
#11097,#11098,#11099,#11100,#11101,#11102,#11103,#11104,#11105),
 .UNSPECIFIED.,.F.,.F.,(4,2,2,2,2,2,2,2,2,2,2,2,2,2,2,2,2,2,2,2,2,2,2,2,
2,2,2,2,2,2,2,2,2,2,2,2,2,2,2,2,2,2,2,2,2,2,2,2,2,2,2,2,2,2,2,2,2,2,2,2,
2,2,2,2,2,2,2,2,2,2,2,2,2,2,2,2,2,2,2,2,2,2,2,4),(-4.27070740756644,-4.26845734415281,
-4.26513559133958,-4.25906606303054,-4.24952699657373,-4.21011345994702,
-4.16915985939891,-4.12180760711633,-4.10676704011442,-4.09615910290225,
-4.08509740221113,-4.06758940933802,-3.99910328784442,-3.9458945201856,
-3.93578396964048,-3.9295677886981,-3.9240191638012,-3.91420944433972,-3.87342317107289,
-3.79628390799866,-3.77640623229577,-3.76488647469895,-3.75446318749615,
-3.74089878878225,-3.71027019002783,-3.69362884610084,-3.61789986526809,
-3.60359714260818,-3.59654526967702,-3.59064853248447,-3.58241197101851,
-3.5666807665863,-3.50044895582588,-3.45166143435875,-3.43652726145964,
-3.42590371268601,-3.4161810895516,-3.40005101277712,-3.31189369827086,
-3.27441517997453,-3.26484243659632,-3.25873327803455,-3.25226026131045,
-3.24091380528961,-3.18231134609231,-3.11799245657953,-3.10215500393181,
-3.09140788170318,-3.08053988233276,-3.06404741549002,-2.97767954176669,
-2.9392793607554,-2.92965905691019,-2.92354073671627,-2.91708181879243,
-2.90580370886008,-2.83327143510972,-2.78524170933674,-2.76822013775899,
-2.75725201681171,-2.74670681015199,-2.73141094379886,-2.68269075238979,
-2.63636231039439,-2.60346383850845,-2.5941744648963,-2.58811880042586,
-2.58155582225467,-2.56976801339054,-2.52829661670641,-2.47414699093332,
-2.44211003703892,-2.42859143623981,-2.41820155744132,-2.40653635310401,
-2.38644804475334,-2.30015407711382,-2.26816090375457,-2.25893700769353,
-2.2528930562116,-2.24630694500189,-2.23440577610699,-2.18385852421173,
-2.14953858586417),.UNSPECIFIED.);
#1343=B_SPLINE_CURVE_WITH_KNOTS('',3,(#11107,#11108,#11109,#11110,#11111,
#11112,#11113,#11114,#11115,#11116,#11117,#11118,#11119,#11120,#11121,#11122,
#11123,#11124,#11125,#11126,#11127,#11128,#11129,#11130,#11131,#11132,#11133,
#11134,#11135,#11136,#11137,#11138,#11139,#11140,#11141,#11142,#11143,#11144,
#11145,#11146,#11147,#11148,#11149,#11150,#11151,#11152,#11153,#11154,#11155,
#11156,#11157,#11158,#11159,#11160,#11161,#11162,#11163,#11164,#11165,#11166,
#11167,#11168,#11169,#11170,#11171,#11172,#11173,#11174,#11175,#11176,#11177,
#11178,#11179,#11180,#11181,#11182,#11183,#11184,#11185,#11186,#11187,#11188,
#11189,#11190,#11191,#11192,#11193,#11194,#11195,#11196,#11197,#11198,#11199,
#11200,#11201,#11202,#11203,#11204,#11205,#11206,#11207,#11208,#11209,#11210,
#11211,#11212,#11213,#11214,#11215,#11216,#11217,#11218,#11219,#11220,#11221,
#11222,#11223,#11224,#11225,#11226,#11227,#11228,#11229,#11230,#11231,#11232,
#11233,#11234,#11235,#11236,#11237,#11238,#11239,#11240,#11241,#11242,#11243,
#11244,#11245,#11246,#11247,#11248,#11249,#11250,#11251,#11252,#11253,#11254,
#11255,#11256,#11257,#11258,#11259,#11260,#11261,#11262,#11263,#11264,#11265,
#11266,#11267,#11268,#11269,#11270,#11271,#11272,#11273,#11274,#11275,#11276,
#11277,#11278,#11279,#11280,#11281,#11282,#11283,#11284,#11285,#11286,#11287,
#11288,#11289,#11290,#11291,#11292,#11293,#11294,#11295,#11296,#11297,#11298,
#11299,#11300,#11301,#11302,#11303,#11304,#11305,#11306,#11307,#11308,#11309,
#11310,#11311,#11312,#11313,#11314,#11315,#11316,#11317),.UNSPECIFIED.,
 .F.,.F.,(4,3,3,3,3,3,3,3,3,3,3,3,3,3,3,3,3,3,3,3,3,3,3,3,3,3,3,3,3,3,3,
3,3,3,3,3,3,3,3,3,3,3,3,3,3,3,3,3,3,3,3,3,3,3,3,3,3,3,3,3,3,3,3,3,3,3,3,
3,3,3,4),(-25.1729131975202,-25.0788738378323,-24.9847644203176,-24.8904963173327,
-24.7961392500284,-24.7016048176209,-24.6618645614202,-24.5698057357159,
-24.4778669769843,-24.3860219073086,-24.2942412126603,-24.2024938403674,
-24.1107560844241,-24.0190042528011,-23.9271578262531,-23.8352616985401,
-23.7432183050277,-23.6753899789634,-23.5833311530027,-23.4913923940134,
-23.3995473240798,-23.3077666291737,-23.2160192566231,-23.1242815004226,
-23.032529668543,-22.9406832417416,-22.8487871137763,-22.7567437200162,
-22.6889153965066,-22.5968565710371,-22.5049178125391,-22.413072743095,
-22.3212920486752,-22.2295446766086,-22.1378069208892,-22.046055089487,
-21.9542086631547,-21.8623125356545,-21.7702691423485,-21.7024408140498,
-21.6103819885079,-21.5184432299415,-21.426598160434,-21.3348174659573,
-21.243070093838,-21.1513323380701,-21.0595805066238,-20.9677340802541,
-20.8758379527205,-20.7837945593873,-20.715966231593,-20.6239074042684,
-20.5319686439116,-20.4401235726081,-20.3483428763351,-20.2565955024199,
-20.1648577448588,-20.0731059116239,-19.9812594834839,-19.8893633541873,
-19.7973199591215,-19.7294916491362,-19.6387533739174,-19.5481571350446,
-19.4576413869019,-19.3671810154049,-19.276750966138,-19.1862889103547,
-19.0958131870846,-19.0052388477835,-18.930070182607),.UNSPECIFIED.);
#1344=B_SPLINE_CURVE_WITH_KNOTS('',3,(#11318,#11319,#11320,#11321),
 .UNSPECIFIED.,.F.,.F.,(4,4),(-18.9300701823637,-18.8905536429109),
 .UNSPECIFIED.);
#1345=B_SPLINE_CURVE_WITH_KNOTS('',3,(#11326,#11327,#11328,#11329,#11330,
#11331,#11332,#11333,#11334,#11335,#11336,#11337,#11338,#11339,#11340,#11341,
#11342,#11343,#11344,#11345,#11346,#11347,#11348,#11349,#11350,#11351,#11352,
#11353,#11354,#11355,#11356,#11357,#11358,#11359,#11360,#11361,#11362,#11363,
#11364,#11365,#11366,#11367,#11368,#11369,#11370,#11371,#11372,#11373,#11374,
#11375,#11376,#11377,#11378,#11379,#11380,#11381,#11382,#11383,#11384,#11385,
#11386,#11387,#11388,#11389,#11390,#11391,#11392,#11393,#11394,#11395,#11396,
#11397,#11398,#11399,#11400,#11401,#11402,#11403,#11404,#11405,#11406,#11407,
#11408,#11409,#11410,#11411,#11412,#11413,#11414,#11415,#11416,#11417,#11418,
#11419,#11420,#11421,#11422,#11423,#11424,#11425,#11426,#11427,#11428,#11429,
#11430,#11431,#11432,#11433,#11434,#11435,#11436,#11437,#11438,#11439,#11440,
#11441,#11442,#11443,#11444,#11445,#11446,#11447,#11448,#11449,#11450,#11451,
#11452,#11453,#11454,#11455,#11456,#11457,#11458,#11459,#11460,#11461,#11462,
#11463,#11464,#11465,#11466,#11467,#11468,#11469,#11470,#11471,#11472,#11473,
#11474,#11475,#11476,#11477,#11478,#11479,#11480,#11481,#11482,#11483,#11484,
#11485),.UNSPECIFIED.,.F.,.F.,(4,2,2,2,2,2,2,2,2,2,2,2,2,2,2,2,2,2,2,2,
2,2,2,2,2,2,2,2,2,2,2,2,2,2,2,2,2,2,2,2,2,2,2,2,2,2,2,2,2,2,2,2,2,2,2,2,
2,2,2,2,2,2,2,2,2,2,2,2,2,2,2,2,2,2,2,2,2,2,2,4),(-2.14929610429856,-2.13546420060753,
-2.05952257959691,-2.02135630128187,-2.01163747150297,-2.00610532855159,
-1.99986862416345,-1.98965703996022,-1.93689921034541,-1.86805261034334,
-1.85056925677954,-1.83951280409052,-1.82890296846166,-1.81384752281798,
-1.76624363582999,-1.70408844889312,-1.68313484161148,-1.67484391041751,
-1.66894143595695,-1.6619238153601,-1.64780429759842,-1.57828901672924,
-1.5283911789661,-1.51306292788187,-1.50251304115817,-1.49155461978892,
-1.47457925945926,-1.41954608868631,-1.35272459954898,-1.34215288669531,
-1.33584132096922,-1.32961008093004,-1.31942331018782,-1.30672559706725,
-1.27796607365477,-1.19950440879412,-1.18112791310739,-1.16989924299949,
-1.15937887655559,-1.14487520442654,-1.10413562971075,-1.06124090532109,
-1.01981336371654,-1.00802996324934,-1.00146822761214,-0.995412816490563,
-0.986122322518482,-0.953207721022963,-0.906835969948993,-0.858125564142618,
-0.84282877879844,-0.832284183874897,-0.821317806699372,-0.804301090105841,
-0.756295628946055,-0.683810467133665,-0.672535405490896,-0.666077605267117,
-0.659959925147,-0.650339754463948,-0.611939939149989,-0.525525154332974,
-0.509036470323033,-0.498170260114691,-0.487424478073313,-0.471588035855322,
-0.40707434501598,-0.348776340856676,-0.337419925706362,-0.330945468836147,
-0.324838891291911,-0.315275743896004,-0.277969583990255,-0.191934540819767,
-0.174670707009472,-0.163657356711335,-0.153022693458767,-0.137815258590444,
-0.0877584016624937,-0.0146656910965199),.UNSPECIFIED.);
#1346=B_SPLINE_CURVE_WITH_KNOTS('',3,(#11487,#11488,#11489,#11490,#11491,
#11492,#11493,#11494,#11495,#11496,#11497,#11498,#11499,#11500,#11501,#11502,
#11503,#11504,#11505,#11506,#11507,#11508,#11509,#11510,#11511,#11512,#11513,
#11514,#11515,#11516,#11517,#11518,#11519,#11520,#11521,#11522,#11523,#11524,
#11525,#11526,#11527,#11528,#11529,#11530,#11531,#11532,#11533,#11534,#11535,
#11536,#11537,#11538,#11539,#11540,#11541,#11542,#11543,#11544,#11545,#11546,
#11547,#11548,#11549,#11550,#11551,#11552,#11553,#11554,#11555,#11556,#11557,
#11558,#11559,#11560,#11561,#11562,#11563,#11564,#11565,#11566,#11567,#11568,
#11569,#11570,#11571,#11572,#11573,#11574,#11575,#11576,#11577,#11578,#11579,
#11580,#11581,#11582,#11583,#11584,#11585,#11586,#11587,#11588,#11589,#11590,
#11591,#11592,#11593,#11594,#11595,#11596,#11597,#11598,#11599,#11600,#11601,
#11602,#11603,#11604,#11605,#11606,#11607,#11608,#11609,#11610,#11611,#11612,
#11613,#11614,#11615,#11616,#11617,#11618,#11619,#11620,#11621,#11622,#11623,
#11624,#11625,#11626,#11627,#11628,#11629,#11630,#11631,#11632,#11633,#11634,
#11635,#11636,#11637,#11638,#11639,#11640,#11641,#11642,#11643,#11644,#11645,
#11646,#11647,#11648,#11649,#11650,#11651,#11652,#11653,#11654,#11655,#11656,
#11657,#11658,#11659,#11660,#11661,#11662,#11663,#11664,#11665,#11666,#11667,
#11668,#11669,#11670,#11671,#11672,#11673,#11674,#11675,#11676,#11677,#11678,
#11679,#11680,#11681,#11682,#11683,#11684,#11685,#11686,#11687,#11688,#11689,
#11690,#11691,#11692,#11693,#11694,#11695,#11696,#11697),.UNSPECIFIED.,
 .F.,.F.,(4,3,3,3,3,3,3,3,3,3,3,3,3,3,3,3,3,3,3,3,3,3,3,3,3,3,3,3,3,3,3,
3,3,3,3,3,3,3,3,3,3,3,3,3,3,3,3,3,3,3,3,3,3,3,3,3,3,3,3,3,3,3,3,3,3,3,3,
3,3,3,4),(-18.8905536429109,-18.7557293146775,-18.7430170666794,-18.6509582413954,
-18.5590194831107,-18.4671744139074,-18.375393719768,-18.2836463480059,
-18.1919085926147,-18.1001567615639,-18.008310335616,-17.9164142085194,
-17.8243708156434,-17.7565424842226,-17.6644836469602,-17.5725448766289,
-17.4806997953276,-17.3889190890633,-17.2971717051645,-17.2054339376393,
-17.1136820944725,-17.0218356565102,-16.9299395174383,-16.8378961127723,
-16.7700679017658,-16.6780090994978,-16.5860703641842,-16.4942253178778,
-16.4024446464311,-16.3106972972283,-16.2189595642365,-16.1272077553988,
-16.0353613512415,-15.9434652457323,-15.8514218738956,-15.783593319309,
-15.6915344876934,-15.5995957232524,-15.5077506480737,-15.4159699482515,
-15.3242225709882,-15.2324848102825,-15.1407329741097,-15.0488865433661,
-14.9569904116482,-14.8649470144796,-14.7971187368521,-14.705059830534,
-14.6131209908129,-14.5212758398835,-14.4294950639227,-14.3377476103115,
-14.2460097731428,-14.1542578604853,-14.0624113536955,-13.970515146065,
-13.8784716739733,-13.8106441543953,-13.7185855293363,-13.6266469712689,
-13.5348021020134,-13.443021606603,-13.3512744327491,-13.2595368742113,
-13.1677852387247,-13.0759390051598,-12.984043068957,-12.8919998626249,
-12.8241695719385,-12.6868365123048,-12.6468848751841),.UNSPECIFIED.);
#1347=B_SPLINE_CURVE_WITH_KNOTS('',3,(#11698,#11699,#11700,#11701),
 .UNSPECIFIED.,.F.,.F.,(4,4),(-12.646880067867,-12.605793069694),
 .UNSPECIFIED.);
#1348=B_SPLINE_CURVE_WITH_KNOTS('',3,(#11707,#11708,#11709,#11710),
 .UNSPECIFIED.,.F.,.F.,(4,4),(-0.0143336373215858,-0.000956395227510613),
 .UNSPECIFIED.);
#1349=B_SPLINE_CURVE_WITH_KNOTS('',3,(#11711,#11712,#11713,#11714,#11715,
#11716,#11717,#11718,#11719,#11720,#11721,#11722,#11723,#11724,#11725,#11726,
#11727,#11728,#11729,#11730,#11731,#11732,#11733,#11734,#11735,#11736,#11737,
#11738,#11739,#11740,#11741,#11742,#11743,#11744,#11745,#11746,#11747,#11748,
#11749,#11750,#11751,#11752,#11753,#11754,#11755,#11756,#11757,#11758,#11759,
#11760,#11761,#11762,#11763,#11764,#11765,#11766,#11767,#11768,#11769,#11770,
#11771,#11772,#11773,#11774,#11775,#11776,#11777,#11778,#11779,#11780,#11781,
#11782,#11783,#11784,#11785,#11786,#11787,#11788,#11789,#11790,#11791,#11792,
#11793,#11794,#11795,#11796,#11797,#11798,#11799,#11800,#11801,#11802,#11803,
#11804,#11805,#11806,#11807,#11808,#11809,#11810,#11811,#11812,#11813,#11814,
#11815,#11816,#11817,#11818,#11819,#11820,#11821,#11822,#11823,#11824,#11825,
#11826,#11827,#11828,#11829,#11830,#11831,#11832,#11833,#11834,#11835,#11836,
#11837,#11838,#11839,#11840,#11841,#11842,#11843,#11844,#11845,#11846,#11847,
#11848,#11849,#11850,#11851,#11852,#11853,#11854,#11855,#11856,#11857,#11858,
#11859,#11860,#11861,#11862,#11863,#11864,#11865,#11866,#11867,#11868,#11869,
#11870,#11871,#11872,#11873,#11874,#11875,#11876),.UNSPECIFIED.,.F.,.F.,
(4,2,2,2,2,2,2,2,2,2,2,2,2,2,2,2,2,2,2,2,2,2,2,2,2,2,2,2,2,2,2,2,2,2,2,
2,2,2,2,2,2,2,2,2,2,2,2,2,2,2,2,2,2,2,2,2,2,2,2,2,2,2,2,2,2,2,2,2,2,2,2,
2,2,2,2,2,2,2,2,2,2,2,4),(-4.27075566588217,-4.22829678691838,-4.20716660973916,
-4.19293595591049,-4.18245536031667,-4.17112333488929,-4.15221716328105,
-4.06868544790909,-4.03199788215742,-4.02246865308842,-4.0163680373765,
-4.00988188810468,-3.99847231363553,-3.92669569261786,-3.87825848541359,
-3.8611788431039,-3.8501991667344,-3.83966060812061,-3.82440676220799,-3.77698114903899,
-3.72959533825348,-3.69640951053994,-3.68709961168663,-3.68103990998908,
-3.67448343916799,-3.66272817673599,-3.59300078740973,-3.53954516752815,
-3.52415797255716,-3.51349170215524,-3.50252321294966,-3.48549619727635,
-3.40186688966681,-3.37473034606797,-3.357250251695,-3.34965453134102,-3.3437982546825,
-3.33624589446818,-3.31970212565846,-3.25279360715997,-3.20381711487164,
-3.18867215516095,-3.17804747178415,-3.16701625163083,-3.14966237173264,
-3.06775066371959,-3.03995088258877,-3.02219342779498,-3.01455398168473,
-3.00869716189578,-3.00118673040566,-2.98423878097789,-2.91755043422619,
-2.86863582116899,-2.85349447367274,-2.84287021075578,-2.83183763790963,
-2.81447766485955,-2.73259719480224,-2.6917318137603,-2.68199898243569,
-2.67585903222826,-2.66943293761237,-2.65831194878752,-2.59624265451598,
-2.53553574898416,-2.51945125413548,-2.50865972422484,-2.49784196283243,
-2.48161523124333,-2.39394462718287,-2.35622582513403,-2.34664103482908,
-2.34052992366097,-2.33406129785287,-2.32273445645158,-2.26364092558707,
-2.22082481112579,-2.19268930029812,-2.17973084959801,-2.16938969329131,
-2.15736609801839,-2.14929610429856),.UNSPECIFIED.);
#1350=B_SPLINE_CURVE_WITH_KNOTS('',3,(#11878,#11879,#11880,#11881,#11882,
#11883,#11884,#11885,#11886,#11887),.UNSPECIFIED.,.F.,.F.,(4,1,1,1,1,1,
1,4),(-12.605793069694,-11.8376949894817,-10.8512204070249,-9.86474582456809,
-8.87827124211129,-7.89179665965447,-6.90532207719767,-6.36369956800449),
 .UNSPECIFIED.);
#1351=B_SPLINE_CURVE_WITH_KNOTS('',3,(#11888,#11889,#11890,#11891),
 .UNSPECIFIED.,.F.,.F.,(4,4),(-6.36369956800449,-6.32388523350727),
 .UNSPECIFIED.);
#1352=B_SPLINE_CURVE_WITH_KNOTS('',3,(#11900,#11901,#11902,#11903,#11904,
#11905,#11906,#11907,#11908,#11909,#11910,#11911,#11912,#11913,#11914,#11915,
#11916,#11917,#11918,#11919,#11920,#11921,#11922,#11923,#11924,#11925,#11926,
#11927,#11928,#11929,#11930,#11931,#11932,#11933,#11934,#11935,#11936,#11937,
#11938,#11939,#11940,#11941),.UNSPECIFIED.,.F.,.F.,(4,2,2,2,2,2,2,2,2,2,
2,2,2,2,2,2,2,2,2,2,4),(-2.74875994684861,-2.73680062346907,-2.66994582987793,
-2.61858205907705,-2.6031629846185,-2.59238489636777,-2.58254038544452,
-2.56622343375549,-2.49014672046941,-2.4448468966665,-2.43487891586894,
-2.42860085479822,-2.42208310613659,-2.41069541006536,-2.35241981652588,
-2.28811087525863,-2.27228734435194,-2.26150416905709,-2.25055972640412,
-2.23386405000636,-2.14915318645226),.UNSPECIFIED.);
#1353=B_SPLINE_CURVE_WITH_KNOTS('',3,(#11945,#11946,#11947,#11948,#11949,
#11950,#11951,#11952),.UNSPECIFIED.,.F.,.F.,(4,2,2,4),(-0.0136766484190329,
-0.0136650905131395,-0.00597929307771191,0.),.UNSPECIFIED.);
#1354=B_SPLINE_CURVE_WITH_KNOTS('',3,(#11955,#11956,#11957,#11958,#11959,
#11960,#11961,#11962,#11963,#11964,#11965,#11966,#11967,#11968,#11969,#11970,
#11971,#11972,#11973,#11974,#11975,#11976,#11977,#11978,#11979,#11980,#11981,
#11982,#11983,#11984,#11985,#11986,#11987,#11988,#11989,#11990,#11991,#11992,
#11993,#11994,#11995,#11996,#11997,#11998,#11999,#12000,#12001,#12002,#12003,
#12004,#12005,#12006,#12007,#12008,#12009,#12010,#12011,#12012,#12013,#12014,
#12015,#12016,#12017,#12018,#12019,#12020,#12021,#12022,#12023,#12024,#12025,
#12026,#12027,#12028,#12029,#12030,#12031,#12032,#12033,#12034,#12035,#12036,
#12037,#12038,#12039,#12040,#12041,#12042,#12043,#12044,#12045,#12046,#12047,
#12048,#12049,#12050,#12051,#12052,#12053,#12054,#12055,#12056,#12057,#12058,
#12059,#12060,#12061,#12062,#12063,#12064,#12065,#12066,#12067,#12068,#12069,
#12070,#12071,#12072,#12073,#12074,#12075,#12076,#12077,#12078,#12079,#12080,
#12081,#12082,#12083,#12084,#12085,#12086,#12087,#12088,#12089,#12090,#12091,
#12092,#12093,#12094,#12095,#12096,#12097,#12098,#12099,#12100,#12101,#12102,
#12103,#12104,#12105,#12106,#12107,#12108,#12109,#12110,#12111,#12112,#12113,
#12114,#12115,#12116,#12117,#12118,#12119,#12120,#12121,#12122,#12123,#12124,
#12125,#12126,#12127,#12128,#12129,#12130),.UNSPECIFIED.,.F.,.F.,(4,2,2,
2,2,2,2,2,2,2,2,2,2,2,2,2,2,2,2,2,2,2,2,2,2,2,2,2,2,2,2,2,2,2,2,2,2,2,2,
2,2,2,2,2,2,2,2,2,2,2,2,2,2,2,2,2,2,2,2,2,2,2,2,2,2,2,2,2,2,2,2,2,2,2,2,
2,2,2,2,2,2,2,2,2,2,2,2,4),(-2.14915318645226,-2.13977645196419,-2.1080230085618,
-2.09880088562358,-2.09275325065881,-2.08619301461964,-2.07432944046408,
-2.0300292253873,-1.98844183527612,-1.94900613152566,-1.93467381877651,
-1.92422632513365,-1.91303383787223,-1.89463127284146,-1.81011878904744,
-1.77302312501884,-1.7635031006812,-1.75742728330176,-1.75096223581443,
-1.73966073299329,-1.67978569541584,-1.61701600790134,-1.60094705824663,
-1.59014195292663,-1.57929034828942,-1.56296779956946,-1.48469862007157,
-1.44235556857053,-1.43053416799353,-1.42395101506027,-1.41795441653693,
-1.40870095239954,-1.37865652758475,-1.3747320458654,-1.28308794063715,
-1.2666199265708,-1.25575343244952,-1.24499674298735,-1.22912387208739,
-1.21051175727462,-1.17159093799611,-1.10488623403885,-1.09429026306603,
-1.0879733151939,-1.08175019409971,-1.0715936047182,-1.01834666410771,-0.949943627903787,
-0.932427970779454,-0.921370136937541,-0.910772556920358,-0.895759187861899,
-0.848708020265131,-0.806917382321201,-0.768059114382065,-0.75831517249119,
-0.752781020769279,-0.746551879382092,-0.736378438319912,-0.723703588450711,
-0.69503427209062,-0.616952807509691,-0.598284433783136,-0.586996233807493,
-0.576494503724389,-0.562136071312497,-0.522918651835135,-0.48100459936932,
-0.436903944879415,-0.425031998285458,-0.418450138009205,-0.412401545987218,
-0.403155310551825,-0.370872617388443,-0.284506134251647,-0.26461898844124,
-0.252994408223817,-0.242596629471047,-0.229004035373909,-0.196403462788172,
-0.140328709106667,-0.0979915958228728,-0.0881577625901853,-0.0826054945296962,
-0.0763967162790068,-0.066317535538703,-0.0537979154367359,-0.0143336373215858),
 .UNSPECIFIED.);
#1355=B_SPLINE_CURVE_WITH_KNOTS('',3,(#12132,#12133,#12134,#12135,#12136,
#12137,#12138,#12139,#12140,#12141,#12142,#12143,#12144,#12145,#12146,#12147,
#12148,#12149,#12150,#12151,#12152,#12153,#12154,#12155,#12156,#12157,#12158,
#12159,#12160,#12161,#12162,#12163,#12164,#12165,#12166,#12167,#12168,#12169,
#12170,#12171,#12172,#12173,#12174,#12175,#12176,#12177,#12178,#12179,#12180,
#12181,#12182,#12183,#12184,#12185,#12186,#12187,#12188,#12189,#12190,#12191,
#12192,#12193,#12194,#12195,#12196,#12197,#12198,#12199,#12200,#12201,#12202,
#12203,#12204,#12205,#12206,#12207,#12208,#12209,#12210,#12211,#12212,#12213,
#12214,#12215,#12216,#12217,#12218,#12219,#12220,#12221,#12222,#12223,#12224,
#12225,#12226,#12227,#12228,#12229,#12230,#12231,#12232,#12233,#12234,#12235,
#12236,#12237,#12238,#12239,#12240,#12241,#12242,#12243,#12244,#12245,#12246,
#12247,#12248,#12249,#12250,#12251,#12252,#12253,#12254,#12255,#12256,#12257,
#12258,#12259,#12260,#12261,#12262,#12263,#12264,#12265,#12266,#12267,#12268,
#12269,#12270,#12271,#12272,#12273,#12274,#12275,#12276,#12277,#12278,#12279,
#12280,#12281,#12282,#12283,#12284,#12285,#12286,#12287,#12288,#12289,#12290,
#12291,#12292,#12293,#12294,#12295,#12296,#12297,#12298,#12299,#12300,#12301,
#12302,#12303,#12304,#12305,#12306,#12307,#12308,#12309,#12310,#12311,#12312,
#12313,#12314,#12315,#12316,#12317,#12318,#12319,#12320,#12321,#12322,#12323,
#12324,#12325,#12326,#12327,#12328,#12329,#12330,#12331,#12332,#12333,#12334,
#12335,#12336,#12337,#12338,#12339),.UNSPECIFIED.,.F.,.F.,(4,3,3,3,3,3,
3,3,3,3,3,3,3,3,3,3,3,3,3,3,3,3,3,3,3,3,3,3,3,3,3,3,3,3,3,3,3,3,3,3,3,3,
3,3,3,3,3,3,3,3,3,3,3,3,3,3,3,3,3,3,3,3,3,3,3,3,3,3,3,4),(-6.32388523350727,
-6.22262579881566,-6.12405219125192,-6.02144984299638,-5.91884749474085,
-5.82677170021766,-5.73481575008188,-5.64295329224136,-5.55115498883091,
-5.45938987934615,-5.36763428019483,-5.27586452167952,-5.18400015070594,
-5.09208604288732,-5.00002479493562,-4.93237291228405,-4.84041538501824,
-4.74857815709913,-4.65683471651366,-4.56515538493322,-4.47350917728831,
-4.38187226863628,-4.29022084773689,-4.19847354646315,-4.10667597603899,
-4.01472921555433,-3.94589832982724,-3.85368314282726,-3.76158838577229,
-3.66958788472042,-3.57765324610522,-3.48575290461766,-3.39386333766725,
-3.30196103757621,-3.20996713085427,-3.11792497754333,-3.02573938568974,
-2.95942374737043,-2.86729445288601,-2.77528351990613,-2.68336469320923,
-2.59150820388178,-2.49968381936634,-2.40786793835657,-2.3160369726511,
-2.22411036274905,-2.13213335341171,-2.04000878182278,-1.97294916491362,
-1.88173600258,-1.79064323262133,-1.69964346841178,-1.60870377166317,-1.51779459789241,
-1.42689135047595,-1.33596944318732,-1.24494083397421,-1.15385717271455,
-1.06260900446962,-0.986474582456811,-0.892933128223043,-0.799526737551554,
-0.706253524008857,-0.613057275991345,-0.519916434825251,-0.426809493840829,
-0.333687967356518,-0.240561825277099,-0.14736608189716,-0.0805142608249079),
 .UNSPECIFIED.);
#1356=B_SPLINE_CURVE_WITH_KNOTS('',3,(#12340,#12341,#12342,#12343),
 .UNSPECIFIED.,.F.,.F.,(4,4),(-0.0273304800634966,-0.0136766484190329),
 .UNSPECIFIED.);
#1357=B_SPLINE_CURVE_WITH_KNOTS('',3,(#12346,#12347,#12348,#12349,#12350,
#12351,#12352,#12353,#12354,#12355,#12356,#12357,#12358,#12359,#12360,#12361,
#12362,#12363,#12364,#12365,#12366,#12367,#12368,#12369,#12370,#12371,#12372,
#12373,#12374,#12375,#12376,#12377,#12378,#12379,#12380,#12381,#12382,#12383,
#12384,#12385,#12386,#12387,#12388,#12389,#12390,#12391,#12392,#12393,#12394,
#12395,#12396,#12397,#12398,#12399,#12400,#12401,#12402,#12403,#12404,#12405,
#12406,#12407,#12408,#12409,#12410,#12411,#12412,#12413,#12414,#12415,#12416,
#12417,#12418,#12419,#12420,#12421,#12422,#12423,#12424,#12425,#12426,#12427,
#12428,#12429,#12430,#12431,#12432,#12433,#12434,#12435,#12436,#12437,#12438,
#12439,#12440,#12441,#12442,#12443,#12444,#12445,#12446,#12447,#12448,#12449,
#12450,#12451,#12452,#12453,#12454,#12455,#12456,#12457,#12458,#12459,#12460,
#12461,#12462,#12463,#12464,#12465,#12466,#12467,#12468,#12469,#12470,#12471,
#12472,#12473,#12474,#12475,#12476,#12477,#12478,#12479,#12480,#12481,#12482,
#12483,#12484,#12485,#12486,#12487,#12488,#12489,#12490,#12491,#12492,#12493,
#12494,#12495,#12496,#12497,#12498,#12499,#12500,#12501,#12502,#12503,#12504,
#12505,#12506,#12507,#12508,#12509,#12510,#12511,#12512,#12513,#12514,#12515,
#12516,#12517,#12518,#12519,#12520,#12521,#12522,#12523,#12524,#12525,#12526,
#12527,#12528,#12529,#12530,#12531,#12532,#12533,#12534,#12535,#12536,#12537,
#12538,#12539,#12540,#12541),.UNSPECIFIED.,.F.,.F.,(4,3,3,3,3,3,3,3,3,3,
3,3,3,3,3,3,3,3,3,3,3,3,3,3,3,3,3,3,3,3,3,3,3,3,3,3,3,3,3,3,3,3,3,3,3,3,
3,3,3,3,3,3,3,3,3,3,3,3,3,3,3,3,3,3,3,4),(22.9601178369312,23.0476632051047,
23.135213307798,23.2227887574945,23.3104589160482,23.3981838672193,23.4860359984705,
23.5192456667785,23.6071124398246,23.6948693164178,23.7825392284102,23.8729368560134,
23.960509806113,24.0480702283888,24.1356387186068,24.2232358732018,24.3109292666562,
24.3986804063943,24.4865549881911,24.5057202492353,24.5935851740784,24.6813402090151,
24.769008288204,24.85940660614,24.9469777578932,25.0345363979054,25.1221031240315,
25.209698534809,25.2973902233545,25.3851396790604,25.4730126198469,25.4921948316921,
25.5800570260922,25.6678092807244,25.7554745334751,25.8458738935593,25.9334421221125,
26.0209978081109,26.1085615525769,26.1961539571956,26.2838426182611,26.3715890305608,
26.4594589274378,26.4786694141489,26.5665335826018,26.6542878372078,26.7419551132146,
26.8323537236385,26.9199240202891,27.0074817873822,27.0950476236647,27.1826421285534,
27.2703328919068,27.3580814100585,27.4459534022615,27.4651439966058,27.5517327508406,
27.6420578922587,27.7284382334182,27.8147667965675,27.9010653768991,27.9873557389373,
28.073693063983,28.160058275786,28.2465113806051,28.2743338821854),
 .UNSPECIFIED.);
#1358=B_SPLINE_CURVE_WITH_KNOTS('',3,(#12542,#12543,#12544,#12545,#12546,
#12547,#12548,#12549,#12550,#12551,#12552,#12553,#12554,#12555,#12556,#12557,
#12558,#12559,#12560,#12561,#12562,#12563,#12564,#12565,#12566,#12567,#12568,
#12569,#12570,#12571,#12572,#12573,#12574,#12575),.UNSPECIFIED.,.F.,.F.,
(4,3,3,3,3,3,3,3,3,3,3,4),(28.2743338823081,28.4054086201873,28.4516185790626,
28.5394941256643,28.6273758957033,28.7150344267578,28.8026345706311,28.8901969753923,
28.9782848030383,29.0658567392794,29.1542025126278,29.2425482859762),
 .UNSPECIFIED.);
#1359=B_SPLINE_CURVE_WITH_KNOTS('',3,(#12577,#12578,#12579,#12580,#12581,
#12582,#12583,#12584,#12585,#12586,#12587,#12588,#12589,#12590,#12591,#12592,
#12593,#12594,#12595,#12596,#12597,#12598,#12599,#12600,#12601,#12602,#12603,
#12604,#12605,#12606,#12607,#12608,#12609,#12610,#12611,#12612,#12613),
 .UNSPECIFIED.,.F.,.F.,(4,3,3,3,3,3,3,3,3,3,3,3,4),(28.2743338823081,28.3609594265871,
28.4475299266133,28.5340726431711,28.6206091569836,28.7071610397518,28.7938001360196,
28.8804868583994,28.9673043233213,29.0202572380501,29.1081269068421,29.1958739894493,
29.243664967692),.UNSPECIFIED.);
#1360=B_SPLINE_CURVE_WITH_KNOTS('',3,(#12614,#12615,#12616,#12617,#12618,
#12619,#12620,#12621,#12622,#12623,#12624,#12625,#12626,#12627,#12628,#12629,
#12630,#12631,#12632,#12633,#12634,#12635,#12636,#12637,#12638,#12639,#12640,
#12641,#12642,#12643,#12644,#12645,#12646,#12647,#12648,#12649,#12650,#12651,
#12652,#12653,#12654,#12655,#12656,#12657,#12658,#12659,#12660,#12661,#12662,
#12663,#12664,#12665,#12666,#12667,#12668,#12669,#12670,#12671,#12672,#12673,
#12674,#12675,#12676,#12677,#12678,#12679,#12680,#12681,#12682,#12683,#12684,
#12685,#12686,#12687,#12688,#12689,#12690,#12691,#12692,#12693,#12694,#12695,
#12696,#12697,#12698,#12699,#12700,#12701,#12702,#12703,#12704,#12705,#12706,
#12707,#12708,#12709,#12710,#12711,#12712,#12713,#12714,#12715,#12716,#12717,
#12718,#12719,#12720,#12721,#12722,#12723,#12724,#12725,#12726,#12727,#12728,
#12729,#12730,#12731,#12732,#12733,#12734,#12735,#12736,#12737,#12738,#12739,
#12740,#12741,#12742,#12743,#12744,#12745,#12746,#12747,#12748,#12749,#12750,
#12751,#12752,#12753,#12754,#12755,#12756,#12757,#12758,#12759,#12760,#12761,
#12762,#12763,#12764,#12765,#12766,#12767,#12768,#12769,#12770,#12771,#12772,
#12773,#12774,#12775,#12776,#12777,#12778,#12779,#12780,#12781,#12782,#12783,
#12784,#12785,#12786,#12787,#12788,#12789,#12790,#12791,#12792,#12793,#12794,
#12795,#12796,#12797,#12798,#12799,#12800,#12801,#12802,#12803,#12804,#12805,
#12806,#12807,#12808,#12809),.UNSPECIFIED.,.F.,.F.,(4,3,3,3,3,3,3,3,3,3,
3,3,3,3,3,3,3,3,3,3,3,3,3,3,3,3,3,3,3,3,3,3,3,3,3,3,3,3,3,3,3,3,3,3,3,3,
3,3,3,3,3,3,3,3,3,3,3,3,3,3,3,3,3,3,3,4),(22.959407626261,23.0471667563207,
23.1014097433092,23.1892903176247,23.2770610256841,23.364744781634,23.4551372246505,
23.5427239571801,23.6302981140569,23.7178802752913,23.8054910215075,23.8931978201871,
23.9809622710052,24.0688499272475,24.087884325766,24.1757616745349,24.2635293741877,
24.3512103418007,24.4416039126035,24.5291884271683,24.6167605827559,24.7043409627459,
24.7919501512936,24.8796557325264,24.9674191639839,25.0553060972717,25.0743589082228,
25.1622107786669,25.2499525693141,25.3376072318518,25.4280105142053,25.5155679067148,
25.6031126844816,25.6906654604034,25.7782468480054,25.865924475284,25.9536598314417,
26.0415187221286,26.0608334906796,26.148700249896,26.2364571125248,26.3241270104362,
26.4145246432738,26.502097579093,26.5896579870398,26.677226462896,26.7648236031118,
26.8525169822334,26.9402681076499,27.0281426752476,27.0473080731364,27.1351729963301,
27.2229280295589,27.3105961069842,27.4009944255604,27.4885655754207,27.5761242134951,
27.6636909376404,27.7512863463961,27.8389780328687,27.9267274864697,28.0146004251197,
28.0337826555933,28.1540582688503,28.2667246132152,28.2743338821073),
 .UNSPECIFIED.);
#1361=B_SPLINE_CURVE_WITH_KNOTS('',3,(#13034,#13035,#13036,#13037,#13038,
#13039,#13040,#13041,#13042,#13043,#13044,#13045,#13046,#13047,#13048,#13049,
#13050,#13051,#13052,#13053,#13054,#13055,#13056,#13057,#13058,#13059,#13060,
#13061,#13062,#13063,#13064,#13065,#13066,#13067,#13068,#13069,#13070,#13071,
#13072,#13073,#13074,#13075,#13076,#13077,#13078,#13079,#13080,#13081,#13082,
#13083,#13084,#13085,#13086,#13087,#13088,#13089,#13090,#13091,#13092,#13093,
#13094,#13095,#13096,#13097,#13098,#13099,#13100,#13101,#13102,#13103,#13104,
#13105,#13106,#13107,#13108,#13109,#13110,#13111,#13112,#13113,#13114,#13115,
#13116,#13117,#13118,#13119,#13120,#13121,#13122,#13123,#13124,#13125,#13126,
#13127,#13128,#13129,#13130),.UNSPECIFIED.,.F.,.F.,(4,3,3,3,3,3,3,3,3,3,
3,3,3,3,3,3,3,3,3,3,3,3,3,3,3,3,3,3,3,3,3,3,4),(0.,0.0371569355328809,0.0748591992606652,
0.112711498711869,0.148235810103463,0.156456024208327,0.161411147228472,
0.198370337527692,0.235138786797284,0.271056856315181,0.300871782327052,
0.307500754227861,0.312797824867268,0.348043230867719,0.383122091970086,
0.389313331030337,0.425334470814702,0.445315771807008,0.452555104475577,
0.457494349157134,0.49247276846388,0.52759487306579,0.562163035780557,0.595118177172423,
0.600660474525191,0.634670637653703,0.658985440093948,0.671142841314071,
0.679282696844516,0.683300242534193,0.715784112958499,0.74542767605421,
0.760759816994557),.UNSPECIFIED.);
#1362=B_SPLINE_CURVE_WITH_KNOTS('',3,(#13131,#13132,#13133,#13134,#13135,
#13136,#13137,#13138,#13139,#13140,#13141,#13142,#13143,#13144,#13145,#13146,
#13147,#13148,#13149,#13150,#13151,#13152,#13153,#13154,#13155,#13156,#13157,
#13158,#13159,#13160,#13161,#13162,#13163,#13164,#13165,#13166,#13167,#13168,
#13169,#13170,#13171,#13172,#13173,#13174,#13175,#13176,#13177,#13178,#13179,
#13180,#13181,#13182,#13183,#13184,#13185,#13186,#13187,#13188,#13189,#13190,
#13191,#13192,#13193,#13194,#13195,#13196,#13197,#13198,#13199,#13200,#13201,
#13202,#13203,#13204,#13205,#13206,#13207,#13208,#13209,#13210,#13211,#13212,
#13213,#13214,#13215,#13216,#13217,#13218,#13219,#13220,#13221),
 .UNSPECIFIED.,.F.,.F.,(4,3,3,3,3,3,3,3,3,3,3,3,3,3,3,3,3,3,3,3,3,3,3,3,
3,3,3,3,3,3,4),(-0.760759816994501,-0.728670005673473,-0.695695580357834,
-0.67904040478989,-0.673088551585097,-0.639573529909649,-0.605410590976213,
-0.599940992372035,-0.594530569322622,-0.55976930285687,-0.524694383676994,
-0.489867297069393,-0.455524569347743,-0.450701654934437,-0.41471168722101,
-0.406206270916632,-0.371647791277057,-0.336193695752684,-0.316381579222496,
-0.308862022274732,-0.30308148718843,-0.267013208605779,-0.230365762573195,
-0.19336779526563,-0.16051946557862,-0.152997977663309,-0.115126875727451,
-0.0772143395199071,-0.0399904833125805,-0.018319237973236,-7.36539879652355E-5),
 .UNSPECIFIED.);
#1363=B_SPLINE_CURVE_WITH_KNOTS('',3,(#13223,#13224,#13225,#13226,#13227,
#13228,#13229,#13230,#13231,#13232,#13233,#13234,#13235,#13236,#13237,#13238,
#13239,#13240,#13241,#13242,#13243,#13244,#13245,#13246,#13247,#13248,#13249,
#13250,#13251,#13252,#13253,#13254,#13255,#13256,#13257,#13258,#13259,#13260,
#13261,#13262,#13263,#13264,#13265,#13266,#13267,#13268,#13269,#13270,#13271,
#13272,#13273,#13274,#13275,#13276,#13277,#13278,#13279,#13280,#13281,#13282,
#13283,#13284,#13285,#13286,#13287,#13288,#13289,#13290,#13291,#13292,#13293,
#13294,#13295,#13296,#13297,#13298,#13299,#13300,#13301,#13302,#13303,#13304,
#13305,#13306,#13307,#13308,#13309,#13310,#13311,#13312,#13313),
 .UNSPECIFIED.,.F.,.F.,(4,3,3,3,3,3,3,3,3,3,3,3,3,3,3,3,3,3,3,3,3,3,3,3,
3,3,3,3,3,3,4),(-0.757763664684535,-0.720404510040711,-0.682461164219946,
-0.666249834426737,-0.657224676989519,-0.619850542291522,-0.582626533293054,
-0.567658451151491,-0.562369519249481,-0.525849388385921,-0.489664449823462,
-0.454476048800286,-0.419529152402925,-0.414641233789178,-0.379750615840662,
-0.370388554325077,-0.334979505679834,-0.299304808423338,-0.281536130666203,
-0.274019724168078,-0.268423813976394,-0.2336927258581,-0.198996831100818,
-0.165024314498677,-0.137477765641968,-0.130952085419143,-0.0975573927314685,
-0.0646607816327848,-0.0327251878282178,-0.0152860524042387,0.),
 .UNSPECIFIED.);
#1364=B_SPLINE_CURVE_WITH_KNOTS('',3,(#13538,#13539,#13540,#13541,#13542,
#13543,#13544,#13545,#13546,#13547,#13548,#13549,#13550,#13551,#13552,#13553,
#13554,#13555,#13556,#13557,#13558,#13559,#13560,#13561,#13562,#13563,#13564,
#13565,#13566,#13567,#13568,#13569,#13570,#13571,#13572,#13573,#13574,#13575,
#13576,#13577,#13578,#13579,#13580,#13581,#13582,#13583,#13584,#13585,#13586,
#13587,#13588,#13589,#13590,#13591,#13592,#13593,#13594,#13595,#13596,#13597,
#13598,#13599,#13600,#13601,#13602,#13603,#13604,#13605,#13606,#13607,#13608,
#13609,#13610,#13611,#13612,#13613,#13614,#13615,#13616,#13617,#13618,#13619,
#13620,#13621,#13622,#13623,#13624,#13625,#13626,#13627,#13628),
 .UNSPECIFIED.,.F.,.F.,(4,3,3,3,3,3,3,3,3,3,3,3,3,3,3,3,3,3,3,3,3,3,3,3,
3,3,3,3,3,3,4),(0.,0.0316034434157731,0.0643812777074898,0.0977466289617717,
0.11960441098055,0.130201724528789,0.138589441131514,0.172845323700023,
0.207497100291187,0.242107499729991,0.272608885111999,0.27741003130413,
0.313030306842683,0.348526801780242,0.353562303825158,0.388378619449034,
0.410240614928535,0.416663398207457,0.421583450321561,0.457807847609702,
0.49385749865802,0.530474689112555,0.566481039474124,0.571906953632555,
0.609227363829363,0.646598106922613,0.656083906904154,0.662136336864782,
0.700826509992472,0.739516683120162,0.757690266844663),.UNSPECIFIED.);
#1365=B_SPLINE_CURVE_WITH_KNOTS('',3,(#13650,#13651,#13652,#13653,#13654,
#13655,#13656,#13657,#13658,#13659,#13660,#13661,#13662,#13663,#13664,#13665,
#13666,#13667,#13668,#13669,#13670,#13671,#13672,#13673,#13674,#13675,#13676,
#13677,#13678,#13679,#13680,#13681,#13682,#13683,#13684,#13685,#13686,#13687,
#13688,#13689,#13690,#13691,#13692,#13693,#13694,#13695,#13696,#13697,#13698,
#13699,#13700,#13701,#13702,#13703,#13704,#13705,#13706,#13707,#13708,#13709,
#13710,#13711,#13712,#13713,#13714,#13715,#13716,#13717,#13718,#13719,#13720,
#13721,#13722,#13723,#13724,#13725,#13726,#13727,#13728,#13729,#13730,#13731,
#13732,#13733,#13734,#13735,#13736,#13737,#13738,#13739,#13740,#13741,#13742,
#13743,#13744,#13745,#13746,#13747,#13748,#13749,#13750,#13751,#13752,#13753,
#13754,#13755,#13756,#13757,#13758,#13759),.UNSPECIFIED.,.F.,.F.,(4,2,2,
2,2,2,2,2,2,2,2,2,2,2,2,2,2,2,2,2,2,2,2,2,2,2,2,2,2,2,2,2,2,2,2,2,2,2,2,
2,2,2,2,2,2,2,2,2,2,2,2,2,2,2,4),(-1.46839216655186,-1.42833493122557,-1.40983960309952,
-1.39649008476235,-1.38192245258612,-1.35595026682801,-1.32006579388245,
-1.25739415958123,-1.24599994074249,-1.23838263735435,-1.2292335836828,
-1.20895486413597,-1.17609120945209,-1.11172712552003,-1.09300158666968,
-1.07960228916858,-1.06507837657971,-1.03947664653156,-1.00445705495045,
-0.941126403182701,-0.929252655631959,-0.921667552812672,-0.912906557233483,
-0.894754745947669,-0.867289011584784,-0.789797140050929,-0.772858151395854,
-0.759724672664605,-0.744718751329267,-0.715589302934294,-0.671818863481682,
-0.624725490925685,-0.612046960332389,-0.605030943441965,-0.596793484943762,
-0.581814683947116,-0.521809333456173,-0.475770727809289,-0.456880324092417,
-0.443431024636274,-0.428912818539185,-0.40347690482787,-0.368790757052006,
-0.305998460037176,-0.293741810698422,-0.286007401773675,-0.277001834303914,
-0.2582504497825,-0.229364741447431,-0.158963286891711,-0.141351957341446,
-0.127920650801248,-0.112746328135276,-0.0837659472426957,-0.00482640158894297),
 .UNSPECIFIED.);
#1366=B_SPLINE_CURVE_WITH_KNOTS('',3,(#13762,#13763,#13764,#13765,#13766,
#13767,#13768,#13769,#13770,#13771,#13772,#13773,#13774,#13775,#13776,#13777,
#13778,#13779,#13780,#13781,#13782,#13783,#13784,#13785,#13786,#13787,#13788,
#13789,#13790,#13791,#13792,#13793,#13794,#13795,#13796,#13797,#13798,#13799,
#13800,#13801,#13802,#13803,#13804,#13805,#13806,#13807,#13808,#13809,#13810,
#13811,#13812,#13813,#13814,#13815,#13816,#13817,#13818,#13819,#13820,#13821,
#13822,#13823,#13824,#13825,#13826,#13827,#13828,#13829,#13830,#13831,#13832,
#13833,#13834,#13835,#13836,#13837,#13838,#13839,#13840,#13841,#13842,#13843),
 .UNSPECIFIED.,.F.,.F.,(4,2,2,2,2,2,2,2,2,2,2,2,2,2,2,2,2,2,2,2,2,2,2,2,
2,2,2,2,2,2,2,2,2,2,2,2,2,2,2,2,4),(-12.9928680261101,-12.9859224043785,
-12.9767663441379,-12.9317684829387,-12.8787491107298,-12.8585962440726,
-12.843864647075,-12.8272831513426,-12.7952673642781,-12.7272779370865,
-12.7034734144216,-12.6867491934808,-12.6781417326004,-12.6706722689398,
-12.6588036168692,-12.5925791120038,-12.559965517409,-12.5357561764214,
-12.5219312356032,-12.5092183047936,-12.4916768823375,-12.4031982185048,
-12.3811372405126,-12.3655143239889,-12.3574349585401,-12.3497117864246,
-12.3373035405743,-12.2745292128648,-12.239536256517,-12.2138553471672,
-12.1992108316161,-12.185635321062,-12.1695331810739,-12.0996377675633,
-12.0705351122928,-12.0517005184064,-12.0426844314299,-12.034958762972,
-12.0227451090155,-11.9599676349854,-11.9265167435349),.UNSPECIFIED.);
#1367=B_SPLINE_CURVE_WITH_KNOTS('',3,(#13848,#13849,#13850,#13851,#13852,
#13853,#13854,#13855,#13856,#13857,#13858,#13859,#13860,#13861,#13862,#13863,
#13864,#13865,#13866,#13867,#13868,#13869,#13870,#13871,#13872,#13873,#13874,
#13875,#13876,#13877,#13878,#13879,#13880,#13881,#13882,#13883,#13884,#13885,
#13886,#13887,#13888,#13889,#13890,#13891,#13892,#13893,#13894,#13895,#13896,
#13897,#13898,#13899,#13900,#13901,#13902,#13903,#13904,#13905,#13906,#13907,
#13908,#13909,#13910,#13911,#13912,#13913,#13914,#13915,#13916,#13917,#13918,
#13919,#13920,#13921,#13922,#13923,#13924,#13925,#13926,#13927,#13928,#13929,
#13930,#13931,#13932,#13933,#13934,#13935,#13936,#13937,#13938,#13939,#13940,
#13941,#13942,#13943,#13944,#13945,#13946,#13947,#13948,#13949,#13950,#13951,
#13952,#13953,#13954,#13955,#13956,#13957,#13958,#13959,#13960,#13961,#13962,
#13963,#13964,#13965,#13966,#13967,#13968,#13969,#13970,#13971,#13972,#13973,
#13974,#13975,#13976,#13977,#13978,#13979,#13980,#13981,#13982,#13983,#13984,
#13985,#13986,#13987,#13988,#13989,#13990,#13991,#13992,#13993,#13994,#13995,
#13996,#13997,#13998,#13999,#14000,#14001,#14002,#14003,#14004,#14005,#14006,
#14007),.UNSPECIFIED.,.F.,.F.,(4,2,2,2,2,2,2,2,2,2,2,2,2,2,2,2,2,2,2,2,
2,2,2,2,2,2,2,2,2,2,2,2,2,2,2,2,2,2,2,2,2,2,2,2,2,2,2,2,2,2,2,2,2,2,2,2,
2,2,2,2,2,2,2,2,2,2,2,2,2,2,2,2,2,2,2,2,2,2,2,4),(-3.49867878100114,-3.48078195894374,
-3.46955972522698,-3.46197286794586,-3.45277159842556,-3.43205243267988,
-3.39797610063354,-3.33546990288741,-3.31654806244602,-3.30313938427867,
-3.28872610459223,-3.263693666223,-3.22988764964021,-3.16560395356786,-3.15313346501676,
-3.14544256963846,-3.13683534548366,-3.11979450354527,-3.09492308948557,
-3.01527193149294,-2.99739186424985,-2.98411787341524,-2.96928256762587,
-2.94165310746421,-2.90187154715814,-2.84744108782649,-2.83519835180177,
-2.82754492556646,-2.81885783486495,-2.80134935179091,-2.77541919752302,
-2.69874979137671,-2.68038057439865,-2.66704941358868,-2.65243562926348,
-2.6261741549808,-2.58964121940858,-2.52834010486826,-2.51679218417816,
-2.50916638327307,-2.50014259245465,-2.48058056285362,-2.44963644828718,
-2.38085364722827,-2.36257423529482,-2.3492540741215,-2.33460217519332,
-2.30810824640674,-2.27103873044209,-2.21095127043577,-2.19926909881182,
-2.19162334288848,-2.18265751788382,-2.1634770024513,-2.13351351801827,
-2.06259963370997,-2.04459412536108,-2.03130461939912,-2.016525598512,-1.98925576826921,
-1.95035384678123,-1.89421291245162,-1.88210670171816,-1.87447641278316,
-1.86574577853761,-1.84795589000478,-1.82136965309309,-1.74647395934031,
-1.72781643493424,-1.71445588254354,-1.69997280638284,-1.67445876507744,
-1.6395921546019,-1.57666462581832,-1.56449569108919,-1.55685831797228,
-1.54815224960004,-1.53052436699322,-1.50432028007254,-1.46839216655186),
 .UNSPECIFIED.);
#1368=B_SPLINE_CURVE_WITH_KNOTS('',3,(#14008,#14009,#14010,#14011,#14012,
#14013,#14014,#14015,#14016,#14017,#14018,#14019,#14020,#14021,#14022,#14023,
#14024,#14025,#14026,#14027,#14028,#14029,#14030,#14031,#14032,#14033,#14034,
#14035,#14036,#14037,#14038,#14039,#14040,#14041,#14042,#14043,#14044,#14045,
#14046,#14047,#14048,#14049,#14050,#14051,#14052,#14053,#14054,#14055,#14056,
#14057,#14058,#14059,#14060,#14061,#14062,#14063,#14064,#14065,#14066,#14067,
#14068,#14069,#14070,#14071,#14072,#14073,#14074,#14075,#14076,#14077,#14078,
#14079,#14080,#14081,#14082,#14083,#14084,#14085,#14086,#14087,#14088,#14089,
#14090,#14091,#14092,#14093,#14094,#14095,#14096,#14097,#14098,#14099,#14100,
#14101,#14102,#14103,#14104,#14105,#14106,#14107,#14108,#14109,#14110,#14111,
#14112,#14113,#14114,#14115,#14116,#14117,#14118,#14119,#14120,#14121,#14122,
#14123,#14124,#14125,#14126,#14127,#14128,#14129,#14130,#14131,#14132,#14133,
#14134,#14135,#14136,#14137,#14138,#14139,#14140,#14141,#14142,#14143,#14144,
#14145,#14146,#14147,#14148,#14149,#14150,#14151,#14152,#14153,#14154,#14155,
#14156,#14157,#14158,#14159,#14160,#14161,#14162,#14163,#14164,#14165),
 .UNSPECIFIED.,.F.,.F.,(4,2,2,2,2,2,2,2,2,2,2,2,2,2,2,2,2,2,2,2,2,2,2,2,
2,2,2,2,2,2,2,2,2,2,2,2,2,2,2,2,2,2,2,2,2,2,2,2,2,2,2,2,2,2,2,2,2,2,2,2,
2,2,2,2,2,2,2,2,2,2,2,2,2,2,2,2,2,2,4),(-11.9265167435349,-11.9253010671319,
-11.8998775010244,-11.8853659903058,-11.8719222083261,-11.853038636317,
-11.8070670854776,-11.7469950171144,-11.732009875923,-11.7237734567874,
-11.7167614908132,-11.7040962421554,-11.657144644663,-11.613348594958,-11.5842158731154,
-11.5692140131739,-11.5560858712183,-11.5391563059077,-11.4616146846684,
-11.4341620971523,-11.4160188349624,-11.4072614323029,-11.3996791529454,
-11.3878096466355,-11.3295052301493,-11.2916491109299,-11.2648076084194,
-11.2500856128337,-11.2367575434473,-11.2185487998283,-11.1495201728474,
-11.1188782881042,-11.0994366818601,-11.0904187427783,-11.0827715924609,
-11.0711299783697,-11.0108006877799,-10.9739293014615,-10.9475272769351,
-10.9328929903791,-10.919570571438,-10.9012581537384,-10.8241647393242,
-10.7983532562927,-10.7808988714022,-10.7722242463342,-10.7645771798208,
-10.7523362255452,-10.6981722958883,-10.6583176476268,-10.6306685501689,
-10.6158432715508,-10.602589118057,-10.5847552249583,-10.5125151252235,
-10.4830685178717,-10.4640972285704,-10.4551729237098,-10.4475245495813,
-10.4357933954727,-10.3762476656135,-10.3389794411438,-10.3124002139746,
-10.2977349418755,-10.2844183959626,-10.2661684350075,-10.1971897108364,
-10.1663518150652,-10.1468330124204,-10.137815162146,-10.1301865446066,
-10.1186200205451,-10.057586096903,-10.0209901905299,-9.99470377217364,
-9.98008828052383,-9.96676098275258,-9.94840609177415,-9.89731205748756),
 .UNSPECIFIED.);
#1369=B_SPLINE_CURVE_WITH_KNOTS('',3,(#14170,#14171,#14172,#14173,#14174,
#14175,#14176,#14177,#14178,#14179,#14180,#14181,#14182,#14183,#14184,#14185,
#14186,#14187,#14188,#14189,#14190,#14191,#14192,#14193,#14194,#14195,#14196,
#14197,#14198,#14199,#14200,#14201,#14202,#14203,#14204,#14205,#14206,#14207,
#14208,#14209,#14210,#14211,#14212,#14213,#14214,#14215,#14216,#14217,#14218,
#14219,#14220,#14221,#14222,#14223,#14224,#14225,#14226,#14227,#14228,#14229,
#14230,#14231,#14232,#14233,#14234,#14235,#14236,#14237,#14238,#14239,#14240,
#14241,#14242,#14243,#14244,#14245,#14246,#14247,#14248,#14249,#14250,#14251,
#14252,#14253,#14254,#14255,#14256,#14257,#14258,#14259,#14260,#14261,#14262,
#14263,#14264,#14265,#14266,#14267,#14268,#14269,#14270,#14271,#14272,#14273,
#14274,#14275,#14276,#14277,#14278,#14279,#14280,#14281,#14282,#14283,#14284,
#14285,#14286,#14287,#14288,#14289,#14290,#14291,#14292,#14293,#14294,#14295,
#14296,#14297,#14298,#14299,#14300,#14301,#14302,#14303,#14304,#14305,#14306,
#14307,#14308,#14309,#14310,#14311,#14312,#14313,#14314,#14315,#14316,#14317,
#14318,#14319,#14320,#14321,#14322,#14323,#14324,#14325,#14326,#14327),
 .UNSPECIFIED.,.F.,.F.,(4,2,2,2,2,2,2,2,2,2,2,2,2,2,2,2,2,2,2,2,2,2,2,2,
2,2,2,2,2,2,2,2,2,2,2,2,2,2,2,2,2,2,2,2,2,2,2,2,2,2,2,2,2,2,2,2,2,2,2,2,
2,2,2,2,2,2,2,2,2,2,2,2,2,2,2,2,2,2,4),(-5.52967993174404,-5.52746103895827,
-5.51301726605171,-5.48781751392462,-5.45365608075187,-5.39023974331564,
-5.37763154077627,-5.37060511658607,-5.36232751823559,-5.34710774761743,
-5.32609931402627,-5.2862261887768,-5.24174894981634,-5.22298786851781,
-5.2095987033326,-5.19512334302082,-5.16973497836552,-5.13516395069695,
-5.07314639039331,-5.06018581576942,-5.05310310809778,-5.04492307594188,
-5.03021949666535,-5.01023868726809,-4.94186884287386,-4.91337098939853,
-4.89839769785815,-4.88514869317986,-4.86752871096216,-4.80838931035308,
-4.75396056823127,-4.74171236882094,-4.734055979712,-4.72536542702825,-4.70785112905183,
-4.68191322298387,-4.60521466097691,-4.58683882554718,-4.57350193498445,
-4.5588808435482,-4.53260225217019,-4.49603942555881,-4.43475512973231,
-4.42319834572813,-4.41556866284627,-4.40654243879864,-4.38698036174205,
-4.35604271661056,-4.28721316259916,-4.26893202003434,-4.25560773622987,
-4.24094857896087,-4.21443280452239,-4.17732242330325,-4.11726652960083,
-4.10557436659351,-4.0979264437805,-4.08896619952871,-4.06982003452643,
-4.03994975453202,-3.96871964483552,-3.95074163312683,-3.93745485665172,
-3.92266291296092,-3.89531644100836,-3.85623277292381,-3.80042416657247,
-3.7882820156738,-3.78064331846076,-3.7719145791267,-3.75417031696167,-3.7276991511797,
-3.65248254650758,-3.63386775502272,-3.62050141253184,-3.60597794025483,
-3.58028256336171,-3.54503001769459,-3.49867878100114),.UNSPECIFIED.);
#1370=B_SPLINE_CURVE_WITH_KNOTS('',3,(#14328,#14329,#14330,#14331,#14332,
#14333,#14334,#14335,#14336,#14337,#14338,#14339,#14340,#14341,#14342,#14343,
#14344,#14345,#14346,#14347,#14348,#14349,#14350,#14351,#14352,#14353,#14354,
#14355,#14356,#14357,#14358,#14359,#14360,#14361,#14362,#14363,#14364,#14365,
#14366,#14367,#14368,#14369,#14370,#14371,#14372,#14373,#14374,#14375,#14376,
#14377,#14378,#14379,#14380,#14381,#14382,#14383,#14384,#14385,#14386,#14387,
#14388,#14389,#14390,#14391,#14392,#14393,#14394,#14395,#14396,#14397,#14398,
#14399,#14400,#14401,#14402,#14403,#14404,#14405,#14406,#14407,#14408,#14409,
#14410,#14411,#14412,#14413,#14414,#14415,#14416,#14417,#14418,#14419,#14420,
#14421,#14422,#14423,#14424,#14425,#14426,#14427,#14428,#14429,#14430,#14431,
#14432,#14433,#14434,#14435,#14436,#14437,#14438,#14439,#14440,#14441,#14442,
#14443,#14444,#14445,#14446,#14447,#14448,#14449,#14450,#14451,#14452,#14453,
#14454,#14455,#14456,#14457,#14458,#14459,#14460,#14461,#14462,#14463,#14464,
#14465,#14466,#14467,#14468,#14469,#14470,#14471,#14472,#14473,#14474,#14475,
#14476,#14477,#14478,#14479,#14480,#14481,#14482,#14483,#14484,#14485,#14486,
#14487),.UNSPECIFIED.,.F.,.F.,(4,2,2,2,2,2,2,2,2,2,2,2,2,2,2,2,2,2,2,2,
2,2,2,2,2,2,2,2,2,2,2,2,2,2,2,2,2,2,2,2,2,2,2,2,2,2,2,2,2,2,2,2,2,2,2,2,
2,2,2,2,2,2,2,2,2,2,2,2,2,2,2,2,2,2,2,2,2,2,2,4),(-9.89731205748756,-9.87162361382395,
-9.84571672148278,-9.8282203325955,-9.81953673147491,-9.81188557016175,
-9.79964504010395,-9.7453353927449,-9.68588701052147,-9.66840892468634,
-9.65518233720158,-9.64014951983856,-9.61121679086927,-9.54710288205336,
-9.52518442005323,-9.50952273187202,-9.50116641415943,-9.49323726967608,
-9.47984096142707,-9.41841483438956,-9.38405272533443,-9.35876460570814,
-9.34431150527036,-9.33092351702992,-9.31213081036045,-9.26682809174202,
-9.20592344878349,-9.19124586497382,-9.18307356778884,-9.17599233018182,
-9.16302464101464,-9.1010926825414,-9.06656652339253,-9.04120314257779,
-9.02673764776751,-9.0133547716598,-8.99459796382821,-8.93015897051987,
-8.89709054613671,-8.87673519280996,-8.86758962770716,-8.85999320107415,
-8.84867813277258,-8.7853386484155,-8.7497414683527,-8.72389307464899,-8.70934690228895,
-8.69599256884213,-8.67745006654022,-8.61089742105274,-8.57888085009621,
-8.5589128575847,-8.5498257876899,-8.54221504342842,-8.53078833786196,-8.46843943241757,
-8.43240433177706,-8.40636060077543,-8.39178154341029,-8.37843687642808,
-8.35997416897036,-8.29268815485724,-8.26101887053062,-8.24118064506504,
-8.23211306100547,-8.22449675695535,-8.21303015286522,-8.1510306685194,
-8.11483687606373,-8.08872245947601,-8.07413118823732,-8.06078943327742,
-8.04235415192669,-7.96600531183447,-7.93992674806435,-7.92235335104717,
-7.91365413696589,-7.90600425157219,-7.89378828854135,-7.86715098468372),
 .UNSPECIFIED.);
#1371=B_SPLINE_CURVE_WITH_KNOTS('',3,(#14492,#14493,#14494,#14495,#14496,
#14497,#14498,#14499,#14500,#14501,#14502,#14503,#14504,#14505,#14506,#14507,
#14508,#14509,#14510,#14511,#14512,#14513,#14514,#14515,#14516,#14517,#14518,
#14519,#14520,#14521,#14522,#14523,#14524,#14525,#14526,#14527,#14528,#14529,
#14530,#14531,#14532,#14533,#14534,#14535,#14536,#14537,#14538,#14539,#14540,
#14541,#14542,#14543,#14544,#14545,#14546,#14547,#14548,#14549,#14550,#14551,
#14552,#14553,#14554,#14555,#14556,#14557,#14558,#14559,#14560,#14561,#14562,
#14563,#14564,#14565,#14566,#14567,#14568,#14569,#14570,#14571,#14572,#14573,
#14574,#14575,#14576,#14577,#14578,#14579,#14580,#14581,#14582,#14583,#14584,
#14585,#14586,#14587,#14588,#14589,#14590,#14591,#14592,#14593,#14594,#14595,
#14596,#14597,#14598,#14599,#14600,#14601,#14602,#14603,#14604,#14605,#14606,
#14607,#14608,#14609,#14610,#14611,#14612,#14613,#14614,#14615,#14616,#14617,
#14618,#14619,#14620,#14621,#14622,#14623,#14624,#14625,#14626,#14627,#14628,
#14629,#14630,#14631,#14632,#14633,#14634,#14635,#14636,#14637,#14638,#14639,
#14640,#14641,#14642,#14643,#14644,#14645,#14646,#14647,#14648,#14649,#14650,
#14651),.UNSPECIFIED.,.F.,.F.,(4,2,2,2,2,2,2,2,2,2,2,2,2,2,2,2,2,2,2,2,
2,2,2,2,2,2,2,2,2,2,2,2,2,2,2,2,2,2,2,2,2,2,2,2,2,2,2,2,2,2,2,2,2,2,2,2,
2,2,2,2,2,2,2,2,2,2,2,2,2,2,2,2,2,2,2,2,2,2,2,4),(-7.56063401821517,-7.51326854468081,
-7.47889664780859,-7.45359951190156,-7.43914016392443,-7.42574589017486,
-7.40694368778009,-7.36161669798204,-7.30067761794024,-7.28599267208735,
-7.27781655497411,-7.27073204834674,-7.25775916081779,-7.19579411210642,
-7.16124964460926,-7.13587298253407,-7.12140006118494,-7.10801038971074,
-7.0892441541453,-7.04472824612105,-7.00474258976706,-6.98378365646472,
-6.96858944035981,-6.96031683320164,-6.95328802084185,-6.94066412593651,
-6.89833220805518,-6.85135167914178,-6.82105128320064,-6.80580836526909,
-6.79260293075702,-6.77574081761993,-6.7276501901097,-6.67999965453028,
-6.65519724829239,-6.6454479770827,-6.63792609692965,-6.62749571660404,
-6.59724519229377,-6.55192602821455,-6.52190715245824,-6.49871346520397,
-6.48460762258951,-6.47103373223388,-6.45103494619549,-6.42691901801644,
-6.36458802981141,-6.33838427503928,-6.32835459325203,-6.32083982459997,
-6.31089899367771,-6.28442624894019,-6.22954117660892,-6.19013440566297,
-6.17337352547654,-6.16019510881402,-6.14468271966448,-6.11247320760936,
-6.05940469690626,-6.02237763351456,-6.01146819552367,-6.00391204078825,
-5.99451476760146,-5.97243911025324,-5.934347640682,-5.87826230434033,-5.8590946363509,
-5.84564737810772,-5.83130860327909,-5.80673925540333,-5.77392186465499,
-5.70696579358409,-5.69491545313696,-5.6872895397492,-5.67852107487172,
-5.66054991806525,-5.63355162912398,-5.55971108181309,-5.54086217272583,
-5.52967993174404),.UNSPECIFIED.);
#1372=B_SPLINE_CURVE_WITH_KNOTS('',3,(#14652,#14653,#14654,#14655,#14656,
#14657,#14658,#14659,#14660,#14661,#14662,#14663,#14664,#14665,#14666,#14667,
#14668,#14669,#14670,#14671,#14672,#14673,#14674,#14675,#14676,#14677,#14678,
#14679,#14680,#14681,#14682,#14683,#14684,#14685,#14686,#14687,#14688,#14689,
#14690,#14691,#14692,#14693,#14694,#14695,#14696,#14697,#14698,#14699,#14700,
#14701,#14702,#14703,#14704,#14705,#14706,#14707,#14708,#14709,#14710,#14711,
#14712,#14713,#14714,#14715,#14716,#14717,#14718,#14719,#14720,#14721,#14722,
#14723,#14724,#14725,#14726,#14727,#14728,#14729,#14730,#14731,#14732,#14733,
#14734,#14735,#14736,#14737,#14738,#14739,#14740,#14741,#14742,#14743,#14744,
#14745,#14746,#14747,#14748,#14749,#14750,#14751,#14752,#14753,#14754,#14755,
#14756,#14757,#14758,#14759,#14760,#14761,#14762,#14763,#14764,#14765,#14766,
#14767,#14768,#14769,#14770,#14771,#14772,#14773,#14774,#14775,#14776,#14777,
#14778,#14779,#14780,#14781,#14782,#14783,#14784,#14785,#14786,#14787,#14788,
#14789,#14790,#14791,#14792,#14793,#14794,#14795,#14796,#14797,#14798,#14799,
#14800,#14801,#14802,#14803,#14804,#14805,#14806,#14807,#14808,#14809,#14810,
#14811,#14812,#14813),.UNSPECIFIED.,.F.,.F.,(4,2,2,2,2,2,2,2,2,2,2,2,2,
2,2,2,2,2,2,2,2,2,2,2,2,2,2,2,2,2,2,2,2,2,2,2,2,2,2,2,2,2,2,2,2,2,2,2,2,
2,2,2,2,2,2,2,2,2,2,2,2,2,2,2,2,2,2,2,2,2,2,2,2,2,2,2,2,2,2,2,4),(-7.86715098468372,
-7.83898087228045,-7.78036523028166,-7.76270811402096,-7.74945801760986,
-7.73451003250844,-7.7061622897504,-7.64100143095205,-7.61912747923954,
-7.60348526415976,-7.59513008643648,-7.58719446284538,-7.57377389478597,
-7.51234747555771,-7.47797998449431,-7.4526860930357,-7.43822860083035,
-7.42483604689371,-7.40603626000087,-7.36071512949483,-7.29978382107827,
-7.28510076359162,-7.27692569673354,-7.26984209924926,-7.2568708750197,
-7.19491378304418,-7.16037375065132,-7.13500034646873,-7.12052928309533,
-7.10714133050446,-7.08837750399718,-7.04386731040103,-7.00388678657383,
-6.98293054409437,-6.96773827864045,-6.95946673348263,-6.95243882343748,
-6.9398165490823,-6.89749006702733,-6.85051556770418,-6.82021906099846,
-6.80497809979182,-6.79177436055578,-6.77491441228576,-6.72682997282342,
-6.67918554233254,-6.65438631699614,-6.6446382969746,-6.63711738248382,
-6.62668834169425,-6.59644170944388,-6.55112836224944,-6.52111333499541,
-6.49792262259055,-6.48381859038211,-6.47024644290493,-6.45025022617551,
-6.4261373973076,-6.36381443577044,-6.33761401890689,-6.32758562157956,
-6.32007181758678,-6.31013226586847,-6.28366294746204,-6.22878505339136,
-6.18938319510126,-6.17262445838086,-6.15944773303133,-6.14393734139516,
-6.11173200926431,-6.05867046731735,-6.02164794627707,-6.0107399037768,
-6.00318471861087,-5.99378865514142,-5.97171585586828,-5.93362935164501,
-5.87755110729914,-5.85838589921919,-5.84494036718781,-5.83652165962026),
 .UNSPECIFIED.);
#1373=B_SPLINE_CURVE_WITH_KNOTS('',3,(#14818,#14819,#14820,#14821,#14822,
#14823,#14824,#14825,#14826,#14827,#14828,#14829,#14830,#14831,#14832,#14833,
#14834,#14835,#14836,#14837,#14838,#14839,#14840,#14841,#14842,#14843,#14844,
#14845,#14846,#14847,#14848,#14849,#14850,#14851,#14852,#14853,#14854,#14855,
#14856,#14857,#14858,#14859,#14860,#14861,#14862,#14863,#14864,#14865,#14866,
#14867,#14868,#14869,#14870,#14871,#14872,#14873,#14874,#14875,#14876,#14877,
#14878,#14879,#14880,#14881,#14882,#14883,#14884,#14885,#14886,#14887,#14888,
#14889,#14890,#14891,#14892,#14893,#14894,#14895,#14896,#14897,#14898,#14899,
#14900,#14901,#14902,#14903,#14904,#14905,#14906,#14907,#14908,#14909,#14910,
#14911,#14912,#14913,#14914,#14915,#14916,#14917,#14918,#14919,#14920,#14921,
#14922,#14923,#14924,#14925,#14926,#14927,#14928,#14929,#14930,#14931,#14932,
#14933,#14934,#14935,#14936,#14937,#14938,#14939,#14940,#14941,#14942,#14943,
#14944,#14945,#14946,#14947,#14948,#14949,#14950,#14951,#14952,#14953,#14954,
#14955,#14956,#14957,#14958,#14959,#14960,#14961,#14962,#14963,#14964,#14965,
#14966,#14967,#14968,#14969,#14970,#14971,#14972,#14973,#14974,#14975,#14976,
#14977),.UNSPECIFIED.,.F.,.F.,(4,2,2,2,2,2,2,2,2,2,2,2,2,2,2,2,2,2,2,2,
2,2,2,2,2,2,2,2,2,2,2,2,2,2,2,2,2,2,2,2,2,2,2,2,2,2,2,2,2,2,2,2,2,2,2,2,
2,2,2,2,2,2,2,2,2,2,2,2,2,2,2,2,2,2,2,2,2,2,2,4),(-9.59119486853264,-9.58541564180725,
-9.52523893204322,-9.51025654432291,-9.5020268834422,-9.49498036148374,
-9.4822289724785,-9.42003528946424,-9.38542265606388,-9.36001906526512,
-9.34554610572673,-9.33216453009469,-9.31342338369265,-9.23896129598912,
-9.2121968184616,-9.19432872957706,-9.18558001225223,-9.17795125516359,
-9.16586597797127,-9.10284839040491,-9.06796227981513,-9.04243355334127,
-9.02793938930535,-9.01456504120352,-8.99588000116821,-8.93066991415714,
-8.897985785038,-8.87776988980236,-8.86864464204234,-8.86104243199963,-8.84968637140788,
-8.78669234038215,-8.75093656094561,-8.72501619065484,-8.71045688641074,
-8.69710474869477,-8.67858913676088,-8.61176188924848,-8.57986951364058,
-8.55994698529019,-8.55086613385593,-8.54325261244276,-8.53181028274389,
-8.46958134221792,-8.43348518380628,-8.4074131814244,-8.3928281755799,-8.37948315628326,
-8.36102841711493,-8.29364283440822,-8.26201257185328,-8.24218805362476,
-8.23312181778317,-8.22550390479095,-8.2140309399148,-8.15206774802931,
-8.11584972015261,-8.0897233252304,-8.0751287711885,-8.06178576659132,-8.04335166011119,
-7.96697159462565,-7.94089749951307,-7.92332524642048,-7.91462549803555,
-7.90697438989995,-7.89475533014395,-7.83996309845466,-7.78132113063378,
-7.76366158402324,-7.75040976924443,-7.73545995014024,-7.70710911882736,
-7.6419389417069,-7.62006223008889,-7.60441803022939,-7.59606178413817,
-7.5881251385117,-7.57470283031182,-7.56063401821517),.UNSPECIFIED.);
#1374=B_SPLINE_CURVE_WITH_KNOTS('',3,(#14978,#14979,#14980,#14981,#14982,
#14983,#14984,#14985,#14986,#14987,#14988,#14989,#14990,#14991,#14992,#14993,
#14994,#14995,#14996,#14997,#14998,#14999,#15000,#15001,#15002,#15003,#15004,
#15005,#15006,#15007,#15008,#15009,#15010,#15011,#15012,#15013,#15014,#15015,
#15016,#15017,#15018,#15019,#15020,#15021,#15022,#15023,#15024,#15025,#15026,
#15027,#15028,#15029,#15030,#15031,#15032,#15033,#15034,#15035,#15036,#15037,
#15038,#15039,#15040,#15041,#15042,#15043,#15044,#15045,#15046,#15047,#15048,
#15049,#15050,#15051,#15052,#15053,#15054,#15055,#15056,#15057,#15058,#15059,
#15060,#15061,#15062,#15063,#15064,#15065,#15066,#15067,#15068,#15069,#15070,
#15071,#15072,#15073,#15074,#15075,#15076,#15077,#15078,#15079,#15080,#15081,
#15082,#15083,#15084,#15085,#15086,#15087,#15088,#15089,#15090,#15091,#15092,
#15093,#15094,#15095,#15096,#15097,#15098,#15099,#15100,#15101,#15102,#15103,
#15104,#15105,#15106,#15107,#15108,#15109,#15110,#15111,#15112,#15113,#15114,
#15115,#15116,#15117,#15118,#15119,#15120,#15121,#15122,#15123,#15124,#15125,
#15126,#15127,#15128,#15129,#15130,#15131,#15132,#15133),.UNSPECIFIED.,
 .F.,.F.,(4,2,2,2,2,2,2,2,2,2,2,2,2,2,2,2,2,2,2,2,2,2,2,2,2,2,2,2,2,2,2,
2,2,2,2,2,2,2,2,2,2,2,2,2,2,2,2,2,2,2,2,2,2,2,2,2,2,2,2,2,2,2,2,2,2,2,2,
2,2,2,2,2,2,2,2,2,2,4),(-5.83652165962026,-5.83060343340443,-5.8060372413055,
-5.77322406706544,-5.70627658063711,-5.69422778881706,-5.68660285467254,
-5.6778355148271,-5.65986666135426,-5.63287182961994,-5.55904078349039,
-5.54019429035759,-5.52679487644636,-5.51235295912005,-5.48715645013475,
-5.45299942006476,-5.38959117828366,-5.37698460102786,-5.36995907990201,
-5.36168254220858,-5.34646471494091,-5.32545895718013,-5.28559098159306,
-5.24111945894058,-5.222360786364,-5.2089733400481,-5.19449983792018,-5.16911473199233,
-5.13454814136845,-5.07253854000887,-5.05957963095843,-5.052497832828,-5.04431885043112,
-5.0296171566623,-5.00963890823567,-4.94127780057389,-4.91278363515482,
-4.89781227043409,-4.88456496582494,-4.86694723725331,-4.80768516548306,
-4.75340874619768,-4.74115445050499,-4.73349783007157,-4.72481128240199,
-4.70731604880015,-4.68141997733795,-4.60462511885929,-4.58626917723554,
-4.57293625961703,-4.55830990177338,-4.53199081093302,-4.49533213249982,
-4.43428099082099,-4.42270076548914,-4.41506872556729,-4.40605598142384,
-4.38657495756673,-4.3558452426953,-4.28657456568634,-4.26835071020849,
-4.25503506367867,-4.24035457830638,-4.21369863751306,-4.17625873129053,
-4.11695049216103,-4.10517752401883,-4.0975189451925,-4.08859798365488,
-4.0696917481748,-4.04042240445074,-3.96779854382722,-3.95000734383667,
-3.93674340072654,-3.92186493432069,-3.89396043893714,-3.85349346320142,
-3.8056948071301),.UNSPECIFIED.);
#1375=B_SPLINE_CURVE_WITH_KNOTS('',3,(#15138,#15139,#15140,#15141,#15142,
#15143,#15144,#15145,#15146,#15147,#15148,#15149,#15150,#15151,#15152,#15153,
#15154,#15155,#15156,#15157,#15158,#15159,#15160,#15161,#15162,#15163,#15164,
#15165,#15166,#15167,#15168,#15169,#15170,#15171,#15172,#15173,#15174,#15175,
#15176,#15177,#15178,#15179,#15180,#15181,#15182,#15183,#15184,#15185,#15186,
#15187,#15188,#15189,#15190,#15191,#15192,#15193,#15194,#15195,#15196,#15197,
#15198,#15199,#15200,#15201,#15202,#15203,#15204,#15205,#15206,#15207,#15208,
#15209,#15210,#15211,#15212,#15213,#15214,#15215,#15216,#15217,#15218,#15219,
#15220,#15221,#15222,#15223,#15224,#15225,#15226,#15227,#15228,#15229,#15230,
#15231,#15232,#15233,#15234,#15235,#15236,#15237,#15238,#15239,#15240,#15241,
#15242,#15243,#15244,#15245,#15246,#15247,#15248,#15249,#15250,#15251,#15252,
#15253,#15254,#15255,#15256,#15257,#15258,#15259,#15260,#15261,#15262,#15263,
#15264,#15265,#15266,#15267,#15268,#15269,#15270,#15271,#15272,#15273,#15274,
#15275,#15276,#15277,#15278,#15279,#15280,#15281,#15282,#15283,#15284,#15285,
#15286,#15287,#15288,#15289,#15290,#15291,#15292,#15293,#15294,#15295,#15296,
#15297),.UNSPECIFIED.,.F.,.F.,(4,2,2,2,2,2,2,2,2,2,2,2,2,2,2,2,2,2,2,2,
2,2,2,2,2,2,2,2,2,2,2,2,2,2,2,2,2,2,2,2,2,2,2,2,2,2,2,2,2,2,2,2,2,2,2,2,
2,2,2,2,2,2,2,2,2,2,2,2,2,2,2,2,2,2,2,2,2,2,2,4),(-11.6209589861144,-11.6133663359858,
-11.5852202047392,-11.5703672184993,-11.5572093879312,-11.5400129782168,
-11.464398022885,-11.4361708524617,-11.4177042261508,-11.4088922037687,
-11.4013266147797,-11.3895760285217,-11.3301634015277,-11.2927997434517,
-11.2661659157797,-11.2514752888791,-11.2381345274991,-11.219841790701,
-11.1430208500536,-11.1172871252356,-11.0998648553724,-11.0911784686328,
-11.0835012274409,-11.0711532604214,-11.0062095874946,-10.972740506592,
-10.9478705224309,-10.9334867383894,-10.9200686462429,-10.9040990587281,
-10.823947907962,-10.7990659565336,-10.7820221778567,-10.7734176075462,
-10.7657368334286,-10.7532945913264,-10.6889548590096,-10.6552225995426,
-10.6302305583084,-10.6158350801731,-10.6024410804383,-10.5835395256831,
-10.5100727904326,-10.4829237501559,-10.4648948869758,-10.456124201246,
-10.4485096159138,-10.4365045995646,-10.3794275399521,-10.3220511806881,
-10.3046514616701,-10.291427296354,-10.2763383060808,-10.2470588104962,
-10.1797595888859,-10.1598889683449,-10.1452444038481,-10.1370765514168,
-10.1299892092107,-10.1169877524896,-10.0550984426467,-10.0205884526424,
-9.9952329698693,-9.9807689227846,-9.96738569180286,-9.94862557158994,-9.90407365533332,
-9.86387149170127,-9.84308018808439,-9.82797182578637,-9.81971851594382,
-9.8126863720025,-9.80002170106756,-9.73711779038159,-9.70281440939386,
-9.67755370248871,-9.66310615132511,-9.64971811400841,-9.63091686560303,
-9.59119486853264),.UNSPECIFIED.);
#1376=B_SPLINE_CURVE_WITH_KNOTS('',3,(#15298,#15299,#15300,#15301,#15302,
#15303,#15304,#15305,#15306,#15307,#15308,#15309,#15310,#15311,#15312,#15313,
#15314,#15315,#15316,#15317,#15318,#15319,#15320,#15321,#15322,#15323,#15324,
#15325,#15326,#15327,#15328,#15329,#15330,#15331,#15332,#15333,#15334,#15335,
#15336,#15337,#15338,#15339,#15340,#15341,#15342,#15343,#15344,#15345,#15346,
#15347,#15348,#15349,#15350,#15351,#15352,#15353,#15354,#15355,#15356,#15357,
#15358,#15359,#15360,#15361,#15362,#15363,#15364,#15365,#15366,#15367,#15368,
#15369,#15370,#15371,#15372,#15373,#15374,#15375,#15376,#15377,#15378,#15379,
#15380,#15381,#15382,#15383,#15384,#15385,#15386,#15387,#15388,#15389,#15390,
#15391,#15392,#15393,#15394,#15395,#15396,#15397,#15398,#15399,#15400,#15401,
#15402,#15403,#15404,#15405,#15406,#15407,#15408,#15409,#15410,#15411,#15412,
#15413,#15414,#15415,#15416,#15417,#15418,#15419,#15420,#15421,#15422,#15423,
#15424,#15425,#15426,#15427,#15428,#15429,#15430,#15431,#15432,#15433,#15434,
#15435,#15436,#15437,#15438,#15439,#15440,#15441,#15442,#15443,#15444,#15445,
#15446,#15447,#15448,#15449,#15450,#15451,#15452,#15453,#15454,#15455),
 .UNSPECIFIED.,.F.,.F.,(4,2,2,2,2,2,2,2,2,2,2,2,2,2,2,2,2,2,2,2,2,2,2,2,
2,2,2,2,2,2,2,2,2,2,2,2,2,2,2,2,2,2,2,2,2,2,2,2,2,2,2,2,2,2,2,2,2,2,2,2,
2,2,2,2,2,2,2,2,2,2,2,2,2,2,2,2,2,2,4),(-3.8056948071301,-3.80026512065085,
-3.78798078993115,-3.78032053900756,-3.77164794451955,-3.75422693301958,
-3.72849750768735,-3.65127124070465,-3.6329928362497,-3.6196721167688,-3.60501834921775,
-3.57851720427146,-3.5414337801098,-3.48135807784409,-3.46967337759391,
-3.46202830157603,-3.4530690061614,-3.43391762282551,-3.40402884300443,
-3.33287805624423,-3.31489714895829,-3.30161332184237,-3.28682956744793,
-3.25951532681412,-3.22050188869135,-3.16459009453224,-3.15246220625848,
-3.14482720911384,-3.13609588845081,-3.11832893183051,-3.09180103978626,
-3.0167851423361,-2.9981465663304,-2.98477948336773,-2.97026967862569,-2.94464264621276,
-2.90953613609495,-2.84588683766129,-2.83427738927482,-2.82664347352911,
-2.81765054826228,-2.79828026756363,-2.76782943230424,-2.69797861537475,
-2.6798361108054,-2.66653513878977,-2.65182902775769,-2.62498780633035,
-2.58710332986536,-2.52881489031045,-2.51693541097618,-2.50933909085913,
-2.50050925903385,-2.4821469123443,-2.45420680869822,-2.37835411535174,
-2.36119191747364,-2.34796592085046,-2.33292479198953,-2.30393982971893,
-2.26064819060926,-2.21286864464054,-2.20013602211377,-2.19309246466381,
-2.1848533004922,-2.16983066704586,-2.09396879350949,-2.05799234407928,
-2.04167922521324,-2.02852484453212,-2.01265975205705,-1.97766511097321,
-1.91336405211699,-1.8890958007975,-1.87935274463646,-1.87184594941125,
-1.86162981250708,-1.83234117395985,-1.77559603949032),.UNSPECIFIED.);
#1377=B_SPLINE_CURVE_WITH_KNOTS('',3,(#15459,#15460,#15461,#15462,#15463,
#15464),.UNSPECIFIED.,.F.,.F.,(4,1,1,4),(-4.09274904019425,-3.93242675008978,
-2.94932006256733,-2.06169017104378),.UNSPECIFIED.);
#1378=B_SPLINE_CURVE_WITH_KNOTS('',3,(#15468,#15469,#15470,#15471,#15472),
 .UNSPECIFIED.,.F.,.F.,(4,1,4),(0.,0.983106687522444,1.11004521091135),
 .UNSPECIFIED.);
#1379=B_SPLINE_CURVE_WITH_KNOTS('',3,(#15474,#15475,#15476,#15477,#15478,
#15479,#15480,#15481,#15482,#15483,#15484,#15485,#15486,#15487,#15488,#15489,
#15490,#15491,#15492,#15493,#15494,#15495,#15496,#15497,#15498,#15499,#15500,
#15501,#15502,#15503,#15504,#15505,#15506,#15507,#15508,#15509,#15510,#15511,
#15512,#15513,#15514,#15515,#15516,#15517,#15518,#15519,#15520,#15521,#15522,
#15523,#15524,#15525,#15526,#15527,#15528,#15529,#15530,#15531,#15532,#15533,
#15534,#15535,#15536,#15537,#15538,#15539,#15540,#15541,#15542,#15543,#15544,
#15545,#15546,#15547,#15548,#15549,#15550,#15551,#15552,#15553,#15554,#15555,
#15556,#15557,#15558,#15559,#15560,#15561,#15562,#15563,#15564,#15565,#15566,
#15567,#15568,#15569,#15570,#15571,#15572,#15573,#15574,#15575,#15576,#15577,
#15578,#15579,#15580,#15581,#15582,#15583,#15584,#15585,#15586,#15587,#15588,
#15589,#15590,#15591,#15592,#15593,#15594,#15595,#15596,#15597,#15598,#15599,
#15600,#15601,#15602,#15603,#15604,#15605,#15606,#15607,#15608,#15609,#15610,
#15611,#15612,#15613,#15614,#15615,#15616,#15617,#15618,#15619,#15620,#15621,
#15622,#15623,#15624,#15625,#15626,#15627,#15628,#15629,#15630,#15631,#15632,
#15633,#15634,#15635,#15636,#15637,#15638,#15639,#15640,#15641,#15642,#15643,
#15644,#15645,#15646,#15647,#15648,#15649,#15650,#15651,#15652,#15653,#15654,
#15655,#15656,#15657,#15658,#15659,#15660,#15661,#15662,#15663,#15664,#15665,
#15666,#15667,#15668,#15669,#15670,#15671,#15672,#15673,#15674,#15675,#15676,
#15677,#15678,#15679,#15680,#15681,#15682,#15683,#15684,#15685,#15686,#15687),
 .UNSPECIFIED.,.F.,.F.,(4,3,3,3,3,3,3,3,3,3,3,3,3,3,3,3,3,3,3,3,3,3,3,3,
3,3,3,3,3,3,3,3,3,3,3,3,3,3,3,3,3,3,3,3,3,3,3,3,3,3,3,3,3,3,3,3,3,3,3,3,
3,3,3,3,3,3,3,3,3,3,3,4),(1.11004521091135,1.19678975220784,1.28343491823949,
1.37000463720176,1.45653382267758,1.5430452412911,1.62956163882972,1.71615883137897,
1.80279632295003,1.88957177193842,1.96621337504489,2.05504161319154,2.14375845460894,
2.23238732145028,2.32200391408991,2.41053563202563,2.49905481643986,2.58758250555964,
2.67801689481156,2.76667099136226,2.8579955269648,2.94932006256733,3.0381928086099,
3.12695687505772,3.21563561039046,3.30523450285287,3.39382229827685,3.48239979811089,
3.57098798371731,3.66134767531043,3.75006715623379,3.84124695316178,3.93242675008978,
4.02106908933155,4.10959899246734,4.19804013238219,4.28772679553595,4.37607010743289,
4.46440098087566,4.55274067520436,4.64343886580633,4.73190750732771,4.82372047246997,
4.91553343761222,5.00429084893833,5.09293715563453,5.18149587482453,5.2711389061133,
5.35960192849135,5.44805309718548,5.5365135366545,5.62704518377454,5.71563458423383,
5.80713735468425,5.89864012513467,5.9873917216973,6.07603240737187,6.16458570587497,
6.25423084422274,6.34268897955531,6.43113547147725,6.51959145102956,6.61013029143644,
6.69871581619304,6.79023131442508,6.88174681265711,6.97411288160619,7.06632853394111,
7.15835923647718,7.25027958940315,7.3420698192528,7.39323051809094),
 .UNSPECIFIED.);
#1380=B_SPLINE_CURVE_WITH_KNOTS('',3,(#15689,#15690,#15691,#15692,#15693,
#15694,#15695,#15696,#15697,#15698,#15699,#15700,#15701,#15702,#15703,#15704,
#15705,#15706,#15707,#15708,#15709,#15710,#15711,#15712,#15713,#15714,#15715,
#15716,#15717,#15718,#15719,#15720,#15721,#15722,#15723,#15724,#15725,#15726,
#15727,#15728,#15729,#15730,#15731,#15732,#15733,#15734,#15735,#15736,#15737,
#15738,#15739,#15740,#15741,#15742,#15743,#15744,#15745,#15746,#15747,#15748,
#15749,#15750,#15751,#15752,#15753,#15754,#15755,#15756,#15757,#15758,#15759,
#15760,#15761,#15762,#15763,#15764,#15765,#15766,#15767,#15768,#15769,#15770,
#15771,#15772,#15773,#15774,#15775,#15776,#15777,#15778,#15779,#15780,#15781,
#15782,#15783,#15784,#15785,#15786,#15787,#15788,#15789,#15790,#15791,#15792,
#15793,#15794,#15795,#15796,#15797,#15798,#15799,#15800,#15801,#15802,#15803,
#15804,#15805,#15806,#15807,#15808,#15809,#15810,#15811,#15812,#15813,#15814,
#15815,#15816,#15817,#15818,#15819,#15820,#15821,#15822,#15823,#15824,#15825,
#15826,#15827,#15828,#15829,#15830,#15831,#15832,#15833,#15834,#15835,#15836,
#15837,#15838,#15839,#15840,#15841,#15842,#15843,#15844,#15845,#15846,#15847,
#15848,#15849,#15850,#15851,#15852,#15853,#15854,#15855,#15856,#15857,#15858,
#15859,#15860,#15861,#15862,#15863,#15864,#15865,#15866,#15867,#15868,#15869,
#15870,#15871,#15872,#15873,#15874,#15875,#15876,#15877,#15878,#15879,#15880,
#15881,#15882,#15883,#15884,#15885,#15886,#15887,#15888,#15889,#15890,#15891,
#15892,#15893,#15894,#15895,#15896,#15897,#15898,#15899,#15900,#15901,#15902),
 .UNSPECIFIED.,.F.,.F.,(4,3,3,3,3,3,3,3,3,3,3,3,3,3,3,3,3,3,3,3,3,3,3,3,
3,3,3,3,3,3,3,3,3,3,3,3,3,3,3,3,3,3,3,3,3,3,3,3,3,3,3,3,3,3,3,3,3,3,3,3,
3,3,3,3,3,3,3,3,3,3,3,4),(7.39323051828195,7.48652054956581,7.58110378721925,
7.67478982599243,7.76982166308599,7.86485350017956,7.95359508066845,8.04222550164844,
8.13076830134049,8.22041728713568,8.30886441436785,8.39729972657984,8.48574436695792,
8.57629832214394,8.66487221403951,8.75641620087076,8.84796018770201,8.9366994182996,
9.02532749057653,9.11386794582422,9.20351781199924,9.29196262122918,9.38039562969083,
9.46883798332746,9.55939520630171,9.64796687526505,9.73951687524475,9.83106687522445,
9.91980333279088,10.0084285796802,10.0969661610973,10.1866170863035,10.2750589210137,
10.3634889224932,10.4519282400123,10.5424895706959,10.6310581587922,10.7226158607695,
10.8141735627469,10.9029121693186,10.9915395941898,11.0800793795962,11.1697294884303,
11.2581735767141,11.3466058462972,11.4350474438882,11.5256056454835,11.6141765224489,
11.7057283863591,11.7972802502693,11.8860183603648,11.974645285871,12.0631845696889,
12.1528348657018,12.241278450278,12.329710216285,12.418151311018,12.5087102177114,
12.5972805982841,12.688833768038,12.7803869377918,12.8681225266378,12.9557475363413,
13.0458310724326,13.1333091513524,13.22075795565,13.3081996293495,13.4002536782799,
13.4877923470092,13.5753806118336,13.6630807303213,13.6764158250714),
 .UNSPECIFIED.);
#1381=B_SPLINE_CURVE_WITH_KNOTS('',3,(#15904,#15905,#15906,#15907,#15908,
#15909,#15910,#15911,#15912,#15913,#15914,#15915,#15916,#15917,#15918,#15919,
#15920,#15921,#15922,#15923,#15924,#15925,#15926,#15927,#15928,#15929,#15930,
#15931,#15932,#15933,#15934,#15935,#15936,#15937,#15938,#15939,#15940,#15941,
#15942,#15943,#15944,#15945,#15946,#15947,#15948,#15949,#15950,#15951,#15952,
#15953,#15954,#15955,#15956,#15957,#15958,#15959,#15960,#15961,#15962,#15963,
#15964,#15965,#15966,#15967,#15968,#15969,#15970,#15971,#15972,#15973,#15974,
#15975,#15976,#15977,#15978,#15979,#15980,#15981,#15982,#15983,#15984,#15985,
#15986,#15987,#15988,#15989,#15990,#15991,#15992,#15993,#15994,#15995,#15996,
#15997,#15998,#15999,#16000,#16001,#16002,#16003,#16004,#16005,#16006,#16007,
#16008,#16009,#16010,#16011,#16012,#16013,#16014,#16015,#16016,#16017,#16018,
#16019,#16020,#16021,#16022,#16023,#16024,#16025,#16026,#16027,#16028,#16029,
#16030,#16031,#16032,#16033,#16034,#16035,#16036,#16037,#16038,#16039,#16040,
#16041,#16042,#16043,#16044,#16045,#16046,#16047,#16048,#16049,#16050,#16051,
#16052,#16053,#16054,#16055,#16056,#16057,#16058,#16059,#16060,#16061,#16062,
#16063,#16064,#16065,#16066,#16067,#16068,#16069,#16070,#16071,#16072,#16073,
#16074,#16075,#16076,#16077,#16078,#16079,#16080,#16081,#16082,#16083,#16084,
#16085,#16086,#16087,#16088,#16089,#16090,#16091,#16092,#16093,#16094,#16095,
#16096,#16097,#16098,#16099,#16100,#16101,#16102,#16103,#16104,#16105,#16106,
#16107,#16108,#16109,#16110,#16111,#16112,#16113,#16114),.UNSPECIFIED.,
 .F.,.F.,(4,3,3,3,3,3,3,3,3,3,3,3,3,3,3,3,3,3,3,3,3,3,3,3,3,3,3,3,3,3,3,
3,3,3,3,3,3,3,3,3,3,3,3,3,3,3,3,3,3,3,3,3,3,3,3,3,3,3,3,3,3,3,3,3,3,3,3,
3,3,3,4),(13.6764158252705,13.7634936253142,13.8522317431468,13.9408586745873,
14.0293979625368,14.1190482563242,14.2074918405328,14.2959236044768,14.3843646954449,
14.4749235997929,14.5634939723758,14.6550471426062,14.7466003128367,14.8353383442683,
14.9239651885601,15.01250438873,15.1021547151836,15.190598210643,15.2790298856361,
15.3674708875542,15.4580299157554,15.5466001998664,15.6381536001127,15.7297070003591,
15.8184450096981,15.9070718313089,15.9956110082415,16.0852613431965,16.1737048141959,
16.2621364643134,16.350577440967,16.4411365026957,16.5297067608031,16.6212602243424,
16.7128136878816,16.801551731529,16.8901785879679,16.9787178002004,17.0683681221008,
17.1568116293316,17.2452433159646,17.3336843293769,17.4242433408836,17.5128136360172,
17.6043670057106,17.695920375404,17.7846584054267,17.8732852480993,17.9618244464429,
18.0514747735033,18.1399182666344,18.2283499391144,18.3167909383364,18.4073499694839,
18.495920250466,18.5874736566962,18.6790270629265,18.7677650921009,18.8563919338726,
18.944931131264,19.0345814586621,19.1230249507207,19.2114566220848,19.2998976201488,
19.3904566527238,19.4790269324526,19.5705803414507,19.6621337504489,19.7691043504165,
19.8748949960292,19.9596009710764),.UNSPECIFIED.);
#1382=B_SPLINE_CURVE_WITH_KNOTS('',3,(#16116,#16117,#16118,#16119,#16120,
#16121,#16122,#16123,#16124,#16125),.UNSPECIFIED.,.F.,.F.,(4,1,1,1,1,1,
1,4),(19.9596011324501,20.6452404379713,21.6283471254938,22.6114538130162,
23.5945605005387,24.5776671880611,25.5607738755836,26.2427864396297),
 .UNSPECIFIED.);
#1383=B_SPLINE_CURVE_WITH_KNOTS('',3,(#16127,#16128,#16129,#16130,#16131,
#16132,#16133,#16134,#16135,#16136,#16137,#16138,#16139,#16140,#16141,#16142,
#16143,#16144,#16145,#16146,#16147,#16148,#16149,#16150,#16151,#16152,#16153,
#16154,#16155,#16156,#16157,#16158,#16159,#16160,#16161,#16162,#16163,#16164,
#16165,#16166,#16167,#16168,#16169,#16170,#16171,#16172,#16173,#16174,#16175,
#16176,#16177,#16178,#16179,#16180,#16181,#16182,#16183,#16184,#16185,#16186,
#16187,#16188,#16189,#16190,#16191,#16192,#16193,#16194,#16195,#16196,#16197,
#16198,#16199,#16200,#16201,#16202,#16203,#16204,#16205,#16206,#16207,#16208,
#16209,#16210,#16211,#16212,#16213,#16214,#16215,#16216,#16217,#16218,#16219,
#16220,#16221,#16222,#16223,#16224,#16225,#16226,#16227,#16228,#16229,#16230,
#16231,#16232,#16233,#16234,#16235,#16236,#16237,#16238,#16239,#16240,#16241,
#16242,#16243,#16244,#16245,#16246,#16247,#16248,#16249,#16250,#16251,#16252,
#16253,#16254,#16255,#16256,#16257,#16258,#16259,#16260,#16261,#16262,#16263,
#16264,#16265,#16266,#16267,#16268,#16269,#16270,#16271,#16272,#16273,#16274,
#16275,#16276,#16277,#16278,#16279,#16280,#16281,#16282,#16283,#16284,#16285,
#16286,#16287,#16288,#16289,#16290,#16291,#16292,#16293,#16294,#16295,#16296,
#16297,#16298,#16299,#16300,#16301,#16302,#16303,#16304,#16305,#16306,#16307,
#16308,#16309,#16310,#16311,#16312,#16313,#16314,#16315,#16316,#16317,#16318,
#16319,#16320,#16321,#16322,#16323,#16324,#16325,#16326,#16327,#16328,#16329,
#16330,#16331,#16332,#16333,#16334,#16335,#16336,#16337),.UNSPECIFIED.,
 .F.,.F.,(4,3,3,3,3,3,3,3,3,3,3,3,3,3,3,3,3,3,3,3,3,3,3,3,3,3,3,3,3,3,3,
3,3,3,3,3,3,3,3,3,3,3,3,3,3,3,3,3,3,3,3,3,3,3,3,3,3,3,3,3,3,3,3,3,3,3,3,
3,3,3,4),(26.2427866070854,26.3479545531162,26.4543084236402,26.543880563106,
26.6326185967606,26.7212454428436,26.8097846443747,26.8994349701564,26.9878784659124,
27.0763101408029,27.1647511422193,27.2553101693216,27.3438804519463,27.4354338512874,
27.5269872506285,27.6157253715144,27.7043523054151,27.7928915952337,27.8825418880984,
27.9709854727142,28.059417236517,28.147858326796,28.2384172296347,28.3269876001762,
28.4185407691635,28.5100939381509,28.5988317636565,28.6874584018148,28.7759973958981,
28.86564779962,28.9540910904238,29.0425225616604,29.1309633609485,29.2215226771297,
29.3100927632426,29.4016466944579,29.4932006256733,29.5819387577266,29.6705657009244,
29.759104998185,29.8487552875613,29.9371988750663,30.0256306400592,30.1140717298361,
30.204630625676,30.2932009915689,30.3847541523824,30.4763073131958,30.5650459322033,
30.6536733670943,30.742213160114,30.8318632651896,30.920307355132,31.0087396241407,
31.0971812189247,31.187739414373,31.2763102830244,31.3678621418713,31.4594140007182,
31.5481503446818,31.6367755000393,31.7253130119065,31.8149639714483,31.9034057910051,
31.9918357977297,32.0802751408886,32.1708365277266,32.2594051917707,32.3509629400057,
32.4425206882407,32.5259717468093),.UNSPECIFIED.);
#1384=B_SPLINE_CURVE_WITH_KNOTS('',3,(#16339,#16340,#16341,#16342,#16343,
#16344,#16345,#16346,#16347,#16348,#16349,#16350,#16351,#16352,#16353,#16354,
#16355,#16356,#16357,#16358,#16359,#16360,#16361,#16362,#16363,#16364,#16365,
#16366,#16367,#16368,#16369,#16370,#16371,#16372,#16373,#16374,#16375,#16376,
#16377,#16378,#16379,#16380,#16381,#16382,#16383,#16384,#16385,#16386,#16387,
#16388,#16389,#16390,#16391,#16392,#16393,#16394,#16395,#16396,#16397,#16398,
#16399,#16400,#16401,#16402,#16403,#16404,#16405,#16406,#16407,#16408,#16409,
#16410,#16411,#16412,#16413,#16414,#16415,#16416,#16417,#16418,#16419,#16420,
#16421,#16422,#16423,#16424,#16425,#16426,#16427,#16428,#16429,#16430,#16431,
#16432,#16433,#16434,#16435,#16436,#16437,#16438,#16439,#16440,#16441,#16442,
#16443,#16444,#16445,#16446,#16447,#16448,#16449,#16450,#16451,#16452,#16453,
#16454,#16455,#16456,#16457,#16458,#16459,#16460,#16461,#16462,#16463,#16464,
#16465,#16466,#16467,#16468,#16469,#16470,#16471,#16472,#16473,#16474,#16475,
#16476,#16477,#16478,#16479,#16480,#16481,#16482,#16483,#16484,#16485,#16486,
#16487,#16488,#16489,#16490,#16491,#16492,#16493,#16494,#16495,#16496,#16497,
#16498,#16499,#16500,#16501,#16502,#16503,#16504,#16505,#16506,#16507,#16508,
#16509,#16510,#16511,#16512,#16513,#16514,#16515,#16516,#16517,#16518,#16519,
#16520,#16521,#16522,#16523,#16524,#16525,#16526,#16527,#16528,#16529,#16530,
#16531,#16532,#16533,#16534,#16535,#16536,#16537,#16538,#16539,#16540,#16541,
#16542,#16543,#16544,#16545,#16546,#16547,#16548,#16549,#16550,#16551,#16552),
 .UNSPECIFIED.,.F.,.F.,(4,3,3,3,3,3,3,3,3,3,3,3,3,3,3,3,3,3,3,3,3,3,3,3,
3,3,3,3,3,3,3,3,3,3,3,3,3,3,3,3,3,3,3,3,3,3,3,3,3,3,3,3,3,3,3,3,3,3,3,3,
3,3,3,3,3,3,3,3,3,3,3,4),(32.5259717470035,32.6136980930916,32.701321678818,
32.7918598909362,32.8793558979929,32.9668299162081,33.0543040619837,33.141800447384,
33.2293879776738,33.3170302208598,33.4047956094643,33.4256273757631,33.5143689611472,
33.6029993860714,33.6915421887604,33.781191173076,33.869638300961,33.9580736129468,
34.0465182522196,34.1370722049861,34.2256460936089,34.3171900784472,34.4087340632856,
34.4974587852672,34.5860723001678,34.6745981676636,34.7642534905566,34.8526837311237,
34.9411022040174,35.02953007149,35.1201077413195,35.2086651786023,35.3002529647052,
35.391840750808,35.4805940901191,35.5692361798978,35.6577905452261,35.7474351568642,
35.8358935245118,35.9243399357615,36.0127955217129,36.1033335008673,36.1919178603191,
36.2834326493248,36.3749474383305,36.4637041692099,36.5523499276875,36.640908230355,
36.7305514672923,36.819014398981,36.9074655991963,36.9959261923746,37.0864581757442,
37.1750480312141,37.2665510785335,37.3580541258529,37.4466911686978,37.5352168033682,
37.6236546985531,37.7133429629058,37.8016855655941,37.8900166797626,37.9783575645755,
38.0690583767754,38.1575305552665,38.2493456843209,38.3411608133753,38.4356542346234,
38.5298819648782,38.6239500559712,38.7177816411047,38.8091570537371),
 .UNSPECIFIED.);
#1385=B_SPLINE_CURVE_WITH_KNOTS('',3,(#16554,#16555,#16556,#16557,#16558,
#16559,#16560,#16561,#16562,#16563,#16564,#16565,#16566,#16567,#16568,#16569,
#16570,#16571,#16572,#16573,#16574,#16575,#16576,#16577,#16578,#16579,#16580,
#16581,#16582,#16583,#16584,#16585,#16586,#16587,#16588,#16589,#16590,#16591,
#16592,#16593,#16594,#16595,#16596,#16597,#16598,#16599,#16600,#16601,#16602),
 .UNSPECIFIED.,.F.,.F.,(4,3,3,3,3,3,3,3,3,3,3,3,3,3,3,3,4),(38.8091570539889,
38.9008783254566,38.9926880493904,39.0846744010417,39.1767552641066,39.2690206125089,
39.3242675008978,39.4119600362523,39.4995435474641,39.5886488497747,39.6760895585896,
39.7635022245041,39.8509090171825,39.9412782543742,40.0287830710683,40.1205845185088,
40.2123859659494),.UNSPECIFIED.);
#1386=B_SPLINE_CURVE_WITH_KNOTS('',3,(#16606,#16607,#16608,#16609),
 .UNSPECIFIED.,.F.,.F.,(4,4),(-42.2735875634651,-41.7918885049275),
 .UNSPECIFIED.);
#1387=B_SPLINE_CURVE_WITH_KNOTS('',3,(#16611,#16612,#16613,#16614,#16615,
#16616,#16617,#16618,#16619,#16620,#16621,#16622,#16623,#16624,#16625,#16626,
#16627,#16628,#16629,#16630,#16631,#16632,#16633,#16634,#16635,#16636,#16637,
#16638,#16639,#16640,#16641,#16642,#16643,#16644,#16645,#16646,#16647,#16648,
#16649,#16650,#16651,#16652,#16653,#16654,#16655,#16656,#16657,#16658,#16659,
#16660,#16661,#16662,#16663,#16664,#16665,#16666,#16667,#16668,#16669,#16670,
#16671,#16672,#16673,#16674,#16675,#16676,#16677,#16678,#16679,#16680,#16681,
#16682,#16683,#16684,#16685,#16686,#16687,#16688,#16689,#16690,#16691,#16692,
#16693,#16694,#16695,#16696,#16697,#16698,#16699,#16700,#16701,#16702,#16703,
#16704,#16705,#16706,#16707,#16708,#16709,#16710,#16711,#16712,#16713,#16714,
#16715,#16716,#16717,#16718,#16719,#16720,#16721,#16722,#16723,#16724,#16725,
#16726,#16727,#16728,#16729,#16730,#16731,#16732,#16733,#16734,#16735,#16736,
#16737,#16738,#16739,#16740,#16741,#16742,#16743,#16744,#16745,#16746,#16747,
#16748,#16749,#16750,#16751,#16752,#16753,#16754,#16755,#16756,#16757,#16758,
#16759,#16760,#16761,#16762,#16763,#16764,#16765,#16766,#16767,#16768,#16769,
#16770,#16771,#16772,#16773,#16774,#16775,#16776,#16777,#16778,#16779,#16780,
#16781,#16782,#16783,#16784,#16785,#16786,#16787,#16788,#16789,#16790,#16791,
#16792,#16793,#16794,#16795,#16796,#16797,#16798,#16799,#16800,#16801,#16802,
#16803,#16804,#16805,#16806,#16807,#16808,#16809,#16810,#16811,#16812,#16813,
#16814,#16815,#16816,#16817,#16818,#16819,#16820,#16821,#16822,#16823,#16824,
#16825,#16826,#16827),.UNSPECIFIED.,.F.,.F.,(4,3,3,3,3,3,3,3,3,3,3,3,3,
3,3,3,3,3,3,3,3,3,3,3,3,3,3,3,3,3,3,3,3,3,3,3,3,3,3,3,3,3,3,3,3,3,3,3,3,
3,3,3,3,3,3,3,3,3,3,3,3,3,3,3,3,3,3,3,3,3,3,3,4),(-41.7918608832718,-41.6963680489168,
-41.6006510282217,-41.5046149620455,-41.4084115456498,-41.3119771500066,
-41.2904808759427,-41.2025196790987,-41.1146804894366,-41.0269387856156,
-40.9369932109662,-40.8493667994677,-40.7617582010694,-40.6741454427343,
-40.5824526291558,-40.4947162756479,-40.406921130202,-40.3190026549469,
-40.3073741884202,-40.218546539833,-40.1298302953959,-40.041202032106,-39.951585215705,
-39.8630541133568,-39.7745355478778,-39.6860084803038,-39.5955732354523,
-39.5069197610933,-39.4155936309956,-39.3242675008978,-39.2353948206761,
-39.1466308219898,-39.0579521562669,-38.9683532384055,-38.8797655167199,
-38.7911880920509,-38.7025999829601,-38.6122401905639,-38.5235207888384,
-38.4323408011069,-38.3411608133753,-38.2525182595748,-38.1639881390155,
-38.075546779094,-37.9858601974389,-37.8975166605352,-37.8091855605984,
-37.7208456385293,-37.6301477603602,-37.5416788900287,-37.4498665079408,
-37.3580541258529,-37.2692968116588,-37.180650603046,-37.0920919827586,
-37.0024489147051,-36.9139859925937,-36.8255349244951,-36.7370745858353,
-36.6465427989591,-36.5579534989103,-36.4664504686204,-36.3749474383305,
-36.2873765264958,-36.1999158891338,-36.1125489134617,-36.0252336577821,
-35.9379478187613,-35.8506691225993,-35.7633296057599,-35.6759609642527,
-35.5884727859879,-35.5086755762926),.UNSPECIFIED.);
#1388=B_SPLINE_CURVE_WITH_KNOTS('',3,(#16829,#16830,#16831,#16832,#16833,
#16834,#16835,#16836,#16837,#16838,#16839,#16840,#16841,#16842,#16843,#16844,
#16845,#16846,#16847,#16848,#16849,#16850,#16851,#16852,#16853,#16854,#16855,
#16856,#16857,#16858,#16859,#16860,#16861,#16862,#16863,#16864,#16865,#16866,
#16867,#16868,#16869,#16870,#16871,#16872,#16873,#16874,#16875,#16876,#16877,
#16878,#16879,#16880,#16881,#16882,#16883,#16884,#16885,#16886,#16887,#16888,
#16889,#16890,#16891,#16892,#16893,#16894,#16895,#16896,#16897,#16898,#16899,
#16900,#16901,#16902,#16903,#16904,#16905,#16906,#16907,#16908,#16909,#16910,
#16911,#16912,#16913,#16914,#16915,#16916,#16917,#16918,#16919,#16920,#16921,
#16922,#16923,#16924,#16925,#16926,#16927,#16928,#16929,#16930,#16931,#16932,
#16933,#16934,#16935,#16936,#16937,#16938,#16939,#16940,#16941,#16942,#16943,
#16944,#16945,#16946,#16947,#16948,#16949,#16950,#16951,#16952,#16953,#16954,
#16955,#16956,#16957,#16958,#16959,#16960,#16961,#16962,#16963,#16964,#16965,
#16966,#16967,#16968,#16969,#16970,#16971,#16972,#16973,#16974,#16975,#16976,
#16977,#16978,#16979,#16980,#16981,#16982,#16983,#16984,#16985,#16986,#16987,
#16988,#16989,#16990,#16991,#16992,#16993,#16994,#16995,#16996,#16997,#16998,
#16999,#17000,#17001,#17002,#17003,#17004,#17005,#17006,#17007,#17008,#17009,
#17010,#17011,#17012,#17013,#17014,#17015,#17016,#17017,#17018,#17019,#17020,
#17021,#17022,#17023,#17024,#17025,#17026,#17027,#17028,#17029,#17030,#17031,
#17032,#17033,#17034,#17035,#17036,#17037,#17038,#17039),.UNSPECIFIED.,
 .F.,.F.,(4,3,3,3,3,3,3,3,3,3,3,3,3,3,3,3,3,3,3,3,3,3,3,3,3,3,3,3,3,3,3,
3,3,3,3,3,3,3,3,3,3,3,3,3,3,3,3,3,3,3,3,3,3,3,3,3,3,3,3,3,3,3,3,3,3,3,3,
3,3,3,4),(-35.5086755760922,-35.391840750808,-35.3031151892389,-35.2145009894124,
-35.1259745910799,-35.0363195251056,-34.9478891353215,-34.8594706563773,
-34.7710429260415,-34.6804657103525,-34.5919087638597,-34.5003214135726,
-34.4087340632856,-34.3199925014802,-34.231362099372,-34.1428193187148,
-34.0531703258458,-33.9647232179249,-33.8762879250928,-33.7878433041413,
-33.6972893220468,-33.6087154495152,-33.5171714126391,-33.4256273757631,
-33.3368881467887,-33.2482600762056,-33.1597196227201,-33.0700697559102,
-32.9816249486,-32.8931919421141,-32.8047495905072,-32.7141923649406,-32.6256206981239,
-32.5340706931823,-32.4425206882407,-32.3537842240172,-32.2651589703713,
-32.1766213821072,-32.0869704594336,-31.998528617698,-31.9100986091387,
-31.8216592844933,-31.7310979635495,-31.6425293682761,-31.5509716844972,
-31.4594140007182,-31.3706753975655,-31.2820479761503,-31.1935081942323,
-31.1038580841028,-31.0154139993643,-30.9269817333416,-30.8385401393217,
-30.7479819327903,-30.6594110593904,-30.5678591862931,-30.4763073131958,
-30.3875692030748,-30.2989422775513,-30.2104029937242,-30.1207526977179,
-30.0323091131527,-29.9438773471645,-29.8554362524577,-29.7648773457616,
-29.6763069652342,-29.5847537954538,-29.4932006256734,-29.3821251371914,
-29.2726971433069,-29.2254902691016),.UNSPECIFIED.);
#1389=B_SPLINE_CURVE_WITH_KNOTS('',3,(#17041,#17042,#17043,#17044,#17045,
#17046,#17047,#17048,#17049,#17050,#17051,#17052,#17053,#17054,#17055,#17056,
#17057,#17058,#17059,#17060,#17061,#17062,#17063,#17064,#17065,#17066,#17067,
#17068,#17069,#17070,#17071,#17072,#17073,#17074,#17075,#17076,#17077,#17078,
#17079,#17080,#17081,#17082,#17083,#17084,#17085,#17086,#17087,#17088,#17089,
#17090,#17091,#17092,#17093,#17094,#17095,#17096,#17097,#17098,#17099,#17100,
#17101,#17102,#17103,#17104,#17105,#17106,#17107,#17108,#17109,#17110,#17111,
#17112,#17113,#17114,#17115,#17116,#17117,#17118,#17119,#17120,#17121,#17122,
#17123,#17124,#17125,#17126,#17127,#17128,#17129,#17130,#17131,#17132,#17133,
#17134,#17135,#17136,#17137,#17138,#17139,#17140,#17141,#17142,#17143,#17144,
#17145,#17146,#17147,#17148,#17149,#17150,#17151,#17152,#17153,#17154,#17155,
#17156,#17157,#17158,#17159,#17160,#17161,#17162,#17163,#17164,#17165,#17166,
#17167,#17168,#17169,#17170,#17171,#17172,#17173,#17174,#17175,#17176,#17177,
#17178,#17179,#17180,#17181,#17182,#17183,#17184,#17185,#17186,#17187,#17188,
#17189,#17190,#17191,#17192,#17193,#17194,#17195,#17196,#17197,#17198,#17199,
#17200,#17201,#17202,#17203,#17204,#17205,#17206,#17207,#17208,#17209,#17210,
#17211,#17212,#17213,#17214,#17215,#17216,#17217,#17218,#17219,#17220,#17221,
#17222,#17223,#17224,#17225,#17226,#17227,#17228,#17229,#17230,#17231,#17232,
#17233,#17234,#17235,#17236,#17237,#17238,#17239,#17240,#17241,#17242,#17243,
#17244,#17245,#17246,#17247,#17248,#17249,#17250,#17251,#17252,#17253,#17254),
 .UNSPECIFIED.,.F.,.F.,(4,3,3,3,3,3,3,3,3,3,3,3,3,3,3,3,3,3,3,3,3,3,3,3,
3,3,3,3,3,3,3,3,3,3,3,3,3,3,3,3,3,3,3,3,3,3,3,3,3,3,3,3,3,3,3,3,3,3,3,3,
3,3,3,3,3,3,3,3,3,3,3,4),(-29.2254902689126,-29.1360657275674,-29.0484146342724,
-28.9607809341787,-28.8731426670707,-28.7823804848408,-28.694619127601,
-28.602356532876,-28.5100939381509,-28.4213558209058,-28.3327288900596,
-28.2441896027105,-28.1545393087003,-28.0660957251031,-27.9776639617736,
-27.8892228714222,-27.7986639662237,-27.7100935942577,-27.6185404224431,
-27.5269872506285,-27.4382492191399,-27.3496223747916,-27.261083174566,
-27.1714328481335,-27.0829893526203,-26.9945576775742,-26.906116675604,
-26.8155576474795,-26.7269873633194,-26.6354339632127,-26.543880563106,
-26.455142553632,-26.3665157318838,-26.2779765548121,-26.1883262199085,
-26.0998827487654,-26.0114510985026,-25.9230101217026,-25.8324510601728,
-25.7438808019172,-25.6523273387504,-25.5607738755836,-25.4720358320312,
-25.3834089756885,-25.2948697635533,-25.2052194416168,-25.1167759344851,
-25.0283442479519,-24.9399032346396,-24.849344222995,-24.7607739279617,
-24.6692205580114,-24.5776671880611,-24.4889291580206,-24.40030231533,-24.3117631169686,
-24.2221127899148,-24.133669296766,-24.0452376242682,-23.9567966250287,
-23.8662375939062,-23.7776673129069,-23.6861139067228,-23.5945605005387,
-23.5058251646571,-23.4171988003756,-23.3286601402729,-23.2401879892028,
-23.1517561322677,-23.0633474767187,-22.9749248609848,-22.942304961733),
 .UNSPECIFIED.);
#1390=B_SPLINE_CURVE_WITH_KNOTS('',3,(#17256,#17257,#17258,#17259,#17260,
#17261,#17262,#17263,#17264,#17265,#17266,#17267,#17268,#17269,#17270,#17271,
#17272,#17273,#17274,#17275,#17276,#17277,#17278,#17279,#17280,#17281,#17282,
#17283,#17284,#17285,#17286,#17287,#17288,#17289,#17290,#17291,#17292,#17293,
#17294,#17295,#17296,#17297,#17298,#17299,#17300,#17301,#17302,#17303,#17304,
#17305,#17306,#17307,#17308,#17309,#17310,#17311,#17312,#17313,#17314,#17315,
#17316,#17317,#17318,#17319,#17320,#17321,#17322,#17323,#17324,#17325,#17326,
#17327,#17328,#17329,#17330,#17331,#17332,#17333,#17334,#17335,#17336,#17337,
#17338,#17339,#17340,#17341,#17342,#17343,#17344,#17345,#17346,#17347,#17348,
#17349,#17350,#17351,#17352,#17353,#17354,#17355,#17356,#17357,#17358,#17359,
#17360,#17361,#17362,#17363,#17364,#17365,#17366,#17367,#17368,#17369,#17370,
#17371,#17372,#17373,#17374,#17375,#17376,#17377,#17378,#17379,#17380,#17381,
#17382,#17383,#17384,#17385,#17386,#17387,#17388,#17389,#17390,#17391,#17392,
#17393,#17394,#17395,#17396,#17397,#17398,#17399,#17400,#17401,#17402,#17403,
#17404,#17405,#17406,#17407,#17408,#17409,#17410,#17411,#17412,#17413,#17414,
#17415,#17416,#17417,#17418,#17419,#17420,#17421,#17422,#17423,#17424,#17425,
#17426,#17427,#17428,#17429,#17430,#17431,#17432,#17433,#17434,#17435,#17436,
#17437,#17438,#17439,#17440,#17441,#17442,#17443,#17444,#17445,#17446,#17447,
#17448,#17449,#17450,#17451,#17452,#17453,#17454,#17455,#17456,#17457,#17458,
#17459,#17460,#17461,#17462,#17463,#17464,#17465,#17466,#17467,#17468,#17469),
 .UNSPECIFIED.,.F.,.F.,(4,3,3,3,3,3,3,3,3,3,3,3,3,3,3,3,3,3,3,3,3,3,3,3,
3,3,3,3,3,3,3,3,3,3,3,3,3,3,3,3,3,3,3,3,3,3,3,3,3,3,3,3,3,3,3,3,3,3,3,3,
3,3,3,3,3,3,3,3,3,3,3,4),(-22.9423049615399,-22.8400783057738,-22.7372890055352,
-22.6338727274574,-22.6114538130162,-22.522715780268,-22.4340889348564,
-22.3455497337639,-22.2558994077301,-22.1674559118441,-22.0790242366121,
-21.9905832346442,-21.9000242073566,-21.8114539236697,-21.7199005245817,
-21.6283471254938,-21.5396090947594,-21.4509822513892,-21.3624430523631,
-21.2727927255641,-21.1843492317921,-21.095917558688,-21.0074765588595,
-20.9169175286375,-20.8283472470988,-20.736793842535,-20.6452404379713,
-20.5565024051013,-20.4678755595915,-20.3793363584244,-20.2896860324275,
-20.2012425365252,-20.1128108612988,-20.0243698593582,-19.9338108321309,
-19.8452405485253,-19.7536871494871,-19.6621337504489,-19.5733957215263,
-19.4847688799543,-19.3962296827109,-19.3065793552378,-19.2181358631989,
-19.1297041918064,-19.0412631936662,-18.9507041609813,-18.8621338810578,
-18.7705804719922,-18.6790270629265,-18.5902890326888,-18.5016621898394,
-18.4131229913573,-18.3234726643631,-18.235029171188,-18.1465974986995,
-18.0581564995045,-17.9675974684794,-17.879027187612,-17.787473781508,-17.695920375404,
-17.6071823312881,-17.5185554744915,-17.4300162620112,-17.340365940245,
-17.2519224330382,-17.1634907465309,-17.0750497333459,-16.9844907219798,
-16.8959204273232,-16.8043670576024,-16.7128136878816,-16.6591196545534),
 .UNSPECIFIED.);
#1391=B_SPLINE_CURVE_WITH_KNOTS('',3,(#17471,#17472,#17473,#17474,#17475,
#17476,#17477,#17478,#17479,#17480,#17481,#17482,#17483,#17484,#17485,#17486,
#17487,#17488,#17489,#17490,#17491,#17492,#17493,#17494,#17495,#17496,#17497,
#17498,#17499,#17500,#17501,#17502,#17503,#17504,#17505,#17506,#17507,#17508,
#17509,#17510,#17511,#17512,#17513,#17514,#17515,#17516,#17517,#17518,#17519,
#17520,#17521,#17522,#17523,#17524,#17525,#17526,#17527,#17528,#17529,#17530,
#17531,#17532,#17533,#17534,#17535,#17536,#17537,#17538,#17539,#17540,#17541,
#17542,#17543,#17544,#17545,#17546,#17547,#17548,#17549,#17550,#17551,#17552,
#17553,#17554,#17555,#17556,#17557,#17558,#17559,#17560,#17561,#17562,#17563,
#17564,#17565,#17566,#17567,#17568,#17569,#17570,#17571,#17572,#17573,#17574,
#17575,#17576,#17577,#17578,#17579,#17580,#17581,#17582,#17583,#17584,#17585,
#17586,#17587,#17588,#17589,#17590,#17591,#17592,#17593,#17594,#17595,#17596,
#17597,#17598,#17599,#17600,#17601,#17602,#17603,#17604,#17605,#17606,#17607,
#17608,#17609,#17610,#17611,#17612,#17613,#17614,#17615,#17616,#17617,#17618,
#17619,#17620,#17621,#17622,#17623,#17624,#17625,#17626,#17627,#17628,#17629,
#17630,#17631,#17632,#17633,#17634,#17635,#17636,#17637,#17638,#17639,#17640,
#17641,#17642,#17643,#17644,#17645,#17646,#17647,#17648,#17649,#17650,#17651,
#17652,#17653,#17654,#17655,#17656,#17657,#17658,#17659,#17660,#17661,#17662,
#17663,#17664,#17665,#17666,#17667,#17668,#17669,#17670,#17671,#17672,#17673,
#17674,#17675,#17676,#17677,#17678,#17679,#17680,#17681,#17682,#17683,#17684),
 .UNSPECIFIED.,.F.,.F.,(4,3,3,3,3,3,3,3,3,3,3,3,3,3,3,3,3,3,3,3,3,3,3,3,
3,3,3,3,3,3,3,3,3,3,3,3,3,3,3,3,3,3,3,3,3,3,3,3,3,3,3,3,3,3,3,3,3,3,3,3,
3,3,3,3,3,3,3,3,3,3,3,4),(-16.6591196543998,-16.5711052143565,-16.4831981162794,
-16.3953740081479,-16.3076047990417,-16.2198631460269,-16.1321271600137,
-16.0443749611132,-15.9565340199988,-15.868644220512,-15.7806226675453,
-15.7297070003591,-15.6409689666578,-15.5523421205266,-15.4638029189464,
-15.3741525931827,-15.2857090973743,-15.1972774224304,-15.1088364209597,
-15.0182773939289,-14.9297071112482,-14.8381537120424,-14.7466003128367,
-14.657862192562,-14.5692352592747,-14.4806959700712,-14.3910456769766,
-14.3026020929753,-14.2141703297856,-14.1257292401177,-14.0351703364169,
-13.9465999664761,-13.8550467958951,-13.7634936253142,-13.6747557987345,
-13.5861291595026,-13.4975901643472,-13.4079397610277,-13.3194964691629,
-13.2310649968712,-13.1426241965351,-13.0520648818493,-12.9634947947155,
-12.8719408662536,-12.7803869377918,-12.6916488057979,-12.6030218626512,
-12.5144825654337,-12.4248322760381,-12.3363886885555,-12.2479569235773,
-12.1595158338075,-12.068956937923,-11.9803865720187,-11.888833411144,-11.7972802502693,
-11.7085416347909,-11.6199142034448,-11.5313744139808,-11.4417243075765,
-11.3532802211941,-11.2648479557407,-11.1764063645028,-11.0858481640638,
-10.9972772989043,-10.9057254308256,-10.8141735627469,-10.7185150588642,
-10.6231617411537,-10.5279991843888,-10.4331223296681,-10.3759343476128),
 .UNSPECIFIED.);
#1392=B_SPLINE_CURVE_WITH_KNOTS('',3,(#17685,#17686,#17687,#17688,#17689,
#17690,#17691,#17692,#17693,#17694,#17695,#17696,#17697,#17698,#17699,#17700,
#17701,#17702,#17703,#17704,#17705,#17706,#17707,#17708,#17709,#17710,#17711,
#17712,#17713,#17714,#17715,#17716,#17717,#17718,#17719,#17720,#17721,#17722,
#17723,#17724,#17725,#17726,#17727,#17728,#17729,#17730,#17731,#17732,#17733,
#17734,#17735,#17736,#17737,#17738,#17739,#17740,#17741,#17742,#17743,#17744,
#17745,#17746,#17747,#17748,#17749,#17750,#17751,#17752,#17753,#17754,#17755,
#17756,#17757,#17758,#17759,#17760,#17761,#17762,#17763,#17764,#17765,#17766,
#17767,#17768,#17769,#17770,#17771,#17772,#17773,#17774,#17775,#17776,#17777,
#17778,#17779,#17780,#17781,#17782,#17783,#17784,#17785,#17786,#17787,#17788,
#17789,#17790,#17791,#17792,#17793,#17794,#17795,#17796,#17797,#17798,#17799,
#17800,#17801,#17802,#17803,#17804,#17805,#17806,#17807,#17808,#17809,#17810,
#17811,#17812,#17813,#17814,#17815,#17816,#17817,#17818,#17819,#17820,#17821,
#17822,#17823,#17824,#17825,#17826,#17827,#17828,#17829,#17830,#17831,#17832,
#17833,#17834,#17835,#17836,#17837,#17838,#17839,#17840,#17841,#17842,#17843,
#17844,#17845,#17846,#17847,#17848,#17849,#17850,#17851,#17852,#17853,#17854,
#17855,#17856,#17857,#17858,#17859,#17860,#17861,#17862,#17863,#17864,#17865,
#17866,#17867,#17868,#17869,#17870,#17871,#17872,#17873,#17874,#17875,#17876,
#17877,#17878,#17879,#17880,#17881,#17882,#17883,#17884,#17885,#17886,#17887,
#17888,#17889,#17890,#17891,#17892,#17893,#17894,#17895,#17896,#17897,#17898),
 .UNSPECIFIED.,.F.,.F.,(4,3,3,3,3,3,3,3,3,3,3,3,3,3,3,3,3,3,3,3,3,3,3,3,
3,3,3,3,3,3,3,3,3,3,3,3,3,3,3,3,3,3,3,3,3,3,3,3,3,3,3,3,3,3,3,3,3,3,3,3,
3,3,3,3,3,3,3,3,3,3,3,4),(-10.3759343473738,-10.2851902025472,-10.1943848714136,
-10.1034269336437,-10.0123921171029,-9.92117043902683,-9.83106687522445,
-9.74232744591289,-9.65369921391586,-9.56515863778241,-9.47550883152236,
-9.38706399749244,-9.29863100026054,-9.2101886938749,-9.11963156733168,
-9.03106003445256,-8.93951011107729,-8.84796018770201,-8.75921862146023,
-8.67058821577755,-8.58204543240453,-8.49239644087641,-8.40394933236375,
-8.3155140397366,-8.22706941978681,-8.136515439885,-8.04794157031955,-7.95639753524956,
-7.86485350017956,-7.77612873502284,-7.68751517689834,-7.59898926618254,
-7.50933395949186,-7.42090367598821,-7.33248516033964,-7.2440572503412,
-7.15347964092018,-7.06492216206265,-6.97333448735988,-6.88174681265711,
-6.79299349255972,-6.70435142178096,-6.61579707521975,-6.52615245645912,
-6.43769410689579,-6.34924771344436,-6.2607921449874,-6.17025414002422,
-6.08166979716281,-5.99015496114874,-5.89864012513467,-5.80988349345781,
-5.721237834732,-5.6326796322351,-5.54303635790724,-5.45457352676152,-5.36612242704649,
-5.27766193421025,-5.18712981006075,-5.09854005361742,-5.00703674561482,
-4.91553343761222,-4.82816672719067,-4.74091103291585,-4.65375084014162,
-4.56664302899291,-4.47956514860665,-4.39249477953229,-4.30537257831964,
-4.21822093231598,-4.13097249351553,-4.09274904019425),.UNSPECIFIED.);
#1393=B_SPLINE_CURVE_WITH_KNOTS('',3,(#17901,#17902,#17903,#17904,#17905,
#17906,#17907,#17908,#17909,#17910,#17911,#17912,#17913,#17914,#17915,#17916,
#17917,#17918,#17919,#17920,#17921,#17922,#17923,#17924,#17925,#17926,#17927,
#17928,#17929,#17930,#17931,#17932,#17933,#17934,#17935,#17936,#17937,#17938,
#17939,#17940,#17941,#17942,#17943,#17944,#17945,#17946,#17947,#17948,#17949,
#17950,#17951,#17952,#17953,#17954,#17955,#17956,#17957,#17958,#17959,#17960,
#17961,#17962,#17963,#17964,#17965,#17966,#17967,#17968,#17969,#17970,#17971,
#17972,#17973,#17974,#17975,#17976,#17977,#17978,#17979,#17980,#17981,#17982,
#17983,#17984,#17985,#17986,#17987,#17988,#17989,#17990,#17991,#17992,#17993,
#17994,#17995,#17996,#17997,#17998,#17999,#18000,#18001,#18002,#18003,#18004,
#18005,#18006,#18007,#18008,#18009,#18010,#18011,#18012,#18013,#18014,#18015,
#18016,#18017,#18018,#18019,#18020,#18021,#18022,#18023,#18024,#18025,#18026,
#18027,#18028,#18029,#18030,#18031,#18032,#18033,#18034,#18035,#18036),
 .UNSPECIFIED.,.F.,.F.,(4,2,2,2,2,2,2,2,2,2,2,2,2,2,2,2,2,2,2,2,2,2,2,2,
2,2,2,2,2,2,2,2,2,2,2,2,2,2,2,2,2,2,2,2,2,2,2,2,2,2,2,2,2,2,2,2,2,2,2,2,
2,2,2,2,2,2,2,4),(-1.77559603949032,-1.76123154608128,-1.7347774998451,
-1.72014143363947,-1.7068339629146,-1.68857155834236,-1.63315424891479,
-1.57627821739527,-1.56425230882687,-1.556637450491,-1.54787596729481,-1.52991828878332,
-1.50294441993861,-1.42904210726485,-1.41020593191291,-1.39681096212694,
-1.38237120796975,-1.35716756233058,-1.32297978190903,-1.25979963496362,
-1.24717229379129,-1.24013906968697,-1.23183624951668,-1.21654647058489,
-1.13819900867779,-1.10478593438375,-1.0886994354341,-1.07552469652321,
-1.05938339279416,-1.0221529379589,-0.945373097674644,-0.931168721675339,
-0.923086896639897,-0.914980731472239,-0.900470464774507,-0.829383392842492,
-0.788686358912283,-0.771942396221659,-0.758847828752075,-0.743525574560414,
-0.712224269767771,-0.662032602029656,-0.624325944085348,-0.611799382621773,
-0.604806613441647,-0.596524834506089,-0.581312003040091,-0.560333974050935,
-0.520212979478024,-0.475549380629993,-0.456720884664485,-0.443279701400228,
-0.428738464622379,-0.403165689810354,-0.368178944476579,-0.303773218212403,
-0.292552367632876,-0.284863377728665,-0.27529201983579,-0.252724455737363,
-0.21291224578363,-0.161665817941933,-0.142706624100451,-0.129150343477715,
-0.114427133356919,-0.0883041265988544,-0.0523412071009701,-0.00482582262840578),
 .UNSPECIFIED.);
#1394=B_SPLINE_CURVE_WITH_KNOTS('',3,(#18039,#18040,#18041,#18042,#18043,
#18044,#18045,#18046,#18047,#18048,#18049,#18050,#18051,#18052,#18053,#18054,
#18055,#18056,#18057,#18058,#18059,#18060,#18061,#18062,#18063,#18064,#18065,
#18066,#18067,#18068,#18069,#18070,#18071,#18072,#18073,#18074,#18075,#18076,
#18077,#18078,#18079,#18080,#18081,#18082,#18083,#18084,#18085,#18086,#18087,
#18088,#18089,#18090,#18091,#18092,#18093,#18094,#18095,#18096,#18097,#18098,
#18099,#18100,#18101,#18102,#18103,#18104,#18105,#18106,#18107,#18108,#18109,
#18110,#18111,#18112,#18113,#18114,#18115,#18116,#18117,#18118,#18119,#18120,
#18121,#18122,#18123,#18124,#18125,#18126,#18127,#18128,#18129,#18130,#18131,
#18132,#18133,#18134,#18135,#18136,#18137,#18138,#18139,#18140,#18141,#18142,
#18143,#18144),.UNSPECIFIED.,.F.,.F.,(4,2,2,2,2,2,2,2,2,2,2,2,2,2,2,2,2,
2,2,2,2,2,2,2,2,2,2,2,2,2,2,2,2,2,2,2,2,2,2,2,2,2,2,2,2,2,2,2,2,2,2,2,4),
(-12.994627603384,-12.9875915521804,-12.9782754205316,-12.91699009307,-12.8731839129498,
-12.8557803975354,-12.8411540685734,-12.8227464552579,-12.7725470591221,
-12.7193211253437,-12.7007430540061,-12.686661419049,-12.6785554299798,
-12.6716500633205,-12.6589777049455,-12.5974421893282,-12.5499643410219,
-12.5317837785489,-12.5189811364405,-12.5053727543902,-12.4824936301464,
-12.4029450770898,-12.3819658998937,-12.366872420079,-12.3588855294487,
-12.3510968527962,-12.3383610505868,-12.2890655093762,-12.2464093533266,
-12.2175336782031,-12.2023791798903,-12.1889491752564,-12.1713159235955,
-12.1010906625992,-12.0721209918708,-12.0533384615127,-12.0443296945605,
-12.0365996637125,-12.024361864911,-11.9695325441213,-11.9302485028225,
-11.9028319644802,-11.8879963913662,-11.874653921784,-11.8565653989144,
-11.7774418205882,-11.7521961895244,-11.7349780097399,-11.7263341382877,
-11.7186941679461,-11.7064021195052,-11.654545056237,-11.6209589861144),
 .UNSPECIFIED.);
#1395=B_SPLINE_CURVE_WITH_KNOTS('',3,(#18192,#18193,#18194,#18195,#18196,
#18197,#18198,#18199,#18200,#18201,#18202,#18203,#18204,#18205),
 .UNSPECIFIED.,.F.,.F.,(4,2,2,2,2,2,4),(-0.00536726278181953,-2.59148391548031E-9,
0.103199421735768,0.207237881907438,0.325153852544771,0.397240462561985,
0.468984198664975),.UNSPECIFIED.);
#1396=B_SPLINE_CURVE_WITH_KNOTS('',3,(#18207,#18208,#18209,#18210,#18211,
#18212,#18213,#18214,#18215),.UNSPECIFIED.,.F.,.F.,(4,1,1,1,1,1,4),(-0.0350009593777651,
-0.0280198960523448,-0.0168045420304008,-0.00558918800845676,0.00562616601348723,
0.0280568740573752,0.0350536102859934),.UNSPECIFIED.);
#1397=B_SPLINE_CURVE_WITH_KNOTS('',3,(#18217,#18218,#18219,#18220,#18221,
#18222,#18223,#18224,#18225,#18226,#18227,#18228,#18229,#18230),
 .UNSPECIFIED.,.F.,.F.,(4,2,2,2,2,2,4),(0.,0.0545964532303548,0.109457297997855,
0.199283875927555,0.278528214008273,0.35702335445668,0.361102531747097),
 .UNSPECIFIED.);
#1398=B_SPLINE_CURVE_WITH_KNOTS('',3,(#18241,#18242,#18243,#18244,#18245,
#18246,#18247,#18248,#18249,#18250,#18251,#18252,#18253,#18254,#18255,#18256,
#18257,#18258,#18259,#18260,#18261,#18262,#18263,#18264,#18265,#18266,#18267,
#18268,#18269,#18270,#18271,#18272,#18273,#18274,#18275,#18276,#18277,#18278,
#18279,#18280,#18281,#18282,#18283,#18284,#18285,#18286,#18287,#18288,#18289),
 .UNSPECIFIED.,.F.,.F.,(4,3,3,3,3,3,3,3,3,3,3,3,3,3,3,3,4),(-0.0350029182876339,
-0.0326784274410288,-0.0303491617466868,-0.0280198960523449,-0.0254680708026916,
-0.0229201060834388,-0.020374904247847,-0.017833637297367,-0.0168045420304009,
-0.0144744225215027,-0.0121456147918491,-0.00981763946125116,-0.00748894401297814,
-0.0055891880084569,-0.00301831184103368,-0.00044459753078153,-5.93799746765259E-12),
 .UNSPECIFIED.);
#1399=B_SPLINE_CURVE_WITH_KNOTS('',3,(#18292,#18293,#18294,#18295,#18296,
#18297,#18298),.UNSPECIFIED.,.F.,.F.,(4,3,4),(-0.0490510097259757,0.,0.0490510097259755),
 .UNSPECIFIED.);
#1400=B_SPLINE_CURVE_WITH_KNOTS('',3,(#18300,#18301,#18302,#18303,#18304,
#18305),.UNSPECIFIED.,.F.,.F.,(4,2,4),(-0.954074778386005,-0.905023768660029,
-0.855972758934053),.UNSPECIFIED.);
#1401=B_SPLINE_CURVE_WITH_KNOTS('',3,(#18308,#18309,#18310,#18311,#18312,
#18313,#18314,#18315,#18316,#18317,#18318,#18319,#18320,#18321,#18322,#18323,
#18324,#18325,#18326,#18327,#18328,#18329,#18330,#18331,#18332,#18333,#18334,
#18335,#18336,#18337,#18338,#18339,#18340,#18341,#18342,#18343,#18344,#18345,
#18346,#18347,#18348,#18349,#18350,#18351,#18352,#18353,#18354,#18355,#18356),
 .UNSPECIFIED.,.F.,.F.,(4,3,3,3,3,3,3,3,3,3,3,3,3,3,3,3,4),(0.,0.00256903263786249,
0.00514025172138199,0.00562616601348712,0.0081513990320383,0.0106763832495211,
0.0132007965397256,0.0157247404553983,0.0168415200354311,0.0191777542451066,
0.0215147787392673,0.0238521408034104,0.026192082316959,0.0280568740573752,
0.030597682690626,0.033145701984153,0.0350439206609343),.UNSPECIFIED.);
#1402=B_SPLINE_CURVE_WITH_KNOTS('',3,(#18411,#18412,#18413,#18414,#18415,
#18416,#18417,#18418,#18419,#18420,#18421,#18422,#18423,#18424),
 .UNSPECIFIED.,.F.,.F.,(4,2,2,2,2,2,4),(-0.361103617303379,-0.357017748906342,
-0.278455831096292,-0.199256530150916,-0.109493107705783,-0.0546164016226888,
-6.26706830986201E-7),.UNSPECIFIED.);
#1403=B_SPLINE_CURVE_WITH_KNOTS('',3,(#18426,#18427,#18428,#18429,#18430,
#18431,#18432,#18433,#18434,#18435,#18436,#18437,#18438,#18439),
 .UNSPECIFIED.,.F.,.F.,(4,2,2,2,2,2,4),(-0.469007914525735,-0.397274254527166,
-0.325193332432218,-0.207246009609002,-0.103181568409207,0.,0.00535948636125596),
 .UNSPECIFIED.);
#1404=B_SPLINE_CURVE_WITH_KNOTS('',3,(#18628,#18629,#18630,#18631,#18632,
#18633,#18634,#18635,#18636,#18637,#18638,#18639,#18640,#18641,#18642,#18643,
#18644,#18645,#18646,#18647,#18648,#18649,#18650,#18651,#18652,#18653,#18654,
#18655,#18656,#18657,#18658,#18659,#18660,#18661,#18662,#18663,#18664,#18665,
#18666,#18667,#18668,#18669,#18670,#18671,#18672,#18673,#18674,#18675,#18676,
#18677,#18678,#18679,#18680,#18681,#18682,#18683,#18684,#18685,#18686,#18687,
#18688,#18689,#18690,#18691,#18692,#18693,#18694,#18695,#18696,#18697,#18698,
#18699,#18700,#18701,#18702,#18703,#18704,#18705,#18706,#18707,#18708,#18709,
#18710,#18711,#18712),.UNSPECIFIED.,.F.,.F.,(4,3,3,3,3,3,3,3,3,3,3,3,3,
3,3,3,3,3,3,3,3,3,3,3,3,3,3,3,4),(5.93772547493953E-5,0.0374260888262869,
0.0738564267296499,0.110770159938098,0.147683893146547,0.154011688621638,
0.189882099992678,0.225711180046048,0.260784282188391,0.292370020163279,
0.299381408876867,0.333941591811059,0.367613151733489,0.401093479558722,
0.407459990826463,0.436280771759322,0.441113261645755,0.474765163706684,
0.50871732282195,0.542418769600373,0.567449717218624,0.575264939175507,
0.60833260900008,0.640763136698678,0.657717726095142,0.662787221699447,
0.694639312545765,0.725626255150186,0.744397949170602),.UNSPECIFIED.);
#1405=B_SPLINE_CURVE_WITH_KNOTS('',3,(#18714,#18715,#18716,#18717,#18718,
#18719,#18720,#18721,#18722,#18723,#18724,#18725,#18726,#18727,#18728,#18729,
#18730,#18731,#18732,#18733,#18734,#18735,#18736,#18737,#18738,#18739,#18740,
#18741,#18742,#18743,#18744,#18745,#18746,#18747,#18748,#18749,#18750,#18751,
#18752,#18753,#18754,#18755,#18756,#18757,#18758,#18759,#18760,#18761,#18762,
#18763,#18764,#18765,#18766,#18767,#18768,#18769,#18770,#18771,#18772,#18773,
#18774,#18775,#18776,#18777,#18778,#18779,#18780,#18781,#18782,#18783,#18784,
#18785,#18786,#18787,#18788,#18789,#18790,#18791,#18792,#18793,#18794,#18795,
#18796,#18797,#18798,#18799,#18800,#18801,#18802,#18803,#18804),
 .UNSPECIFIED.,.F.,.F.,(4,3,3,3,3,3,3,3,3,3,3,3,3,3,3,3,3,3,3,3,3,3,3,3,
3,3,3,3,3,3,4),(0.,0.0309970440507718,0.0619955277647955,0.0939113023789225,
0.122434839440515,0.12758455026797,0.132227190796814,0.164899763317829,
0.198101502938401,0.231586044786447,0.259311605376256,0.263977965982227,
0.298334414351843,0.333236562478584,0.368138710605325,0.370114527877473,
0.398052464733428,0.403189970392264,0.437098301742969,0.471632442026652,
0.506863545933039,0.53577203760693,0.541093903690208,0.546417846440992,
0.582336732445268,0.618540903512682,0.634760608889732,0.641019432752641,
0.67784978911133,0.714258333683681,0.74127076840638),.UNSPECIFIED.);
#1406=B_SPLINE_CURVE_WITH_KNOTS('',3,(#18805,#18806,#18807,#18808),
 .UNSPECIFIED.,.F.,.F.,(4,4),(-0.0121139156679117,0.),.UNSPECIFIED.);
#1407=B_SPLINE_CURVE_WITH_KNOTS('',3,(#18994,#18995,#18996,#18997,#18998,
#18999,#19000,#19001,#19002,#19003,#19004,#19005,#19006,#19007,#19008,#19009,
#19010,#19011,#19012,#19013,#19014,#19015,#19016,#19017,#19018,#19019,#19020,
#19021,#19022,#19023,#19024,#19025,#19026,#19027,#19028,#19029,#19030,#19031,
#19032,#19033,#19034,#19035,#19036,#19037,#19038,#19039,#19040,#19041,#19042,
#19043,#19044,#19045,#19046,#19047,#19048,#19049,#19050,#19051,#19052,#19053,
#19054,#19055,#19056,#19057,#19058,#19059,#19060,#19061,#19062,#19063,#19064,
#19065,#19066,#19067,#19068,#19069,#19070,#19071,#19072,#19073,#19074,#19075,
#19076,#19077,#19078,#19079,#19080,#19081,#19082,#19083,#19084,#19085,#19086,
#19087,#19088,#19089,#19090),.UNSPECIFIED.,.F.,.F.,(4,3,3,3,3,3,3,3,3,3,
3,3,3,3,3,3,3,3,3,3,3,3,3,3,3,3,3,3,3,3,3,3,4),(0.,0.0309970440507677,0.0619181010064114,
0.0937144809078779,0.110912695544682,0.122435055735921,0.127584942037278,
0.132227280497855,0.1648998786022,0.198101629608467,0.231586168644273,0.259311708386001,
0.263978079994448,0.298334530993182,0.333236654183239,0.368138777373297,
0.370114527877469,0.393311792910526,0.398370229703331,0.403189968677661,
0.437098316226467,0.471632477527816,0.506863596722405,0.535772077628709,
0.541093944718474,0.546417849114959,0.582336753940169,0.618540921884149,
0.634760639680576,0.641019471053442,0.677849826923293,0.714258330886494,
0.741270768406381),.UNSPECIFIED.);
#1408=B_SPLINE_CURVE_WITH_KNOTS('',3,(#19091,#19092,#19093,#19094),
 .UNSPECIFIED.,.F.,.F.,(4,4),(0.,0.0121134590555018),.UNSPECIFIED.);
#1409=B_SPLINE_CURVE_WITH_KNOTS('',3,(#19095,#19096,#19097,#19098,#19099,
#19100,#19101,#19102,#19103,#19104,#19105,#19106,#19107,#19108,#19109,#19110,
#19111,#19112,#19113,#19114,#19115,#19116,#19117,#19118,#19119,#19120,#19121,
#19122,#19123,#19124,#19125,#19126,#19127,#19128,#19129,#19130,#19131,#19132,
#19133,#19134,#19135,#19136,#19137,#19138,#19139,#19140,#19141,#19142,#19143,
#19144,#19145,#19146,#19147,#19148,#19149,#19150,#19151,#19152,#19153,#19154,
#19155,#19156,#19157,#19158,#19159,#19160,#19161,#19162,#19163,#19164,#19165,
#19166,#19167,#19168,#19169,#19170,#19171,#19172,#19173,#19174,#19175,#19176,
#19177,#19178,#19179,#19180,#19181,#19182,#19183,#19184,#19185,#19186,#19187,
#19188),.UNSPECIFIED.,.F.,.F.,(4,3,3,3,3,3,3,3,3,3,3,3,3,3,3,3,3,3,3,3,
3,3,3,3,3,3,3,3,3,3,3,4),(0.,0.0374260888263008,0.0738564290320547,0.110770162397625,
0.147683895763195,0.154011692627707,0.189882104065088,0.225711192227168,
0.260784326226137,0.292370154409116,0.299381403642943,0.333917720960345,
0.36795450999486,0.401093586298063,0.407459990826479,0.428518613222987,
0.434552801562352,0.439572347501266,0.441113258225818,0.474677870938634,
0.508628197894967,0.54247978601399,0.558802088782934,0.568708698403076,
0.576616421709766,0.609674167629691,0.642088946178112,0.657717694151321,
0.662787189531987,0.694639229192994,0.725626103462853,0.744397949170599),
 .UNSPECIFIED.);
#1410=B_SPLINE_CURVE_WITH_KNOTS('',3,(#19197,#19198,#19199,#19200,#19201,
#19202,#19203,#19204,#19205,#19206,#19207,#19208,#19209,#19210,#19211,#19212,
#19213,#19214,#19215,#19216,#19217,#19218,#19219,#19220,#19221,#19222,#19223,
#19224,#19225,#19226,#19227,#19228,#19229,#19230,#19231,#19232,#19233,#19234,
#19235,#19236,#19237,#19238,#19239,#19240,#19241,#19242,#19243,#19244,#19245,
#19246,#19247,#19248,#19249,#19250,#19251,#19252,#19253,#19254,#19255,#19256,
#19257,#19258,#19259,#19260,#19261,#19262,#19263,#19264,#19265,#19266,#19267,
#19268,#19269,#19270,#19271,#19272,#19273,#19274),.UNSPECIFIED.,.F.,.F.,
(4,2,2,2,2,2,2,2,2,2,2,2,2,2,2,2,2,2,2,2,2,2,2,2,2,2,2,2,2,2,2,2,2,2,2,
2,2,2,4),(-0.953586899306873,-0.946224083901339,-0.939681248602814,-0.933646614330381,
-0.924287213729251,-0.88833783922987,-0.804035161913967,-0.788327368237523,
-0.778740839088327,-0.768154224228326,-0.752801038121388,-0.691121741172027,
-0.635518435315854,-0.624462413541429,-0.618082999395715,-0.611911752838689,
-0.60200076655729,-0.589720784215698,-0.562242711762516,-0.486315971197755,
-0.46886052902349,-0.457800984209137,-0.447137732981836,-0.431855739492939,
-0.37573088153337,-0.313542424627404,-0.30302882313823,-0.296702133009702,
-0.290241676772455,-0.279315169359953,-0.265353516421564,-0.230988909071748,
-0.168154569303192,-0.151167359383941,-0.140141098841724,-0.129305786003328,
-0.11338295845748,-0.0538958793772908,-0.00526464879914939),
 .UNSPECIFIED.);
#1411=B_SPLINE_CURVE_WITH_KNOTS('',3,(#19277,#19278,#19279,#19280,#19281,
#19282,#19283,#19284,#19285,#19286,#19287,#19288,#19289,#19290,#19291,#19292,
#19293,#19294,#19295,#19296,#19297,#19298,#19299,#19300,#19301,#19302,#19303,
#19304,#19305,#19306,#19307,#19308,#19309,#19310,#19311,#19312,#19313,#19314,
#19315,#19316,#19317,#19318,#19319,#19320,#19321,#19322,#19323,#19324,#19325,
#19326,#19327,#19328,#19329,#19330,#19331,#19332,#19333,#19334),
 .UNSPECIFIED.,.F.,.F.,(4,3,3,3,3,3,3,3,3,3,3,3,3,3,3,3,3,3,3,4),(-94.2338387311155,
-94.1386227061935,-94.0434628204143,-93.9483368145334,-93.853196460553,
-93.7580426009854,-93.6628550280585,-93.567613507008,-93.4722330639492,
-93.376774672444,-93.2811517509658,-93.2410420546399,-93.1487193791218,
-93.0565224071019,-92.9644252665555,-92.8724021885971,-92.7804134444312,
-92.6884474321017,-92.5964417156794,-92.5246180830661),.UNSPECIFIED.);
#1412=B_SPLINE_CURVE_WITH_KNOTS('',3,(#19339,#19340,#19341,#19342,#19343,
#19344,#19345,#19346,#19347,#19348,#19349,#19350,#19351,#19352,#19353,#19354,
#19355,#19356,#19357,#19358,#19359,#19360,#19361,#19362,#19363,#19364,#19365,
#19366,#19367,#19368,#19369,#19370,#19371,#19372,#19373,#19374,#19375,#19376,
#19377,#19378,#19379,#19380,#19381,#19382,#19383,#19384,#19385,#19386,#19387,
#19388,#19389,#19390,#19391,#19392,#19393,#19394,#19395,#19396,#19397,#19398,
#19399,#19400,#19401,#19402,#19403,#19404,#19405,#19406,#19407,#19408,#19409,
#19410,#19411,#19412,#19413,#19414,#19415,#19416,#19417,#19418,#19419,#19420,
#19421,#19422,#19423,#19424,#19425,#19426,#19427,#19428,#19429,#19430,#19431,
#19432,#19433,#19434,#19435,#19436,#19437,#19438,#19439,#19440,#19441,#19442,
#19443,#19444,#19445,#19446,#19447,#19448,#19449,#19450,#19451,#19452,#19453,
#19454,#19455,#19456,#19457,#19458,#19459,#19460,#19461,#19462,#19463,#19464,
#19465,#19466,#19467,#19468,#19469,#19470,#19471,#19472,#19473,#19474,#19475,
#19476,#19477,#19478,#19479,#19480,#19481,#19482,#19483,#19484,#19485,#19486,
#19487,#19488,#19489,#19490,#19491,#19492,#19493,#19494,#19495,#19496,#19497,
#19498,#19499,#19500,#19501,#19502,#19503,#19504,#19505,#19506),
 .UNSPECIFIED.,.F.,.F.,(4,2,2,2,2,2,2,2,2,2,2,2,2,2,2,2,2,2,2,2,2,2,2,2,
2,2,2,2,2,2,2,2,2,2,2,2,2,2,2,2,2,2,2,2,2,2,2,2,2,2,2,2,2,2,2,2,2,2,2,2,
2,2,2,2,2,2,2,2,2,2,2,2,2,2,2,2,2,2,2,2,2,2,2,4),(-2.98314948647837,-2.92931927299001,
-2.87847831664238,-2.86854692686803,-2.86238048863821,-2.85598188384405,
-2.84491835823975,-2.78906969762543,-2.72775918925124,-2.71234213768023,
-2.70169927312789,-2.69075927697716,-2.67371484620561,-2.60849645012846,
-2.55783247712985,-2.54788253120033,-2.54171277534183,-2.53531903720203,
-2.52428009071603,-2.46776648675201,-2.42715250362434,-2.40830069600736,
-2.39233125418358,-2.38158948252091,-2.37076866644709,-2.35436708268367,
-2.28314135391068,-2.25155038995474,-2.23824842378604,-2.22773649064595,
-2.22145110781181,-2.21594582391548,-2.20632739871659,-2.16701154076078,
-2.11294395468491,-2.0912376827486,-2.07353264494282,-2.06246402564764,
-2.05201402271332,-2.0394863417041,-2.0061953134929,-1.99990582558898,-1.94050245591194,
-1.92231800668791,-1.90911550001101,-1.90229003981063,-1.89634126079205,
-1.88902652801476,-1.86895400933939,-1.80951506282857,-1.77897954822343,
-1.75649112348816,-1.74453409286566,-1.73422264512113,-1.72122725251755,
-1.69233732141656,-1.64649274907083,-1.59931226565268,-1.58749550650159,
-1.58094516716533,-1.57487942726118,-1.5654739075449,-1.52927851683261,
-1.44595504899421,-1.43008910319921,-1.42043269512404,-1.4097841233922,
-1.39436252007387,-1.33286583781343,-1.27719596698061,-1.26611968641952,
-1.25971350417248,-1.25352405459038,-1.24354070919542,-1.23113688245437,
-1.20315529593337,-1.12441168013372,-1.10911634905808,-1.09858349711662,
-1.08760467199154,-1.07043920126136,-1.02023819202142,-0.957986996023974,
-0.953586899306873),.UNSPECIFIED.);
#1413=B_SPLINE_CURVE_WITH_KNOTS('',3,(#19508,#19509,#19510,#19511,#19512,
#19513,#19514,#19515,#19516,#19517,#19518,#19519,#19520,#19521,#19522,#19523,
#19524,#19525,#19526,#19527,#19528,#19529,#19530,#19531,#19532,#19533,#19534,
#19535,#19536,#19537,#19538,#19539,#19540,#19541,#19542,#19543,#19544,#19545,
#19546,#19547,#19548,#19549,#19550,#19551,#19552,#19553),.UNSPECIFIED.,
 .F.,.F.,(4,3,3,3,3,3,3,3,3,3,3,3,3,3,3,4),(-92.5246180830661,-92.4325102353362,
-92.3402421939541,-92.2482453781643,-92.1550137134133,-92.0619070601935,
-91.9688980138682,-91.8759565736399,-91.78305006345,-91.6901538610218,-91.5972433592587,
-91.5042366896818,-91.4111786089953,-91.3179720140179,-91.2554487016887,
-91.106186954104),.UNSPECIFIED.);
#1414=B_SPLINE_CURVE_WITH_KNOTS('',3,(#19554,#19555,#19556,#19557,#19558,
#19559,#19560,#19561,#19562),.UNSPECIFIED.,.F.,.F.,(4,1,1,1,1,1,4),(-91.1061804086756,
-90.2626520252132,-89.2698553487376,-88.277058672262,-87.2842619957864,
-86.2914653193108,-86.2406734486321),.UNSPECIFIED.);
#1415=B_SPLINE_CURVE_WITH_KNOTS('',3,(#19568,#19569,#19570,#19571,#19572,
#19573,#19574,#19575,#19576,#19577,#19578,#19579,#19580,#19581,#19582,#19583,
#19584,#19585,#19586,#19587,#19588,#19589,#19590,#19591,#19592,#19593,#19594,
#19595,#19596,#19597,#19598,#19599,#19600,#19601,#19602,#19603,#19604,#19605,
#19606,#19607,#19608,#19609,#19610,#19611,#19612,#19613,#19614,#19615,#19616,
#19617,#19618,#19619,#19620,#19621,#19622,#19623,#19624,#19625,#19626,#19627,
#19628,#19629,#19630,#19631,#19632,#19633,#19634,#19635,#19636,#19637,#19638,
#19639,#19640,#19641,#19642,#19643,#19644,#19645,#19646,#19647,#19648,#19649,
#19650,#19651,#19652,#19653,#19654,#19655,#19656,#19657,#19658,#19659,#19660,
#19661,#19662,#19663,#19664,#19665,#19666,#19667,#19668,#19669,#19670,#19671,
#19672,#19673,#19674,#19675,#19676,#19677,#19678,#19679,#19680,#19681,#19682,
#19683,#19684,#19685,#19686,#19687,#19688,#19689,#19690,#19691,#19692,#19693,
#19694,#19695),.UNSPECIFIED.,.F.,.F.,(4,2,2,2,2,2,2,2,2,2,2,2,2,2,2,2,2,
2,2,2,2,2,2,2,2,2,2,2,2,2,2,2,2,2,2,2,2,2,2,2,2,2,2,2,2,2,2,2,2,2,2,2,2,
2,2,2,2,2,2,2,2,2,2,4),(-1.57226653739125,-1.5335777974379,-1.51749976800245,
-1.50781260533011,-1.49720443964807,-1.48199362716857,-1.4271100079384,
-1.36376233553656,-1.35299538353744,-1.34665765102371,-1.34044105870802,
-1.33026081848513,-1.28036678994184,-1.21482587221898,-1.19781359925106,
-1.18687887704712,-1.17623012667664,-1.16078436208362,-1.09877281757955,
-1.04367999968674,-1.03258103848034,-1.02617467754542,-1.02001319481398,
-1.01010791778992,-0.958953801785455,-0.894272784649096,-0.877190705715183,
-0.866242485531937,-0.855602583965498,-0.840209857332201,-0.778575631347056,
-0.722936048969459,-0.711861685957521,-0.70546020493503,-0.699294513098806,
-0.689369054767423,-0.677054035431794,-0.649392216624609,-0.572613580933394,
-0.555994727226221,-0.545133285484477,-0.53442622969633,-0.518652195275346,
-0.459429796640774,-0.402070705637716,-0.391076790872994,-0.384691797229376,
-0.378513281994944,-0.368523491494722,-0.356101632547016,-0.328031571970327,
-0.24906421527631,-0.233758461195957,-0.223238986692471,-0.212293433018225,
-0.195226494574182,-0.145648423230977,-0.0814618760384713,-0.070400689902343,
-0.0640018345987939,-0.0578339732759233,-0.0513639077985467,-0.0362287903919722,
-0.000931521656303621),.UNSPECIFIED.);
#1416=B_SPLINE_CURVE_WITH_KNOTS('',3,(#19696,#19697,#19698,#19699,#19700,
#19701,#19702,#19703,#19704,#19705,#19706,#19707,#19708,#19709,#19710,#19711,
#19712,#19713,#19714,#19715,#19716,#19717,#19718,#19719,#19720,#19721,#19722,
#19723,#19724,#19725,#19726,#19727,#19728,#19729,#19730,#19731,#19732,#19733),
 .UNSPECIFIED.,.F.,.F.,(4,2,2,2,2,2,2,2,2,2,2,2,2,2,2,2,2,2,4),(-3.44144283943813,
-3.36915521246843,-3.35372024630458,-3.34307352431673,-3.33213640148464,
-3.31511101176518,-3.24965355552941,-3.19915704516472,-3.18922333268155,
-3.18305637047153,-3.17665726842006,-3.1655942456309,-3.10972609818714,
-3.04842654583021,-3.03301632354937,-3.02237360197422,-3.01142989848601,
-2.99437110190186,-2.98314948647837),.UNSPECIFIED.);
#1417=B_SPLINE_CURVE_WITH_KNOTS('',3,(#19735,#19736,#19737,#19738,#19739),
 .UNSPECIFIED.,.F.,.F.,(4,1,4),(-86.2406734486321,-85.2986686428353,-84.8230031757796),
 .UNSPECIFIED.);
#1418=B_SPLINE_CURVE_WITH_KNOTS('',3,(#19740,#19741,#19742,#19743,#19744,
#19745,#19746,#19747,#19748,#19749,#19750,#19751,#19752,#19753,#19754,#19755,
#19756,#19757,#19758,#19759,#19760,#19761,#19762,#19763,#19764,#19765,#19766,
#19767,#19768,#19769,#19770,#19771,#19772,#19773,#19774,#19775,#19776,#19777,
#19778,#19779,#19780,#19781,#19782,#19783,#19784,#19785,#19786,#19787,#19788,
#19789,#19790,#19791,#19792,#19793,#19794,#19795,#19796,#19797,#19798,#19799,
#19800,#19801,#19802,#19803,#19804,#19805,#19806,#19807,#19808,#19809,#19810,
#19811,#19812,#19813,#19814,#19815,#19816,#19817,#19818,#19819,#19820,#19821,
#19822,#19823,#19824,#19825,#19826,#19827,#19828,#19829,#19830,#19831,#19832,
#19833,#19834,#19835,#19836,#19837,#19838,#19839,#19840,#19841,#19842,#19843,
#19844,#19845,#19846,#19847,#19848,#19849,#19850,#19851,#19852,#19853,#19854,
#19855,#19856,#19857,#19858,#19859,#19860,#19861,#19862,#19863),
 .UNSPECIFIED.,.F.,.F.,(4,2,2,2,2,2,2,2,2,2,2,2,2,2,2,2,2,2,2,2,2,2,2,2,
2,2,2,2,2,2,2,2,2,2,2,2,2,2,2,2,2,2,2,2,2,2,2,2,2,2,2,2,2,2,2,2,2,2,2,2,
2,4),(-4.05949121043388,-4.05121437145667,-4.04065847954402,-4.02381103819477,
-3.95897828953223,-3.90811934396657,-3.89820260742545,-3.8920396257056,
-3.88563807260872,-3.87455861457586,-3.81920431913373,-3.75742003728717,
-3.74201743687854,-3.7313777449435,-3.72043543181097,-3.70337527512879,
-3.63838157000884,-3.58749127890204,-3.5775671792347,-3.57140291795658,
-3.56500278009261,-3.55393200139329,-3.49833852441203,-3.4368258288365,
-3.42140106480513,-3.41075658377407,-3.39981778691892,-3.38278102810115,
-3.31749947334804,-3.26754902845121,-3.25726826635629,-3.25103138547184,
-3.24471713356767,-3.23406214171634,-3.17336971297882,-3.13494613533587,
-3.11665137224682,-3.10103194361361,-3.09035352395009,-3.07946036874197,
-3.06266587013177,-2.99480056759295,-2.94745285384507,-2.93689327516753,
-2.93059879932187,-2.92434353568057,-2.91397336918307,-2.85079466441326,
-2.81356101937502,-2.79557917663882,-2.78015734987967,-2.76951317962702,
-2.75857335392659,-2.74153221996127,-2.67627961911833,-2.62565067878737,
-2.61570117934235,-2.60953128798207,-2.60313694386948,-2.59209545593267,
-2.53566520876919,-2.48818497945327),.UNSPECIFIED.);
#1419=B_SPLINE_CURVE_WITH_KNOTS('',3,(#19868,#19869,#19870,#19871,#19872,
#19873,#19874,#19875,#19876,#19877,#19878,#19879,#19880,#19881,#19882,#19883,
#19884,#19885,#19886,#19887,#19888,#19889,#19890,#19891,#19892,#19893,#19894,
#19895,#19896,#19897,#19898,#19899,#19900,#19901,#19902,#19903,#19904,#19905,
#19906,#19907,#19908,#19909,#19910,#19911,#19912,#19913,#19914,#19915,#19916,
#19917,#19918,#19919,#19920,#19921,#19922,#19923,#19924,#19925,#19926,#19927,
#19928,#19929,#19930,#19931,#19932,#19933,#19934,#19935,#19936,#19937,#19938,
#19939,#19940,#19941,#19942,#19943,#19944,#19945,#19946,#19947,#19948,#19949,
#19950,#19951,#19952,#19953,#19954,#19955,#19956,#19957,#19958,#19959,#19960,
#19961,#19962,#19963,#19964,#19965,#19966,#19967,#19968,#19969,#19970,#19971,
#19972,#19973,#19974,#19975,#19976,#19977,#19978,#19979,#19980,#19981,#19982,
#19983,#19984,#19985,#19986,#19987,#19988,#19989,#19990,#19991,#19992,#19993,
#19994,#19995,#19996,#19997,#19998,#19999,#20000,#20001,#20002,#20003,#20004,
#20005,#20006,#20007,#20008,#20009,#20010,#20011,#20012,#20013,#20014,#20015,
#20016,#20017,#20018,#20019,#20020,#20021,#20022,#20023,#20024,#20025,#20026,
#20027,#20028,#20029,#20030,#20031,#20032,#20033,#20034,#20035,#20036,#20037,
#20038,#20039,#20040,#20041),.UNSPECIFIED.,.F.,.F.,(4,2,2,2,2,2,2,2,2,2,
2,2,2,2,2,2,2,2,2,2,2,2,2,2,2,2,2,2,2,2,2,2,2,2,2,2,2,2,2,2,2,2,2,2,2,2,
2,2,2,2,2,2,2,2,2,2,2,2,2,2,2,2,2,2,2,2,2,2,2,2,2,2,2,2,2,2,2,2,2,2,2,2,
2,2,2,2,4),(-3.60148803627134,-3.59726790795439,-3.59098685437188,-3.58471907313518,
-3.57428766404847,-3.51164348509371,-3.45559099116675,-3.44034678171266,
-3.42973359074539,-3.41875011562731,-3.40147579935169,-3.34043366880226,
-3.30310540362232,-3.28205654415774,-3.27398152357135,-3.26810771974208,
-3.26090656586411,-3.2456415178696,-3.18703553787276,-3.13855425810496,
-3.1216363120744,-3.11072040881662,-3.10018385387515,-3.0847683875459,-3.00651772233112,
-2.97812444519445,-2.96561919642675,-2.95558062126107,-2.94939320865812,
-2.94302219732592,-2.93209232466705,-2.87403556224324,-2.83428541792364,
-2.81565086864161,-2.79981791455114,-2.78910164548746,-2.77825485553291,
-2.76170816630454,-2.69166204680768,-2.65949146606953,-2.64605245758614,
-2.63546067061529,-2.6291595684875,-2.62291078291482,-2.61257177018778,
-2.54912091334469,-2.5120150754806,-2.49406737179312,-2.47866721537971,
-2.46802690006783,-2.45708201518327,-2.4400135557156,-2.37510334330683,
-2.32419385495604,-2.31423984884152,-2.30806912114555,-2.30167618897554,
-2.29064106146257,-2.22197476329415,-2.18871569735013,-2.16492129885298,
-2.15273109663306,-2.1424291067809,-2.12971584634897,-2.10273105378269,
-2.02998606678719,-2.0016293028606,-1.99260960515907,-1.98667066811743,
-1.97999954768792,-1.96758725489158,-1.95090337602745,-1.90211662187695,
-1.85194585632104,-1.8369121508399,-1.82643866908472,-1.81542316901591,
-1.79798287416363,-1.74547920414441,-1.68411033096761,-1.67352430836737,
-1.66722415648816,-1.66097373936419,-1.65062802104306,-1.63760890563595,
-1.60717731235625,-1.57226653739125),.UNSPECIFIED.);
#1420=B_SPLINE_CURVE_WITH_KNOTS('',3,(#20042,#20043,#20044,#20045,#20046,
#20047,#20048,#20049,#20050,#20051,#20052,#20053,#20054,#20055,#20056,#20057,
#20058,#20059,#20060,#20061,#20062,#20063,#20064,#20065,#20066,#20067,#20068,
#20069,#20070,#20071,#20072,#20073,#20074,#20075,#20076,#20077,#20078,#20079,
#20080,#20081,#20082,#20083,#20084,#20085,#20086,#20087,#20088,#20089,#20090,
#20091,#20092,#20093,#20094,#20095,#20096,#20097,#20098,#20099,#20100,#20101,
#20102,#20103,#20104,#20105,#20106,#20107,#20108,#20109,#20110,#20111,#20112,
#20113,#20114,#20115,#20116,#20117,#20118,#20119,#20120,#20121,#20122,#20123,
#20124,#20125,#20126,#20127,#20128,#20129,#20130,#20131,#20132,#20133,#20134,
#20135,#20136,#20137,#20138,#20139,#20140,#20141,#20142,#20143,#20144,#20145,
#20146,#20147,#20148,#20149,#20150,#20151,#20152,#20153,#20154,#20155,#20156,
#20157,#20158,#20159,#20160,#20161,#20162,#20163,#20164,#20165,#20166,#20167,
#20168,#20169,#20170,#20171,#20172,#20173,#20174,#20175,#20176,#20177,#20178,
#20179,#20180,#20181,#20182,#20183,#20184,#20185,#20186,#20187,#20188,#20189,
#20190,#20191,#20192,#20193,#20194,#20195,#20196,#20197,#20198,#20199,#20200,
#20201,#20202,#20203,#20204,#20205,#20206,#20207,#20208,#20209),
 .UNSPECIFIED.,.F.,.F.,(4,2,2,2,2,2,2,2,2,2,2,2,2,2,2,2,2,2,2,2,2,2,2,2,
2,2,2,2,2,2,2,2,2,2,2,2,2,2,2,2,2,2,2,2,2,2,2,2,2,2,2,2,2,2,2,2,2,2,2,2,
2,2,2,2,2,2,2,2,2,2,2,2,2,2,2,2,2,2,2,2,2,2,2,4),(-2.48818497945327,-2.47661569284377,
-2.46041249231985,-2.44962867574266,-2.43885292257533,-2.42269402150062,
-2.34963196044359,-2.31891957880817,-2.30583089242212,-2.29544489121947,
-2.28918621756621,-2.28289464564112,-2.27235029868863,-2.21067864367937,
-2.15559329660223,-2.13955930085061,-2.12880625929744,-2.11799874145444,
-2.10166705448592,-2.02990196306529,-1.98730851207629,-1.97573932437658,
-1.96923692158684,-1.96314080965402,-1.95357264272231,-1.91386818576171,
-1.83704171514185,-1.81996554507048,-1.80901875051122,-1.79837854665767,
-1.78298224522728,-1.76503910564669,-1.72795555566859,-1.66437608378914,
-1.6540447671092,-1.64779725241036,-1.64149351545674,-1.63089127738814,
-1.61743622842379,-1.58519570479033,-1.51535388396843,-1.49878885307633,
-1.48793790926569,-1.47722314628574,-1.46140326307786,-1.40103999361036,
-1.3450610657836,-1.33399883001431,-1.32760001200728,-1.32143274143006,
-1.31149835160373,-1.26082229040495,-1.19564760626722,-1.17860471563187,
-1.16766389105049,-1.15701870553694,-1.14159547110918,-1.1236100980696,
-1.08636972622046,-1.02311542409142,-1.01274592372879,-1.00649036762245,
-1.00019460847225,-0.989631608162483,-0.941721342655347,-0.874629750026393,
-0.857760383650131,-0.846852232066049,-0.836182940761279,-0.820621411802712,
-0.761154441683342,-0.703549270177194,-0.692574275383058,-0.686193266407756,
-0.680011710962549,-0.670006535853517,-0.657558990906142,-0.629389598384432,
-0.550666233097892,-0.535325340491625,-0.524799982685431,-0.513863175707245,
-0.496842297440668,-0.458703963070235),.UNSPECIFIED.);
#1421=B_SPLINE_CURVE_WITH_KNOTS('',3,(#20215,#20216,#20217,#20218,#20219,
#20220,#20221,#20222,#20223,#20224,#20225,#20226,#20227,#20228,#20229,#20230,
#20231,#20232,#20233,#20234,#20235,#20236,#20237,#20238,#20239,#20240,#20241,
#20242,#20243,#20244,#20245,#20246,#20247,#20248,#20249,#20250,#20251,#20252,
#20253,#20254,#20255,#20256,#20257,#20258,#20259,#20260,#20261,#20262,#20263,
#20264,#20265,#20266,#20267,#20268,#20269,#20270,#20271,#20272,#20273,#20274,
#20275,#20276,#20277,#20278,#20279,#20280,#20281,#20282,#20283,#20284,#20285,
#20286,#20287,#20288,#20289,#20290,#20291,#20292,#20293,#20294,#20295,#20296,
#20297,#20298,#20299,#20300,#20301,#20302,#20303,#20304,#20305,#20306,#20307,
#20308,#20309,#20310,#20311,#20312,#20313,#20314,#20315,#20316,#20317,#20318,
#20319,#20320,#20321,#20322,#20323,#20324,#20325,#20326,#20327,#20328,#20329,
#20330,#20331,#20332,#20333,#20334,#20335,#20336,#20337,#20338,#20339,#20340,
#20341,#20342,#20343,#20344,#20345,#20346,#20347,#20348),.UNSPECIFIED.,
 .F.,.F.,(4,2,2,2,2,2,2,2,2,2,2,2,2,2,2,2,2,2,2,2,2,2,2,2,2,2,2,2,2,2,2,
2,2,2,2,2,2,2,2,2,2,2,2,2,2,2,2,2,2,2,2,2,2,2,2,2,2,2,2,2,2,2,2,2,2,2,4),
(-1.57270504429441,-1.57198597895571,-1.53184015506289,-1.4744178950004,
-1.46342781057866,-1.45704342558984,-1.4508638651289,-1.44086999371776,
-1.42844156890585,-1.40034729366256,-1.32143087815656,-1.30611622816268,
-1.29559480540958,-1.28465062268848,-1.26759324916272,-1.21809184782572,
-1.15729158777298,-1.14419135132274,-1.13738539355418,-1.13142607440303,
-1.12265609486979,-1.09531100949502,-1.03125066260997,-0.997509615877714,
-0.98493246552515,-0.974472652709664,-0.963426589679085,-0.945834993848146,
-0.924318436015176,-0.871329842578893,-0.830426302826506,-0.820785203293156,
-0.815276889046202,-0.808998247382131,-0.798520016701879,-0.785277148103801,
-0.753931042657932,-0.682243191223101,-0.665904305115668,-0.655094053629165,
-0.64433973007818,-0.628306893505015,-0.574149269053255,-0.511174379321276,
-0.500769824530627,-0.494506480797386,-0.488217178586173,-0.477687892439614,
-0.428977275730074,-0.362775320398643,-0.345817247349719,-0.334891381242875,
-0.324232895492104,-0.308739200514757,-0.290643425545204,-0.252992014084021,
-0.190575699323686,-0.180106656871352,-0.173829923488554,-0.167554150248785,
-0.157090098128878,-0.109028173875831,-0.0418274175576785,-0.0252966452826552,
-0.0143328742967741,-0.00723065120931022,-0.000931044346426293),
 .UNSPECIFIED.);
#1422=B_SPLINE_CURVE_WITH_KNOTS('',3,(#20349,#20350,#20351,#20352,#20353,
#20354,#20355,#20356,#20357,#20358,#20359,#20360,#20361,#20362,#20363,#20364,
#20365,#20366,#20367,#20368,#20369,#20370,#20371,#20372,#20373,#20374,#20375,
#20376,#20377,#20378,#20379,#20380,#20381,#20382,#20383,#20384,#20385,#20386),
 .UNSPECIFIED.,.F.,.F.,(4,2,2,2,2,2,2,2,2,2,2,2,2,2,2,2,2,2,4),(-4.05940163546454,
-4.0513614597985,-4.03929124303463,-3.97799719175202,-3.92748437027949,
-3.91747126369622,-3.91128897983749,-3.90491163882794,-3.89395098991898,
-3.83625920142476,-3.7778835028167,-3.76189126289714,-3.75114653873282,
-3.74033227188704,-3.72395993843194,-3.6525226917305,-3.62103886952059,
-3.60776360891426,-3.60148803627134),.UNSPECIFIED.);
#1423=B_SPLINE_CURVE_WITH_KNOTS('',3,(#20388,#20389,#20390,#20391,#20392,
#20393,#20394,#20395,#20396,#20397,#20398,#20399,#20400,#20401,#20402,#20403,
#20404,#20405,#20406,#20407,#20408,#20409,#20410,#20411,#20412,#20413,#20414,
#20415,#20416,#20417,#20418,#20419,#20420,#20421,#20422,#20423,#20424,#20425,
#20426,#20427,#20428,#20429,#20430,#20431,#20432,#20433),.UNSPECIFIED.,
 .F.,.F.,(4,2,2,2,2,2,2,2,2,2,2,2,2,2,2,2,2,2,2,2,2,2,4),(-0.458703963070235,
-0.4476103789344,-0.387390603287348,-0.373726897302928,-0.36681426866366,
-0.36088624078785,-0.352333693779791,-0.32719823278997,-0.274608647504632,
-0.229055324726366,-0.214134235080965,-0.203677569512926,-0.19262737818266,
-0.175011958392165,-0.153454737042513,-0.140085221830007,-0.0719338954249617,
-0.0547956271046257,-0.0472815868163417,-0.0414267321571205,-0.0356813677969033,
-0.0279552207881814,-0.000930590274443855),.UNSPECIFIED.);
#1424=B_SPLINE_CURVE_WITH_KNOTS('',3,(#20434,#20435,#20436,#20437,#20438,
#20439,#20440,#20441,#20442,#20443,#20444,#20445,#20446,#20447,#20448,#20449,
#20450,#20451,#20452,#20453,#20454,#20455,#20456,#20457,#20458,#20459,#20460,
#20461,#20462,#20463,#20464,#20465,#20466,#20467,#20468,#20469,#20470,#20471,
#20472,#20473,#20474,#20475,#20476,#20477,#20478,#20479,#20480,#20481,#20482,
#20483,#20484,#20485,#20486,#20487,#20488,#20489,#20490,#20491,#20492,#20493,
#20494,#20495,#20496,#20497,#20498,#20499,#20500,#20501,#20502,#20503,#20504,
#20505,#20506,#20507,#20508,#20509,#20510,#20511,#20512,#20513,#20514,#20515,
#20516,#20517,#20518,#20519,#20520,#20521,#20522,#20523,#20524,#20525,#20526,
#20527,#20528,#20529,#20530,#20531,#20532,#20533,#20534,#20535,#20536,#20537,
#20538,#20539,#20540,#20541,#20542,#20543,#20544,#20545,#20546,#20547,#20548,
#20549,#20550,#20551,#20552,#20553,#20554,#20555,#20556,#20557,#20558,#20559,
#20560,#20561),.UNSPECIFIED.,.F.,.F.,(4,2,2,2,2,2,2,2,2,2,2,2,2,2,2,2,2,
2,2,2,2,2,2,2,2,2,2,2,2,2,2,2,2,2,2,2,2,2,2,2,2,2,2,2,2,2,2,2,2,2,2,2,2,
2,2,2,2,2,2,2,2,2,2,4),(-4.06048203363518,-4.03025455645395,-3.9691349538326,
-3.95369424520963,-3.94304683352945,-3.9321116200381,-3.91509476425701,
-3.84955218125704,-3.79933143232759,-3.78929737786332,-3.78311059686391,
-3.77673781623578,-3.76580068005654,-3.70782017083285,-3.64915364962081,
-3.63340707851152,-3.62270589410659,-3.61184022793493,-3.59519396745887,
-3.51842926964027,-3.49076501195105,-3.47844946162652,-3.46852477553194,
-3.46235979182168,-3.45595900217838,-3.44488608818992,-3.3893318418027,
-3.32767918035704,-3.31229691148376,-3.30165956012622,-3.29071002293352,
-3.27361754916669,-3.19683072234816,-3.16975298762487,-3.15243990351045,
-3.14489903546282,-3.13962441374937,-3.13230314338034,-3.11633927545952,
-3.05838609218079,-3.0101994379,-2.99332016806537,-2.98241057334082,-2.97186714936823,
-2.95641724351904,-2.87838180616511,-2.83655159525338,-2.82690302107234,
-2.82079166632169,-2.81431345858978,-2.80286356868832,-2.75024228454491,
-2.68747732350124,-2.67156813817421,-2.66083741428753,-2.65000483326521,
-2.63353877133443,-2.55649529326159,-2.52876569107145,-2.51643269276606,
-2.50649735215666,-2.50033001830562,-2.49393150688731,-2.48879418648611),
 .UNSPECIFIED.);
#1425=B_SPLINE_CURVE_WITH_KNOTS('',3,(#20566,#20567,#20568,#20569,#20570,
#20571,#20572,#20573,#20574,#20575,#20576,#20577,#20578,#20579,#20580,#20581,
#20582,#20583,#20584,#20585,#20586,#20587,#20588,#20589,#20590,#20591,#20592,
#20593,#20594,#20595,#20596,#20597,#20598,#20599,#20600,#20601,#20602,#20603,
#20604,#20605,#20606,#20607,#20608,#20609,#20610,#20611,#20612,#20613,#20614,
#20615,#20616,#20617,#20618,#20619,#20620,#20621,#20622,#20623,#20624,#20625,
#20626,#20627,#20628,#20629,#20630,#20631,#20632,#20633,#20634,#20635,#20636,
#20637,#20638,#20639,#20640,#20641,#20642,#20643,#20644,#20645,#20646,#20647,
#20648,#20649,#20650,#20651,#20652,#20653,#20654,#20655,#20656,#20657,#20658,
#20659,#20660,#20661,#20662,#20663,#20664,#20665,#20666,#20667,#20668,#20669,
#20670,#20671,#20672,#20673,#20674,#20675,#20676,#20677,#20678,#20679,#20680,
#20681,#20682,#20683,#20684,#20685,#20686,#20687,#20688,#20689,#20690,#20691,
#20692,#20693,#20694,#20695,#20696,#20697,#20698,#20699,#20700,#20701,#20702,
#20703,#20704,#20705,#20706,#20707,#20708,#20709,#20710,#20711,#20712,#20713,
#20714,#20715,#20716,#20717,#20718,#20719,#20720,#20721,#20722,#20723,#20724,
#20725,#20726,#20727),.UNSPECIFIED.,.F.,.F.,(4,2,2,2,2,2,2,2,2,2,2,2,2,
2,2,2,2,2,2,2,2,2,2,2,2,2,2,2,2,2,2,2,2,2,2,2,2,2,2,2,2,2,2,2,2,2,2,2,2,
2,2,2,2,2,2,2,2,2,2,2,2,2,2,2,2,2,2,2,2,2,2,2,2,2,2,2,2,2,2,2,4),(-3.60242287809638,
-3.56721784695233,-3.55156189813843,-3.54087604581589,-3.52998929297132,
-3.51323412204218,-3.44497013969903,-3.39791346110271,-3.38735473125302,
-3.38105987829509,-3.37480333375927,-3.36442970316565,-3.30125673265392,
-3.26400908284791,-3.2460223081981,-3.23059678410155,-3.21995088869975,
-3.20900998526235,-3.19196872439598,-3.12667495572608,-3.07633231876972,
-3.06624290939729,-3.060044392539,-3.05368405300464,-3.04281000897509,-2.98411981411094,
-2.92597258491712,-2.91024653188731,-2.89954788321163,-2.88867582073824,
-2.87200116277746,-2.79526113514378,-2.7676005695254,-2.75528520035583,
-2.74536024613777,-2.73919461687122,-2.73279268291657,-2.72171705169384,
-2.66617790190046,-2.6045148723875,-2.58911903845016,-2.5784782235403,-2.56752998187024,
-2.55045013455705,-2.4856433040347,-2.43459781081709,-2.42465866485077,
-2.4184902403953,-2.41209205800306,-2.40103454940899,-2.34495831573944,
-2.2838783420997,-2.26844777215121,-2.25780098835939,-2.24686128134125,
-2.22982643444661,-2.15269523980569,-2.11311651180288,-2.1035514946851,
-2.09745561068995,-2.09095128173895,-2.07937494247329,-2.03104486686402,
-1.96667113596343,-1.94956534772693,-1.93861223520825,-1.92797478084316,
-1.9125987156333,-1.84933732086722,-1.79562684674695,-1.78435791261974,
-1.77791627132938,-1.77177925894983,-1.76200059891485,-1.71521190961271,
-1.64467016553331,-1.62818656919652,-1.6173497828642,-1.60662021642605,
-1.59072325636642,-1.57270504429441),.UNSPECIFIED.);
#1426=B_SPLINE_CURVE_WITH_KNOTS('',3,(#20728,#20729,#20730,#20731,#20732,
#20733,#20734,#20735,#20736,#20737,#20738,#20739,#20740,#20741,#20742,#20743,
#20744,#20745,#20746,#20747,#20748,#20749,#20750,#20751,#20752,#20753,#20754,
#20755,#20756,#20757,#20758,#20759,#20760,#20761,#20762,#20763,#20764,#20765,
#20766,#20767,#20768,#20769,#20770,#20771,#20772,#20773,#20774,#20775,#20776,
#20777,#20778,#20779,#20780,#20781,#20782,#20783,#20784,#20785,#20786,#20787,
#20788,#20789,#20790,#20791,#20792,#20793,#20794,#20795,#20796,#20797,#20798,
#20799,#20800,#20801,#20802,#20803,#20804,#20805,#20806,#20807,#20808,#20809,
#20810,#20811,#20812,#20813,#20814,#20815,#20816,#20817,#20818,#20819,#20820,
#20821,#20822,#20823,#20824,#20825,#20826,#20827,#20828,#20829,#20830,#20831,
#20832,#20833,#20834,#20835,#20836,#20837,#20838,#20839,#20840,#20841,#20842,
#20843,#20844,#20845,#20846,#20847,#20848,#20849,#20850,#20851,#20852,#20853,
#20854,#20855,#20856,#20857,#20858,#20859,#20860,#20861,#20862,#20863,#20864,
#20865,#20866,#20867,#20868,#20869,#20870,#20871,#20872,#20873,#20874,#20875,
#20876,#20877,#20878,#20879,#20880,#20881,#20882,#20883,#20884,#20885,#20886,
#20887,#20888,#20889,#20890,#20891,#20892,#20893),.UNSPECIFIED.,.F.,.F.,
(4,2,2,2,2,2,2,2,2,2,2,2,2,2,2,2,2,2,2,2,2,2,2,2,2,2,2,2,2,2,2,2,2,2,2,
2,2,2,2,2,2,2,2,2,2,2,2,2,2,2,2,2,2,2,2,2,2,2,2,2,2,2,2,2,2,2,2,2,2,2,2,
2,2,2,2,2,2,2,2,2,2,2,4),(-2.48879418648611,-2.482870786226,-2.42692956343107,
-2.36600785850896,-2.35045675318813,-2.33978959585287,-2.33016094885262,
-2.31444582835103,-2.23821710940245,-2.19523975059826,-2.1855542992085,
-2.17943580816656,-2.17296831262753,-2.16157124617673,-2.11118827433854,
-2.06704068844034,-2.04734877497841,-2.0308590398503,-2.02002175028717,
-2.00929425375571,-1.99340524118733,-1.97468006647316,-1.93457908581669,
-1.87709109853615,-1.86610750722511,-1.85972480069881,-1.85354479225751,
-1.84354696670865,-1.79297932372389,-1.72782025145022,-1.71077564213425,
-1.69983433429665,-1.6891891139229,-1.67376662544518,-1.65578255957856,
-1.61854770167534,-1.55527893663139,-1.54491074496027,-1.53865537392209,
-1.53235915546231,-1.52179434822374,-1.47368194101312,-1.40684450290551,
-1.38994962777,-1.37903651957945,-1.36837058921596,-1.3528291953071,-1.29288180784992,
-1.2357731213652,-1.2247627523323,-1.21837436650977,-1.21219837856251,-1.20222149130216,
-1.18982109384957,-1.16183326387008,-1.08267697612122,-1.06740015276224,
-1.05688543352747,-1.0459323793008,-1.02882628372556,-0.978950224072073,
-0.917329280997904,-0.905017534155332,-0.898365664895021,-0.892347412696423,
-0.883212145366521,-0.851369147050279,-0.8063673714056,-0.761177170046655,
-0.74626846473054,-0.735813488995268,-0.724759123042586,-0.707123289176841,
-0.685531949518534,-0.632133201827475,-0.591798795701873,-0.582163133943164,
-0.576655828465875,-0.570375876223591,-0.559890990576539,-0.546636681512379,
-0.51524224622991,-0.45931701754657),.UNSPECIFIED.);
#1427=B_SPLINE_CURVE_WITH_KNOTS('',3,(#20899,#20900,#20901,#20902,#20903,
#20904,#20905,#20906,#20907,#20908,#20909,#20910,#20911,#20912,#20913,#20914,
#20915,#20916,#20917,#20918,#20919,#20920,#20921,#20922,#20923,#20924,#20925,
#20926,#20927,#20928,#20929,#20930,#20931,#20932,#20933,#20934,#20935,#20936,
#20937,#20938,#20939,#20940,#20941,#20942,#20943,#20944,#20945,#20946,#20947,
#20948,#20949,#20950,#20951,#20952,#20953,#20954,#20955,#20956,#20957,#20958,
#20959,#20960,#20961,#20962,#20963,#20964,#20965,#20966,#20967,#20968,#20969,
#20970,#20971,#20972,#20973,#20974,#20975,#20976,#20977,#20978,#20979,#20980,
#20981,#20982,#20983,#20984,#20985,#20986,#20987,#20988,#20989,#20990,#20991,
#20992,#20993,#20994,#20995,#20996,#20997,#20998,#20999,#21000,#21001,#21002,
#21003,#21004,#21005,#21006,#21007,#21008,#21009,#21010,#21011,#21012,#21013,
#21014,#21015,#21016,#21017,#21018,#21019,#21020,#21021,#21022,#21023,#21024),
 .UNSPECIFIED.,.F.,.F.,(4,2,2,2,2,2,2,2,2,2,2,2,2,2,2,2,2,2,2,2,2,2,2,2,
2,2,2,2,2,2,2,2,2,2,2,2,2,2,2,2,2,2,2,2,2,2,2,2,2,2,2,2,2,2,2,2,2,2,2,2,
2,2,4),(-1.57273988019061,-1.56691346024312,-1.56072898385932,-1.55070573887629,
-1.50842406317083,-1.43222502173132,-1.41651494897745,-1.4068881047619,
-1.39622185106329,-1.38067029519754,-1.31828553824896,-1.26392823496632,
-1.25275991015442,-1.24633978848889,-1.24018924744267,-1.23033879598207,
-1.1760008817155,-1.11477371714702,-1.09750587349208,-1.08652241989586,
-1.07590625961537,-1.06065247806019,-1.00441058913554,-0.941945479199864,
-0.931484916050102,-0.925210316360724,-0.918933749330253,-0.90846320995488,
-0.895232867586938,-0.863935841053784,-0.792164412777069,-0.775839821530913,
-0.765033207159675,-0.754278155395765,-0.738235749766936,-0.682680727504737,
-0.621535654361532,-0.610922418914989,-0.604616329925545,-0.598370659077198,
-0.588049362231943,-0.575071819605588,-0.544810450900195,-0.470830069515804,
-0.454802593626465,-0.445123229273891,-0.434506544974243,-0.419248850028895,
-0.362877812031364,-0.300576688829507,-0.290096385595649,-0.283817819462706,
-0.277545348773213,-0.26709499646107,-0.253899067128589,-0.222745178504822,
-0.150669428219029,-0.134383624062453,-0.123583848906434,-0.112821487766765,
-0.0967404810140852,-0.0777076763684024,-0.000936417546807567),
 .UNSPECIFIED.);
#1428=B_SPLINE_CURVE_WITH_KNOTS('',3,(#21025,#21026,#21027,#21028,#21029,
#21030,#21031,#21032,#21033,#21034,#21035,#21036,#21037,#21038,#21039,#21040,
#21041,#21042,#21043,#21044,#21045,#21046,#21047,#21048,#21049,#21050,#21051,
#21052,#21053,#21054,#21055,#21056,#21057,#21058,#21059,#21060,#21061,#21062,
#21063,#21064,#21065,#21066),.UNSPECIFIED.,.F.,.F.,(4,2,2,2,2,2,2,2,2,2,
2,2,2,2,2,2,2,2,2,2,4),(-4.06024511832612,-4.04416917649443,-4.03341342658371,
-4.02723973391658,-4.02172518011229,-4.01522137623075,-4.00364660759717,
-3.94883815801512,-3.88741519438322,-3.87198632035072,-3.86134018065844,
-3.85040070853188,-3.83336531020972,-3.76801068386381,-3.71745087900611,
-3.70750155272622,-3.70133131022163,-3.69493621368035,-3.68389271615082,
-3.62747426988344,-3.60242287809638),.UNSPECIFIED.);
#1429=B_SPLINE_CURVE_WITH_KNOTS('',3,(#21068,#21069,#21070,#21071,#21072,
#21073,#21074,#21075,#21076,#21077,#21078,#21079,#21080,#21081,#21082,#21083,
#21084,#21085,#21086,#21087,#21088,#21089,#21090,#21091,#21092,#21093,#21094,
#21095,#21096,#21097,#21098,#21099,#21100,#21101,#21102,#21103,#21104,#21105,
#21106,#21107),.UNSPECIFIED.,.F.,.F.,(4,2,2,2,2,2,2,2,2,2,2,2,2,2,2,2,2,
2,2,4),(-0.45931701754657,-0.443662955116037,-0.427311208082828,-0.416498713796264,
-0.405746798310332,-0.389726540866301,-0.331854426135855,-0.273525442235887,
-0.262610494918398,-0.256241478612075,-0.250049205834386,-0.239992621745995,
-0.227459807822531,-0.198962724177927,-0.121968714348891,-0.106068905204749,
-0.0964095104727434,-0.0857712360881861,-0.0703931358704458,-0.000931723441433497),
 .UNSPECIFIED.);
#1430=B_SPLINE_CURVE_WITH_KNOTS('',3,(#21108,#21109,#21110,#21111,#21112,
#21113,#21114,#21115,#21116,#21117,#21118,#21119,#21120,#21121,#21122,#21123,
#21124,#21125,#21126,#21127,#21128,#21129,#21130,#21131,#21132,#21133,#21134,
#21135,#21136,#21137,#21138,#21139,#21140,#21141,#21142,#21143,#21144,#21145,
#21146,#21147,#21148,#21149,#21150,#21151,#21152,#21153,#21154,#21155,#21156,
#21157,#21158,#21159,#21160,#21161,#21162,#21163,#21164,#21165,#21166,#21167,
#21168,#21169,#21170,#21171,#21172,#21173,#21174,#21175,#21176,#21177,#21178,
#21179,#21180,#21181,#21182,#21183,#21184,#21185,#21186,#21187,#21188,#21189,
#21190,#21191,#21192,#21193,#21194,#21195,#21196,#21197,#21198,#21199,#21200,
#21201,#21202,#21203,#21204,#21205,#21206,#21207,#21208,#21209,#21210,#21211,
#21212,#21213,#21214,#21215,#21216,#21217,#21218,#21219,#21220,#21221,#21222,
#21223,#21224,#21225,#21226,#21227,#21228,#21229,#21230,#21231,#21232,#21233,
#21234,#21235,#21236,#21237,#21238,#21239,#21240,#21241,#21242,#21243,#21244,
#21245,#21246,#21247,#21248,#21249,#21250,#21251,#21252,#21253,#21254,#21255,
#21256,#21257,#21258,#21259,#21260,#21261,#21262,#21263,#21264,#21265,#21266,
#21267,#21268,#21269,#21270),.UNSPECIFIED.,.F.,.F.,(4,3,3,3,3,3,3,3,3,3,
3,3,3,3,3,3,3,3,3,3,3,3,3,3,3,3,3,3,3,3,3,3,3,3,3,3,3,3,3,3,3,3,3,3,3,3,
3,3,3,3,3,3,3,3,4),(-59.6902604182061,-59.5594237704194,-59.4859550544703,
-59.3928003674027,-59.2997701461022,-59.2068368787636,-59.1139699001593,
-59.0211370084654,-58.9283134841204,-58.83547462196,-58.7425375299053,-58.6495479743784,
-58.5564074989373,-58.4931583779947,-58.4000037272726,-58.3069735423544,
-58.2140403113874,-58.1211733689893,-58.0283405133873,-57.9355170249773,
-57.842678198552,-57.7497411417073,-57.6567516211492,-57.563611179937,-57.5003617015191,
-57.4072070142344,-57.3141767929645,-57.2212435259009,-57.1283765479317,
-57.0355436570937,-56.9427201338232,-56.8498812729533,-56.7569441825103,
-56.663954628777,-56.5708141554015,-56.5075650250435,-56.4144102728466,
-56.3213799860577,-56.2284466529631,-56.1355796084747,-56.0427466508417,
-55.9499230605827,-55.8570841326131,-55.7641469753148,-55.6711573547634,
-55.5780168153083,-55.514768348568,-55.4216338866632,-55.3286149917671,
-55.2356867536879,-55.1428243459392,-55.0499907232509,-54.957173946929,
-54.8643241540367,-54.8255493545477),.UNSPECIFIED.);
#1431=B_SPLINE_CURVE_WITH_KNOTS('',3,(#21275,#21276,#21277,#21278,#21279,
#21280,#21281,#21282,#21283,#21284,#21285,#21286,#21287,#21288,#21289,#21290,
#21291,#21292,#21293,#21294,#21295,#21296,#21297,#21298,#21299,#21300,#21301,
#21302,#21303,#21304,#21305,#21306,#21307,#21308,#21309,#21310,#21311,#21312,
#21313,#21314,#21315,#21316,#21317,#21318,#21319,#21320,#21321,#21322,#21323,
#21324,#21325,#21326,#21327,#21328,#21329,#21330,#21331,#21332,#21333,#21334,
#21335,#21336,#21337,#21338,#21339,#21340,#21341,#21342,#21343,#21344,#21345,
#21346,#21347,#21348,#21349,#21350,#21351,#21352,#21353,#21354,#21355,#21356,
#21357,#21358,#21359,#21360,#21361,#21362,#21363,#21364,#21365,#21366,#21367,
#21368,#21369,#21370,#21371,#21372,#21373,#21374,#21375,#21376,#21377,#21378,
#21379,#21380,#21381,#21382,#21383,#21384,#21385,#21386,#21387,#21388,#21389,
#21390,#21391,#21392,#21393,#21394,#21395,#21396,#21397,#21398,#21399,#21400,
#21401,#21402,#21403,#21404,#21405,#21406,#21407,#21408,#21409,#21410,#21411,
#21412,#21413,#21414,#21415,#21416,#21417,#21418,#21419,#21420,#21421,#21422,
#21423,#21424,#21425,#21426,#21427,#21428,#21429,#21430,#21431,#21432,#21433,
#21434,#21435,#21436),.UNSPECIFIED.,.F.,.F.,(4,2,2,2,2,2,2,2,2,2,2,2,2,
2,2,2,2,2,2,2,2,2,2,2,2,2,2,2,2,2,2,2,2,2,2,2,2,2,2,2,2,2,2,2,2,2,2,2,2,
2,2,2,2,2,2,2,2,2,2,2,2,2,2,2,2,2,2,2,2,2,2,2,2,2,2,2,2,2,2,2,4),(-3.60215374024631,
-3.55832024003365,-3.50705427008981,-3.4968341398854,-3.49059980699694,
-3.48507404412005,-3.47524953380503,-3.42545216512038,-3.36226836082976,
-3.34368290842291,-3.33249220157644,-3.32208238891058,-3.30781403324334,
-3.27108441733982,-3.21701855398476,-3.18394106025523,-3.17475410044726,
-3.16875045340127,-3.16214969449917,-3.15009518988101,-3.088210951477,-3.03819078612893,
-3.02105122816739,-3.01007851977686,-2.99954428438166,-2.9842337455252,
-2.90556246335392,-2.877528358283,-2.86511103438098,-2.85512072802792,-2.84893056883329,
-2.84252743093647,-2.83146332856961,-2.77555745219184,-2.71436471944647,
-2.69894454545784,-2.68829726882711,-2.67735044329871,-2.66028994445742,
-2.59511047468227,-2.54430720742812,-2.53437679428667,-2.52821091969801,
-2.52181660033448,-2.5107625946858,-2.45471757638087,-2.39362961337755,
-2.37820211010528,-2.36756281426864,-2.35663583530306,-2.33963333278813,
-2.27391475522454,-2.22361545056843,-2.21367491641689,-2.20750981472791,
-2.20111571714163,-2.19007639515179,-2.12142788152226,-2.08815716591305,
-2.06435557855792,-2.05216201634104,-2.04288922286891,-2.03065362175129,
-2.00660710569097,-1.97279945159265,-1.90547789764357,-1.89420888679343,
-1.88776616735981,-1.88162833803431,-1.87184546381257,-1.82478818754195,
-1.7546494918005,-1.73812119283216,-1.72727711461282,-1.71655653511475,
-1.70070403385726,-1.6820371535432,-1.64216857823805,-1.58423694395074,
-1.57328848970991,-1.57273988019061),.UNSPECIFIED.);
#1432=B_SPLINE_CURVE_WITH_KNOTS('',3,(#21438,#21439,#21440,#21441,#21442,
#21443,#21444,#21445,#21446,#21447,#21448,#21449,#21450,#21451,#21452,#21453,
#21454,#21455,#21456,#21457,#21458,#21459,#21460,#21461,#21462,#21463,#21464,
#21465,#21466,#21467,#21468,#21469,#21470,#21471,#21472,#21473,#21474,#21475,
#21476,#21477,#21478,#21479,#21480,#21481,#21482,#21483,#21484,#21485,#21486),
 .UNSPECIFIED.,.F.,.F.,(4,3,3,3,3,3,3,3,3,3,3,3,3,3,3,3,4),(-54.8255493545477,
-54.7325933049784,-54.6395755236503,-54.5464177867358,-54.5219716720924,
-54.4288168396936,-54.3357864745466,-54.2428530650123,-54.1499859472367,
-54.0571529182782,-53.9643292587279,-53.8714902635756,-53.7785530427219,
-53.6855633605477,-53.5924227631797,-53.5291749956168,-53.4070751110265),
 .UNSPECIFIED.);
#1433=B_SPLINE_CURVE_WITH_KNOTS('',3,(#21487,#21488,#21489,#21490,#21491,
#21492,#21493,#21494,#21495,#21496,#21497,#21498,#21499,#21500,#21501,#21502,
#21503,#21504,#21505,#21506,#21507,#21508,#21509,#21510,#21511,#21512,#21513,
#21514,#21515,#21516,#21517,#21518,#21519,#21520,#21521,#21522,#21523,#21524,
#21525,#21526,#21527,#21528,#21529,#21530,#21531,#21532,#21533,#21534,#21535,
#21536,#21537,#21538,#21539,#21540,#21541,#21542,#21543,#21544,#21545,#21546,
#21547,#21548,#21549,#21550,#21551,#21552,#21553,#21554,#21555,#21556,#21557,
#21558,#21559,#21560,#21561,#21562,#21563,#21564,#21565,#21566,#21567,#21568,
#21569,#21570,#21571,#21572,#21573,#21574,#21575,#21576,#21577,#21578,#21579,
#21580,#21581,#21582,#21583,#21584,#21585,#21586,#21587,#21588,#21589,#21590,
#21591,#21592,#21593,#21594,#21595,#21596,#21597,#21598,#21599,#21600,#21601,
#21602,#21603,#21604,#21605,#21606,#21607,#21608,#21609,#21610,#21611,#21612,
#21613,#21614,#21615,#21616),.UNSPECIFIED.,.F.,.F.,(4,2,2,2,2,2,2,2,2,2,
2,2,2,2,2,2,2,2,2,2,2,2,2,2,2,2,2,2,2,2,2,2,2,2,2,2,2,2,2,2,2,2,2,2,2,2,
2,2,2,2,2,2,2,2,2,2,2,2,2,2,2,2,2,2,4),(1.57246993836349,1.57255871975661,
1.57912898874073,1.58518286264246,1.59453433753174,1.62982177800544,1.6838845987573,
1.71828614481204,1.73092565126013,1.74139304571477,1.75240101115234,1.76982543540094,
1.82223034169457,1.88375253025013,1.89431647517552,1.90060935312462,1.90686298322144,
1.9172215182081,1.93026301994996,1.96077944471626,2.03428548587652,2.05039027237552,
2.06008452998516,2.07069376960653,2.08589349044519,2.14045811894018,2.20324430260467,
2.21444992277198,2.22088009460053,2.22702782231185,2.23685967261981,2.28727759474377,
2.35307275814114,2.37006985100011,2.38100242008193,2.3916543689042,2.40711469823814,
2.4251562826882,2.4626094056295,2.52535635003071,2.53577911681293,2.54204558594937,
2.54832907345374,2.5588350906938,2.5721275374578,2.60368083522067,2.6749914601101,
2.69138269714049,2.70220098702464,2.71294337437566,2.72891972722895,2.78831623300196,
2.84490980446916,2.85594447347385,2.86233734383786,2.86850877892949,2.8784642278196,
2.92941239254775,2.99428247378257,3.01135593775882,3.0223027976203,3.03294423964134,
3.04834472225774,3.1101328671186,3.14415938148886),.UNSPECIFIED.);
#1434=B_SPLINE_CURVE_WITH_KNOTS('',3,(#21620,#21621,#21622,#21623,#21624,
#21625,#21626,#21627,#21628,#21629,#21630,#21631,#21632,#21633,#21634,#21635,
#21636,#21637,#21638,#21639,#21640,#21641,#21642,#21643,#21644,#21645,#21646,
#21647,#21648,#21649,#21650,#21651,#21652,#21653,#21654,#21655,#21656),
 .UNSPECIFIED.,.F.,.F.,(4,3,3,3,3,3,3,3,3,3,3,3,4),(102.721401181859,102.870662929443,
102.958378318029,103.045982635166,103.133500549336,103.220958859954,103.308386983301,
103.395807072386,103.483241269198,103.570759547802,103.658325393878,103.746016067803,
103.787441035706),.UNSPECIFIED.);
#1435=B_SPLINE_CURVE_WITH_KNOTS('',3,(#21662,#21663,#21664,#21665,#21666,
#21667,#21668,#21669,#21670,#21671),.UNSPECIFIED.,.F.,.F.,(4,1,1,1,1,1,
1,4),(-105.704105011142,-104.856256282395,-103.863459605919,-102.870662929443,
-101.877866252968,-100.885069576492,-99.8922729000164,-99.4209215138263),
 .UNSPECIFIED.);
#1436=B_SPLINE_CURVE_WITH_KNOTS('',3,(#21673,#21674,#21675,#21676,#21677,
#21678,#21679,#21680,#21681,#21682,#21683,#21684,#21685,#21686,#21687,#21688,
#21689,#21690,#21691,#21692,#21693,#21694,#21695,#21696,#21697,#21698,#21699,
#21700,#21701,#21702,#21703,#21704,#21705,#21706,#21707,#21708,#21709,#21710,
#21711,#21712,#21713,#21714,#21715,#21716,#21717,#21718,#21719,#21720,#21721,
#21722,#21723,#21724,#21725,#21726,#21727,#21728,#21729,#21730,#21731,#21732,
#21733,#21734,#21735,#21736,#21737,#21738,#21739,#21740,#21741,#21742,#21743,
#21744,#21745,#21746,#21747,#21748,#21749,#21750,#21751,#21752,#21753,#21754,
#21755,#21756,#21757,#21758,#21759,#21760,#21761,#21762,#21763,#21764,#21765,
#21766,#21767,#21768,#21769,#21770,#21771,#21772,#21773,#21774,#21775,#21776,
#21777,#21778,#21779,#21780,#21781,#21782,#21783,#21784,#21785,#21786,#21787,
#21788,#21789,#21790,#21791,#21792,#21793,#21794,#21795,#21796,#21797,#21798,
#21799,#21800,#21801,#21802,#21803,#21804,#21805,#21806,#21807,#21808,#21809,
#21810,#21811,#21812,#21813,#21814,#21815,#21816,#21817,#21818,#21819,#21820,
#21821,#21822,#21823,#21824,#21825,#21826,#21827,#21828,#21829,#21830,#21831,
#21832,#21833,#21834,#21835,#21836,#21837,#21838,#21839,#21840,#21841,#21842,
#21843,#21844,#21845,#21846,#21847,#21848,#21849,#21850,#21851,#21852,#21853,
#21854,#21855,#21856,#21857,#21858,#21859,#21860,#21861,#21862,#21863,#21864,
#21865,#21866,#21867,#21868,#21869,#21870,#21871,#21872,#21873,#21874,#21875,
#21876,#21877,#21878,#21879,#21880,#21881,#21882,#21883,#21884,#21885,#21886,
#21887,#21888,#21889,#21890,#21891,#21892,#21893,#21894,#21895,#21896,#21897,
#21898),.UNSPECIFIED.,.F.,.F.,(4,3,3,3,3,3,3,3,3,3,3,3,3,3,3,3,3,3,3,3,
3,3,3,3,3,3,3,3,3,3,3,3,3,3,3,3,3,3,3,3,3,3,3,3,3,3,3,3,3,3,3,3,3,3,3,3,
3,3,3,3,3,3,3,3,3,3,3,3,3,3,3,3,3,3,3,4),(-99.4209197039621,-99.3293208753837,
-99.2376279663801,-99.1457470587024,-99.05376624967,-98.9615873900447,-98.8994762235407,
-98.8108583933232,-98.7223539962568,-98.6339393192582,-98.5430318477341,
-98.4547169969307,-98.3664149889373,-98.2781045317982,-98.1852482856149,
-98.0968062954329,-98.0083035049247,-97.9196751481056,-97.9066795470651,
-97.8180467295868,-97.7295271647582,-97.6410971592762,-97.5501953731904,
-97.4618648930757,-97.3735471711978,-97.2852209326452,-97.1923864171312,
-97.1039286208209,-97.0154100174652,-96.9267659333002,-96.9138828705894,
-96.825251508294,-96.7367333851373,-96.6483048060602,-96.5574024795669,
-96.4690733781967,-96.3807570148084,-96.2924321128727,-96.199595633183,
-96.1111391054233,-96.0226217469349,-95.9339788663736,-95.9210861941138,
-95.8324578037414,-95.74394270537,-95.6555171999199,-95.5646137396346,-95.476287813751,
-95.3879746582396,-95.2996529931624,-95.2068121242814,-95.1183588768868,
-95.0298448134196,-94.9412052289657,-94.9282895176381,-94.8396591330816,
-94.7511420149651,-94.662714466852,-94.5718117636408,-94.4834837512752,
-94.3951684966289,-94.3068447220381,-94.2140067518192,-94.125551388185,
-94.0370352064011,-93.9483935134071,-93.9354928411625,-93.8481338474163,
-93.7593339161101,-93.672189012311,-93.5850984288973,-93.498039699971,-93.40796337422,
-93.320869528771,-93.229301962869,-93.137734396967),.UNSPECIFIED.);
#1437=B_SPLINE_CURVE_WITH_KNOTS('',3,(#21900,#21901,#21902,#21903,#21904,
#21905,#21906,#21907,#21908,#21909,#21910,#21911,#21912,#21913,#21914,#21915,
#21916,#21917,#21918,#21919,#21920,#21921,#21922,#21923,#21924,#21925,#21926,
#21927,#21928,#21929,#21930,#21931,#21932,#21933,#21934,#21935,#21936,#21937,
#21938,#21939,#21940,#21941,#21942,#21943,#21944,#21945,#21946,#21947,#21948,
#21949,#21950,#21951,#21952,#21953,#21954,#21955,#21956,#21957,#21958,#21959,
#21960,#21961,#21962,#21963,#21964,#21965,#21966,#21967,#21968,#21969,#21970,
#21971,#21972,#21973,#21974,#21975,#21976,#21977,#21978,#21979,#21980,#21981,
#21982,#21983,#21984,#21985,#21986,#21987,#21988,#21989,#21990,#21991,#21992,
#21993,#21994,#21995,#21996,#21997,#21998,#21999,#22000,#22001,#22002,#22003,
#22004,#22005,#22006,#22007,#22008,#22009,#22010,#22011,#22012,#22013,#22014,
#22015,#22016,#22017,#22018,#22019,#22020,#22021,#22022,#22023,#22024,#22025,
#22026,#22027,#22028,#22029,#22030,#22031,#22032,#22033,#22034,#22035,#22036,
#22037,#22038,#22039,#22040,#22041,#22042,#22043,#22044,#22045,#22046,#22047,
#22048,#22049,#22050,#22051,#22052,#22053,#22054,#22055,#22056,#22057,#22058,
#22059,#22060,#22061,#22062,#22063,#22064,#22065,#22066,#22067,#22068,#22069,
#22070,#22071,#22072,#22073,#22074,#22075,#22076,#22077,#22078,#22079,#22080,
#22081,#22082,#22083,#22084,#22085,#22086,#22087,#22088,#22089,#22090,#22091,
#22092,#22093,#22094,#22095,#22096,#22097,#22098,#22099,#22100,#22101,#22102,
#22103,#22104,#22105,#22106,#22107,#22108,#22109,#22110,#22111,#22112,#22113,
#22114,#22115,#22116,#22117,#22118,#22119,#22120,#22121,#22122,#22123,#22124,
#22125),.UNSPECIFIED.,.F.,.F.,(4,3,3,3,3,3,3,3,3,3,3,3,3,3,3,3,3,3,3,3,
3,3,3,3,3,3,3,3,3,3,3,3,3,3,3,3,3,3,3,3,3,3,3,3,3,3,3,3,3,3,3,3,3,3,3,3,
3,3,3,3,3,3,3,3,3,3,3,3,3,3,3,3,3,3,3,4),(-93.1377343967825,-93.0103943584027,
-92.9426961646869,-92.8540664377197,-92.7655499839449,-92.6771231060632,
-92.5862201538317,-92.4978928219952,-92.4095782505129,-92.321255160973,
-92.2284162427826,-92.1399615626117,-92.0514460636615,-91.9628050484979,
-91.9498994882112,-91.8612695033504,-91.772752788195,-91.6843256457884,
-91.5934227915318,-91.5050951890547,-91.4167803451294,-91.3284569816384,
-91.2356184391627,-91.1471634837603,-91.0586477091683,-90.9700064194352,
-90.9571028117356,-90.8684728896893,-90.7799562377415,-90.6915291588546,
-90.6006262809053,-90.5122987423081,-90.4239839622835,-90.335660662643,
-90.2428220307972,-90.1543671385224,-90.0658514268007,-89.9772101991928,
-89.9643061352599,-89.8756762436412,-89.7871596227823,-89.698732575604,
-89.6078296860015,-89.5195021804533,-89.4311874339195,-89.3428641681764,
-89.2500254908284,-89.1615706331691,-89.0730549563071,-88.9844137636974,
-88.9715094587843,-88.8828795346996,-88.7943628809135,-88.7059358003901,
-88.6150329231299,-88.5267053834115,-88.4383906024603,-88.3500673020895,
-88.2572286721443,-88.1687737796457,-88.0802580678753,-87.9916168404687,
-87.9787127823086,-87.890082868362,-87.8015662248006,-87.7131391545749,
-87.6222362734821,-87.5339087441764,-87.4455939736623,-87.3572706837416,
-87.2644320392645,-87.1759771571514,-87.087461455743,-86.9988202386023,
-86.985916105833,-86.8545490896029),.UNSPECIFIED.);
#1438=B_SPLINE_CURVE_WITH_KNOTS('',3,(#22127,#22128,#22129,#22130,#22131,
#22132,#22133,#22134,#22135,#22136,#22137,#22138,#22139,#22140,#22141,#22142,
#22143,#22144,#22145,#22146,#22147,#22148,#22149,#22150,#22151,#22152,#22153,
#22154,#22155,#22156,#22157,#22158,#22159,#22160,#22161,#22162,#22163,#22164,
#22165,#22166,#22167,#22168,#22169,#22170,#22171,#22172,#22173,#22174,#22175,
#22176,#22177,#22178,#22179,#22180,#22181,#22182,#22183,#22184,#22185,#22186,
#22187,#22188,#22189,#22190,#22191,#22192,#22193,#22194,#22195,#22196,#22197,
#22198,#22199,#22200,#22201,#22202,#22203,#22204,#22205,#22206,#22207,#22208,
#22209,#22210,#22211,#22212,#22213,#22214,#22215,#22216,#22217,#22218,#22219,
#22220,#22221,#22222,#22223,#22224,#22225,#22226,#22227,#22228,#22229,#22230,
#22231,#22232,#22233,#22234,#22235,#22236,#22237,#22238,#22239,#22240,#22241,
#22242,#22243,#22244,#22245,#22246,#22247,#22248,#22249,#22250,#22251,#22252,
#22253,#22254,#22255,#22256,#22257,#22258,#22259,#22260,#22261,#22262,#22263,
#22264,#22265,#22266,#22267,#22268,#22269,#22270,#22271,#22272,#22273,#22274,
#22275,#22276,#22277,#22278,#22279,#22280,#22281,#22282,#22283,#22284,#22285,
#22286,#22287,#22288,#22289,#22290,#22291,#22292,#22293,#22294,#22295,#22296,
#22297,#22298,#22299,#22300,#22301,#22302,#22303,#22304,#22305,#22306,#22307,
#22308,#22309,#22310,#22311,#22312,#22313,#22314,#22315,#22316,#22317,#22318,
#22319,#22320,#22321,#22322,#22323,#22324,#22325,#22326,#22327,#22328,#22329,
#22330,#22331,#22332,#22333,#22334,#22335,#22336,#22337,#22338,#22339,#22340,
#22341,#22342,#22343,#22344,#22345,#22346,#22347,#22348,#22349,#22350,#22351,
#22352),.UNSPECIFIED.,.F.,.F.,(4,3,3,3,3,3,3,3,3,3,3,3,3,3,3,3,3,3,3,3,
3,3,3,3,3,3,3,3,3,3,3,3,3,3,3,3,3,3,3,3,3,3,3,3,3,3,3,3,3,3,3,3,3,3,3,3,
3,3,3,3,3,3,3,3,3,3,3,3,3,3,3,3,3,3,3,4),(-86.8545490893979,-86.7672499901414,
-86.6800454109648,-86.5929101898395,-86.5058118038681,-86.4187278319951,
-86.3316358695655,-86.2444597005961,-86.1572411555414,-86.0698827457749,
-85.9931194293573,-85.9044895140403,-85.8159728691177,-85.7275457975421,
-85.6366429169596,-85.5483153863403,-85.4600006145283,-85.3716773233271,
-85.2788386807158,-85.1903837973786,-85.1018680947656,-85.0132268764558,
-85.0003227528817,-84.9116928390893,-84.8231761957068,-84.7347491256843,
-84.6438462445245,-84.5555187154812,-84.4672039452513,-84.378880655636,
-84.2860420108285,-84.1975871290725,-84.1090714280394,-84.0204302112969,
-84.0075260764061,-83.9188961627797,-83.8303795195696,-83.7419524497257,
-83.6510495685013,-83.5627220396514,-83.4744072696198,-83.386083980208,
-83.2932453351386,-83.2047904535967,-83.1162747527811,-83.0276335362603,
-83.0147293999304,-82.926099485826,-82.8375828421303,-82.7491557717945,
-82.658252890752,-82.5699253613962,-82.4816105908546,-82.3932873009289,
-82.3004486565604,-82.2119937745,-82.1234780731646,-82.0348368561247,-82.0219327234548,
-81.9333028095752,-81.8447861661066,-81.7563590960003,-81.6654562148727,
-81.5771286857499,-81.4888139154421,-81.4004906257509,-81.307651981058,
-81.2191970992323,-81.1306813981307,-81.0420401813238,-81.0291360469791,
-80.9342373457995,-80.8396305779098,-80.7452006727478,-80.6510359595392,
-80.571363782615),.UNSPECIFIED.);
#1439=B_SPLINE_CURVE_WITH_KNOTS('',3,(#22354,#22355,#22356,#22357,#22358,
#22359,#22360,#22361,#22362,#22363,#22364,#22365,#22366,#22367,#22368,#22369,
#22370,#22371,#22372,#22373,#22374,#22375,#22376,#22377,#22378,#22379,#22380,
#22381,#22382,#22383,#22384,#22385,#22386,#22387,#22388,#22389,#22390,#22391,
#22392,#22393,#22394,#22395,#22396,#22397,#22398,#22399,#22400,#22401,#22402,
#22403,#22404,#22405,#22406,#22407,#22408,#22409,#22410,#22411,#22412,#22413,
#22414,#22415,#22416,#22417,#22418,#22419,#22420,#22421,#22422,#22423,#22424,
#22425,#22426,#22427,#22428,#22429,#22430,#22431,#22432,#22433,#22434,#22435,
#22436,#22437,#22438,#22439,#22440,#22441,#22442,#22443,#22444,#22445,#22446,
#22447,#22448,#22449,#22450,#22451,#22452,#22453,#22454,#22455,#22456,#22457,
#22458,#22459,#22460,#22461,#22462,#22463,#22464,#22465,#22466,#22467,#22468,
#22469,#22470,#22471,#22472,#22473,#22474,#22475,#22476,#22477,#22478,#22479,
#22480,#22481,#22482,#22483,#22484,#22485,#22486,#22487,#22488,#22489,#22490,
#22491,#22492,#22493,#22494,#22495,#22496,#22497,#22498,#22499,#22500,#22501,
#22502,#22503,#22504,#22505,#22506,#22507,#22508,#22509,#22510,#22511,#22512,
#22513,#22514,#22515,#22516,#22517,#22518,#22519,#22520,#22521,#22522,#22523,
#22524,#22525,#22526,#22527,#22528,#22529,#22530,#22531,#22532,#22533,#22534,
#22535,#22536,#22537,#22538,#22539,#22540,#22541,#22542,#22543,#22544,#22545,
#22546,#22547,#22548,#22549,#22550,#22551,#22552,#22553,#22554,#22555,#22556,
#22557,#22558,#22559,#22560,#22561,#22562,#22563,#22564,#22565,#22566,#22567,
#22568,#22569,#22570,#22571,#22572,#22573,#22574,#22575,#22576,#22577,#22578,
#22579),.UNSPECIFIED.,.F.,.F.,(4,3,3,3,3,3,3,3,3,3,3,3,3,3,3,3,3,3,3,3,
3,3,3,3,3,3,3,3,3,3,3,3,3,3,3,3,3,3,3,3,3,3,3,3,3,3,3,3,3,3,3,3,3,3,3,3,
3,3,3,3,3,3,3,3,3,3,3,3,3,3,3,3,3,3,3,4),(-80.5713637824232,-80.4802388382001,
-80.3890358883964,-80.2976607708068,-80.2061965706322,-80.1145367878468,
-80.0363393705035,-79.9477094565397,-79.8591928129868,-79.7707657427952,
-79.6798628616993,-79.5915353324914,-79.5032205620988,-79.414897272323,
-79.3220586277492,-79.23360374584,-79.1450880446554,-79.0564468277664,-79.0435426940279,
-78.9549127801537,-78.8663961366907,-78.7779690665895,-78.6870661854598,
-78.5987386563421,-78.5104238860394,-78.4221005963534,-78.3292619516531,
-78.2408070698319,-78.152291368735,-78.0636501519321,-78.0507460175522,
-77.9621161036702,-77.8735994601996,-77.7851723900913,-77.6942695089645,
-77.6059419798413,-77.5176272095339,-77.4293039198435,-77.3364652751518,
-77.2480103933277,-77.1594946922283,-77.0708534754237,-77.0579493410766,
-76.9693194269626,-76.8808027832593,-76.792375712917,-76.7014728318775,
-76.6131453025204,-76.5248305319791,-76.4365072420554,-76.3436685976918,
-76.2552137156379,-76.16669801431,-76.0780567972801,-76.0651526646009,-75.9765227510041,
-75.8880061078176,-75.7995790379919,-75.7086761567586,-75.6203486279128,
-75.5320338578802,-75.4437105684623,-75.350871923378,-75.2624170418168,
-75.1739013409774,-75.0852601244265,-75.0723559881253,-74.9849531892148,
-74.8976869217581,-74.8104984384445,-74.7233652466618,-74.6362649091503,
-74.5491421323337,-74.4620121544108,-74.3747943755378,-74.2881784754821),
 .UNSPECIFIED.);
#1440=B_SPLINE_CURVE_WITH_KNOTS('',3,(#22581,#22582,#22583,#22584,#22585,
#22586,#22587,#22588,#22589,#22590,#22591,#22592,#22593,#22594,#22595,#22596,
#22597,#22598,#22599,#22600,#22601,#22602,#22603,#22604,#22605,#22606,#22607,
#22608,#22609,#22610,#22611,#22612,#22613,#22614,#22615,#22616,#22617,#22618,
#22619,#22620,#22621,#22622,#22623,#22624,#22625,#22626,#22627,#22628,#22629,
#22630,#22631,#22632,#22633,#22634,#22635,#22636,#22637,#22638,#22639,#22640,
#22641,#22642,#22643,#22644,#22645,#22646,#22647,#22648,#22649,#22650,#22651,
#22652,#22653,#22654,#22655,#22656,#22657,#22658,#22659,#22660,#22661,#22662,
#22663,#22664,#22665,#22666,#22667,#22668,#22669,#22670,#22671,#22672,#22673,
#22674,#22675,#22676,#22677,#22678,#22679,#22680,#22681,#22682,#22683,#22684,
#22685,#22686,#22687,#22688,#22689,#22690,#22691,#22692,#22693,#22694,#22695,
#22696,#22697,#22698,#22699,#22700,#22701,#22702,#22703,#22704,#22705,#22706,
#22707,#22708,#22709,#22710,#22711,#22712,#22713,#22714,#22715,#22716,#22717,
#22718,#22719,#22720,#22721,#22722,#22723,#22724,#22725,#22726,#22727,#22728,
#22729,#22730,#22731,#22732,#22733,#22734,#22735,#22736,#22737,#22738,#22739,
#22740,#22741,#22742,#22743,#22744,#22745,#22746,#22747,#22748,#22749,#22750,
#22751,#22752,#22753,#22754,#22755,#22756,#22757,#22758,#22759,#22760,#22761,
#22762,#22763,#22764,#22765,#22766,#22767,#22768,#22769,#22770,#22771,#22772,
#22773,#22774,#22775,#22776,#22777,#22778,#22779,#22780,#22781,#22782,#22783,
#22784,#22785,#22786,#22787,#22788,#22789,#22790,#22791,#22792,#22793,#22794,
#22795,#22796,#22797,#22798,#22799,#22800,#22801,#22802,#22803,#22804,#22805,
#22806),.UNSPECIFIED.,.F.,.F.,(4,3,3,3,3,3,3,3,3,3,3,3,3,3,3,3,3,3,3,3,
3,3,3,3,3,3,3,3,3,3,3,3,3,3,3,3,3,3,3,3,3,3,3,3,3,3,3,3,3,3,3,3,3,3,3,3,
3,3,3,3,3,3,3,3,3,3,3,3,3,3,3,3,3,3,3,4),(-74.2881784752437,-74.1649193736331,
-74.0795593116496,-73.9909293962694,-73.9024127512956,-73.8139856796808,
-73.7230827991175,-73.6347552684894,-73.5464404966801,-73.4581172054929,
-73.3652785629132,-73.2768236796181,-73.188307977057,-73.0996667588124,
-73.086762635174,-72.9981327240733,-72.9096160833806,-72.8211890160432,
-72.7302861338751,-72.6419586074888,-72.5536438399008,-72.4653205529098,
-72.3724819043569,-72.2840270251565,-72.1955113266547,-72.106870112395,
-72.0939659586983,-72.0053360444867,-71.9168194007111,-71.8283923303221,
-71.7374894493097,-71.6491619199673,-71.5608471494635,-71.4725238596003,
-71.3796852152559,-71.291230333318,-71.2027146321253,-71.1140734152566,
-71.1011692822227,-71.0125393577712,-70.9240227036889,-70.8355956229393,
-70.7446927457903,-70.6563652060211,-70.5680504250841,-70.4797271247928,
-70.3868884950313,-70.2984336027753,-70.2099178913036,-70.1212766642732,
-70.108372605747,-70.0197427159813,-69.9312260966195,-69.8427990505834,
-69.7518961604194,-69.6635686551279,-69.5752539085218,-69.4869306423774,
-69.3940919641009,-69.3056371052161,-69.2171214268451,-69.1284802323341,
-69.1155759292714,-69.0269460046457,-68.9384293506142,-68.8500022701374,
-68.7590993929697,-68.6707718540151,-68.5824570740912,-68.4941337750091,
-68.4012951444558,-68.3128402538869,-68.224324544266,-68.1356833193045,
-68.1227792527958,-68.0049931680641),.UNSPECIFIED.);
#1441=B_SPLINE_CURVE_WITH_KNOTS('',3,(#22808,#22809,#22810,#22811,#22812,
#22813,#22814,#22815,#22816,#22817,#22818,#22819,#22820,#22821,#22822,#22823,
#22824,#22825,#22826,#22827,#22828,#22829,#22830,#22831,#22832,#22833,#22834,
#22835,#22836,#22837,#22838,#22839,#22840,#22841,#22842,#22843,#22844,#22845,
#22846,#22847,#22848,#22849,#22850,#22851,#22852,#22853,#22854,#22855,#22856,
#22857,#22858,#22859,#22860,#22861,#22862,#22863,#22864,#22865,#22866,#22867,
#22868,#22869,#22870,#22871,#22872,#22873,#22874,#22875,#22876,#22877,#22878,
#22879,#22880,#22881,#22882,#22883,#22884,#22885,#22886,#22887,#22888,#22889,
#22890,#22891,#22892,#22893,#22894,#22895,#22896,#22897,#22898,#22899,#22900,
#22901,#22902,#22903,#22904,#22905,#22906,#22907,#22908,#22909,#22910,#22911,
#22912,#22913,#22914,#22915,#22916,#22917,#22918,#22919,#22920,#22921,#22922,
#22923,#22924,#22925,#22926,#22927,#22928,#22929,#22930,#22931,#22932,#22933,
#22934,#22935,#22936,#22937,#22938,#22939,#22940,#22941,#22942,#22943,#22944,
#22945,#22946,#22947,#22948,#22949,#22950,#22951,#22952,#22953,#22954,#22955,
#22956,#22957,#22958,#22959,#22960,#22961,#22962,#22963,#22964,#22965,#22966,
#22967,#22968,#22969,#22970,#22971,#22972,#22973,#22974,#22975,#22976,#22977,
#22978,#22979,#22980,#22981,#22982,#22983,#22984,#22985,#22986,#22987,#22988,
#22989,#22990,#22991,#22992,#22993,#22994,#22995,#22996,#22997,#22998,#22999,
#23000,#23001,#23002,#23003,#23004,#23005,#23006,#23007,#23008,#23009,#23010,
#23011,#23012,#23013,#23014,#23015,#23016,#23017,#23018,#23019,#23020,#23021,
#23022,#23023,#23024,#23025,#23026,#23027,#23028,#23029,#23030,#23031,#23032,
#23033),.UNSPECIFIED.,.F.,.F.,(4,3,3,3,3,3,3,3,3,3,3,3,3,3,3,3,3,3,3,3,
3,3,3,3,3,3,3,3,3,3,3,3,3,3,3,3,3,3,3,3,3,3,3,3,3,3,3,3,3,3,3,3,3,3,3,3,
3,3,3,3,3,3,3,3,3,3,3,3,3,3,3,3,3,3,3,4),(-68.0049931678491,-67.9176272364039,
-67.8303590125715,-67.7428119580401,-67.6556573987918,-67.5685201374423,
-67.4813778063888,-67.3935289988716,-67.306263955284,-67.2181232658021,
-67.1299825763201,-67.0413528634227,-66.9528364210138,-66.8644095518054,
-66.7735065953103,-66.6851792654233,-66.5968646933924,-66.5085416008059,
-66.4157026755656,-66.3272479860896,-66.2387324756828,-66.150091446084,
-66.1371858998445,-66.0485558370061,-65.9600390458805,-65.8716118295741,
-65.7807090037984,-65.6923813329701,-65.6040664228603,-65.5157429954148,
-65.4229045524033,-65.3344495392061,-65.2459337089372,-65.1572923668465,
-65.1443892233688,-65.0557588345089,-64.9672417129162,-64.8788141621505,
-64.7879114602434,-64.6995834472815,-64.6112681928031,-64.5229444191439,
-64.4301064510812,-64.3416510902931,-64.2531349120133,-64.1644932234347,
-64.1515925468932,-64.0629642601545,-63.9744492455001,-63.8860238039323,
-63.7951203122429,-63.70679440072,-63.6184812411673,-63.5301595536508,-63.4373186328424,
-63.3488653169106,-63.2603511690565,-63.1717114782792,-63.1587958704175,
-63.0701642993288,-62.9816460075068,-62.8932172997264,-62.8023150365033,
-62.7139859062041,-62.6256695509626,-62.5373446942416,-62.4445083191667,
-62.3560519294957,-62.2675347410291,-62.1788920746855,-62.1659991939419,
-62.0703971982959,-61.9751094420689,-61.8800163865857,-61.7852175910644,
-61.7218081198968),.UNSPECIFIED.);
#1442=B_SPLINE_CURVE_WITH_KNOTS('',3,(#23035,#23036,#23037,#23038,#23039,
#23040,#23041,#23042,#23043,#23044),.UNSPECIFIED.,.F.,.F.,(4,1,1,1,1,1,
1,4),(-61.7218078608845,-61.1732025174663,-60.1804058409906,-59.187609164515,
-58.1948124880393,-57.2020158115637,-56.209219135088,-55.4386448475283),
 .UNSPECIFIED.);
#1443=B_SPLINE_CURVE_WITH_KNOTS('',3,(#23046,#23047,#23048,#23049,#23050,
#23051),.UNSPECIFIED.,.F.,.F.,(4,2,4),(0.00013759178667376,0.0288396991503689,
0.0579150026494099),.UNSPECIFIED.);
#1444=B_SPLINE_CURVE_WITH_KNOTS('',3,(#23055,#23056,#23057,#23058,#23059,
#23060,#23061,#23062,#23063),.UNSPECIFIED.,.F.,.F.,(4,1,1,1,1,1,4),(53.2308291056646,
54.2236257821402,55.2164224586157,56.2092191350913,57.2020158115669,58.1948124880425,
58.7391040316016),.UNSPECIFIED.);
#1445=B_SPLINE_CURVE_WITH_KNOTS('',3,(#23065,#23066,#23067,#23068,#23069,
#23070,#23071,#23072,#23073,#23074,#23075,#23076,#23077,#23078,#23079,#23080,
#23081,#23082,#23083,#23084,#23085,#23086,#23087,#23088,#23089,#23090,#23091,
#23092,#23093,#23094,#23095,#23096,#23097,#23098,#23099,#23100,#23101,#23102,
#23103,#23104,#23105,#23106,#23107,#23108,#23109,#23110,#23111,#23112,#23113,
#23114,#23115,#23116,#23117,#23118,#23119,#23120,#23121,#23122,#23123,#23124,
#23125,#23126,#23127,#23128,#23129,#23130,#23131,#23132,#23133,#23134,#23135,
#23136,#23137,#23138,#23139,#23140,#23141,#23142,#23143,#23144,#23145,#23146,
#23147,#23148,#23149,#23150,#23151,#23152,#23153,#23154,#23155,#23156,#23157,
#23158,#23159,#23160,#23161,#23162,#23163,#23164,#23165,#23166,#23167,#23168,
#23169,#23170,#23171,#23172,#23173,#23174,#23175,#23176,#23177,#23178,#23179,
#23180,#23181,#23182,#23183,#23184,#23185,#23186,#23187,#23188,#23189,#23190,
#23191,#23192,#23193,#23194,#23195,#23196,#23197,#23198,#23199,#23200,#23201,
#23202,#23203,#23204,#23205,#23206,#23207,#23208,#23209,#23210,#23211,#23212,
#23213,#23214,#23215,#23216,#23217,#23218,#23219,#23220,#23221,#23222,#23223,
#23224,#23225,#23226,#23227,#23228,#23229,#23230,#23231,#23232,#23233,#23234,
#23235,#23236,#23237,#23238,#23239,#23240,#23241,#23242,#23243,#23244,#23245,
#23246,#23247,#23248,#23249,#23250,#23251,#23252,#23253,#23254,#23255,#23256,
#23257,#23258,#23259,#23260,#23261,#23262,#23263,#23264,#23265,#23266,#23267,
#23268,#23269,#23270,#23271,#23272,#23273,#23274,#23275,#23276,#23277,#23278,
#23279,#23280,#23281,#23282,#23283,#23284,#23285,#23286,#23287,#23288,#23289,
#23290),.UNSPECIFIED.,.F.,.F.,(4,3,3,3,3,3,3,3,3,3,3,3,3,3,3,3,3,3,3,3,
3,3,3,3,3,3,3,3,3,3,3,3,3,3,3,3,3,3,3,3,3,3,3,3,3,3,3,3,3,3,3,3,3,3,3,3,
3,3,3,3,3,3,3,3,3,3,3,3,3,3,3,3,3,3,3,4),(58.7391042641703,58.8335838703561,
58.9284005420665,59.0233890466834,59.118661083167,59.1876091645181,59.2762538660009,
59.3647855821298,59.4532279897729,59.5441252211755,59.6324686487407,59.7207994986245,
59.8091390319831,59.9019557342358,59.9904271252048,60.0789594252534,60.167617269212,
60.1804058409936,60.2690236889587,60.3575281040159,60.445942799225,60.5368502640056,
60.6251651334518,60.7134671602168,60.8017776362361,60.8946338565443,60.9830758657094,
61.0715786752344,61.1602070510044,61.1732025174692,61.2618353276175,61.3503548850479,
61.4387848830728,61.5296866719318,61.6180171444911,61.7063348587903,61.7946610897492,
61.8874956157981,61.9759534045469,62.064472000353,62.1531160770312,62.1659991939448,
62.2546305549895,62.3431486768587,62.4315772546133,62.5224795815892,62.6108086815575,
62.6991250435169,62.7874499439978,62.8802864256034,62.9687429518561,63.0572603088198,
63.1459031878398,63.1587958704204,63.2474242637227,63.3359393650657,63.4243648735262,
63.5152683326974,63.6035942616666,63.6919074202865,63.7802290884916,63.8730699530927,
63.961523203636,64.0500372702589,64.1386768578591,64.1515925468959,64.23900867765,
64.3263123945337,64.4135197963484,64.500673816494,64.5877968757005,64.674911363053,
64.7620861803452,64.849289012654,64.9366137069396,65.0222893385667),
 .UNSPECIFIED.);
#1446=B_SPLINE_CURVE_WITH_KNOTS('',3,(#23292,#23293,#23294,#23295,#23296,
#23297,#23298,#23299,#23300,#23301,#23302,#23303,#23304,#23305,#23306,#23307,
#23308,#23309,#23310,#23311,#23312,#23313,#23314,#23315,#23316,#23317,#23318,
#23319,#23320,#23321,#23322,#23323,#23324,#23325,#23326,#23327,#23328,#23329,
#23330,#23331,#23332,#23333,#23334,#23335,#23336,#23337,#23338,#23339,#23340,
#23341,#23342,#23343,#23344,#23345,#23346,#23347,#23348,#23349,#23350,#23351,
#23352,#23353,#23354,#23355,#23356,#23357,#23358,#23359,#23360,#23361,#23362,
#23363,#23364,#23365,#23366,#23367,#23368,#23369,#23370,#23371,#23372,#23373,
#23374,#23375,#23376,#23377,#23378,#23379,#23380,#23381,#23382,#23383,#23384,
#23385,#23386,#23387,#23388,#23389,#23390,#23391,#23392,#23393,#23394,#23395,
#23396,#23397,#23398,#23399,#23400,#23401,#23402,#23403,#23404,#23405,#23406,
#23407,#23408,#23409,#23410,#23411,#23412,#23413,#23414,#23415,#23416,#23417,
#23418,#23419,#23420,#23421,#23422,#23423,#23424,#23425,#23426,#23427,#23428,
#23429,#23430,#23431,#23432,#23433,#23434,#23435,#23436,#23437,#23438,#23439,
#23440,#23441,#23442,#23443,#23444,#23445,#23446,#23447,#23448,#23449,#23450,
#23451,#23452,#23453,#23454,#23455,#23456,#23457,#23458,#23459,#23460,#23461,
#23462,#23463,#23464,#23465,#23466,#23467,#23468,#23469,#23470,#23471,#23472,
#23473,#23474,#23475,#23476,#23477,#23478,#23479,#23480,#23481,#23482,#23483,
#23484,#23485,#23486,#23487,#23488,#23489,#23490,#23491,#23492,#23493,#23494,
#23495,#23496,#23497,#23498,#23499,#23500,#23501,#23502,#23503,#23504,#23505,
#23506,#23507,#23508,#23509,#23510,#23511,#23512,#23513,#23514,#23515,#23516,
#23517),.UNSPECIFIED.,.F.,.F.,(4,3,3,3,3,3,3,3,3,3,3,3,3,3,3,3,3,3,3,3,
3,3,3,3,3,3,3,3,3,3,3,3,3,3,3,3,3,3,3,3,3,3,3,3,3,3,3,3,3,3,3,3,3,3,3,3,
3,3,3,3,3,3,3,3,3,3,3,3,3,3,3,3,3,3,3,4),(65.0222893387811,65.1443892233715,
65.2330192623953,65.3215360342572,65.4099632358317,65.5008660688337,65.5891937362466,
65.6775086471462,65.7658320795859,65.8586705346512,65.9471255633786,66.0356414128,
66.1242827790579,66.1371858998471,66.2258156272582,66.3143320814836,66.402758959822,
66.4936619118846,66.58198924419,66.670303816145,66.7586269061608,66.8514658237013,
66.9399205043519,67.028436003783,67.1170770194266,67.1299825763227,67.2186125609608,
67.3071292758913,67.3955564180708,67.4864592724117,67.5747868746579,67.6631017183513,
67.7514250816097,67.8442636244069,67.9327185795769,68.0212343539367,68.1098756434391,
68.1227792527983,68.2114091748451,68.2999258267928,68.3883529056791,68.4792557836284,
68.5675833222237,68.6558981022458,68.7442214018833,68.8370600337309,68.9255149260015,
69.0140306377185,69.1026718653213,69.1155759292738,69.2042058209554,69.2927224418782,
69.3811494891212,69.4720523786998,69.5603798843147,69.6486946309156,69.7370178967264,
69.8298565739821,69.9183114317098,70.0068271086403,70.0954683013184,70.1083726057494,
70.1970025297981,70.2855191835478,70.3739462640343,70.4648491413082,70.5531766809891,
70.6414914619027,70.7298147622357,70.822653392233,70.9111082846938,70.9996239964263,
71.0882652237953,71.101169282225,71.2256508576449,71.3054746459608),
 .UNSPECIFIED.);
#1447=B_SPLINE_CURVE_WITH_KNOTS('',3,(#23519,#23520,#23521,#23522,#23523,
#23524,#23525,#23526,#23527,#23528,#23529,#23530,#23531,#23532,#23533,#23534,
#23535,#23536,#23537,#23538,#23539,#23540,#23541,#23542,#23543,#23544,#23545,
#23546,#23547,#23548,#23549,#23550,#23551,#23552,#23553,#23554,#23555,#23556,
#23557,#23558,#23559,#23560,#23561,#23562,#23563,#23564,#23565,#23566,#23567,
#23568,#23569,#23570,#23571,#23572,#23573,#23574,#23575,#23576,#23577,#23578,
#23579,#23580,#23581,#23582,#23583,#23584,#23585,#23586,#23587,#23588,#23589,
#23590,#23591,#23592,#23593,#23594,#23595,#23596,#23597,#23598,#23599,#23600,
#23601,#23602,#23603,#23604,#23605,#23606,#23607,#23608,#23609,#23610,#23611,
#23612,#23613,#23614,#23615,#23616,#23617,#23618,#23619,#23620,#23621,#23622,
#23623,#23624,#23625,#23626,#23627,#23628,#23629,#23630,#23631,#23632,#23633,
#23634,#23635,#23636,#23637,#23638,#23639,#23640,#23641,#23642,#23643,#23644,
#23645,#23646,#23647,#23648,#23649,#23650,#23651,#23652,#23653,#23654,#23655,
#23656,#23657,#23658,#23659,#23660,#23661,#23662,#23663,#23664,#23665,#23666,
#23667,#23668,#23669,#23670,#23671,#23672,#23673,#23674,#23675,#23676,#23677,
#23678,#23679,#23680,#23681,#23682,#23683,#23684,#23685,#23686,#23687,#23688,
#23689,#23690,#23691,#23692,#23693,#23694,#23695,#23696,#23697,#23698,#23699,
#23700,#23701,#23702,#23703,#23704,#23705,#23706,#23707,#23708,#23709,#23710,
#23711,#23712,#23713,#23714,#23715,#23716,#23717,#23718,#23719,#23720,#23721,
#23722,#23723,#23724,#23725,#23726,#23727,#23728,#23729,#23730,#23731,#23732,
#23733,#23734,#23735,#23736,#23737,#23738,#23739,#23740,#23741,#23742,#23743,
#23744),.UNSPECIFIED.,.F.,.F.,(4,3,3,3,3,3,3,3,3,3,3,3,3,3,3,3,3,3,3,3,
3,3,3,3,3,3,3,3,3,3,3,3,3,3,3,3,3,3,3,3,3,3,3,3,3,3,3,3,3,3,3,3,3,3,3,3,
3,3,3,3,3,3,3,3,3,3,3,3,3,3,3,3,3,3,3,4),(71.3054746461005,71.3926937178224,
71.4803527479322,71.56745629258,71.654541925881,71.7416320525193,71.8297155290647,
71.9169275868896,72.0054467727951,72.0939659587006,72.1825958700471,72.27111251094,
72.3595395784323,72.4504424605253,72.5387699869533,72.6270847545411,72.7154080414897,
72.8082466899113,72.8967015689638,72.9852172672815,73.0738584813068,73.0867626351761,
73.1753925504875,73.2639091954045,73.3523362669747,73.4432391475593,73.5315666781729,
73.619881449979,73.7082047411741,73.8010433837935,73.8894982671248,73.9780139697316,
74.0666551880355,74.0795593116517,74.1681892254449,74.2567058688284,74.3451329388519,
74.4360358200113,74.5243633490555,74.6126781192865,74.7010014089025,74.7938400537087,
74.8822949354655,74.9708106365,75.0594518532432,75.0723559881273,75.1609859017548,
75.2495025449661,75.3379296148109,75.4288324960349,75.5171600248858,75.6054747949184,
75.6937980843313,75.7866367293992,75.8750916109423,75.9636073117593,76.0522485282809,
76.0651526646029,76.1537825787065,76.242299222401,76.330726292736,76.4216291737788,
76.5099567031338,76.5982714736746,76.6865947635996,76.7794334079693,76.8678882900288,
76.9564039913636,77.0450452084028,77.0579493410785,77.149780829808,77.2414655319119,
77.3329735006271,77.424377476035,77.5156633354471,77.5886599531404),
 .UNSPECIFIED.);
#1448=B_SPLINE_CURVE_WITH_KNOTS('',3,(#23746,#23747,#23748,#23749,#23750,
#23751,#23752,#23753,#23754,#23755,#23756,#23757,#23758,#23759,#23760,#23761,
#23762,#23763,#23764,#23765,#23766,#23767,#23768,#23769,#23770,#23771,#23772,
#23773,#23774,#23775,#23776,#23777,#23778,#23779,#23780,#23781,#23782,#23783,
#23784,#23785,#23786,#23787,#23788,#23789,#23790,#23791,#23792,#23793,#23794,
#23795,#23796,#23797,#23798,#23799,#23800,#23801,#23802,#23803,#23804,#23805,
#23806,#23807,#23808,#23809,#23810,#23811,#23812,#23813,#23814,#23815,#23816,
#23817,#23818,#23819,#23820,#23821,#23822,#23823,#23824,#23825,#23826,#23827,
#23828,#23829,#23830,#23831,#23832,#23833,#23834,#23835,#23836,#23837,#23838,
#23839,#23840,#23841,#23842,#23843,#23844,#23845,#23846,#23847,#23848,#23849,
#23850,#23851,#23852,#23853,#23854,#23855,#23856,#23857,#23858,#23859,#23860,
#23861,#23862,#23863,#23864,#23865,#23866,#23867,#23868,#23869,#23870,#23871,
#23872,#23873,#23874,#23875,#23876,#23877,#23878,#23879,#23880,#23881,#23882,
#23883,#23884,#23885,#23886,#23887,#23888,#23889,#23890,#23891,#23892,#23893,
#23894,#23895,#23896,#23897,#23898,#23899,#23900,#23901,#23902,#23903,#23904,
#23905,#23906,#23907,#23908,#23909,#23910,#23911,#23912,#23913,#23914,#23915,
#23916,#23917,#23918,#23919,#23920,#23921,#23922,#23923,#23924,#23925,#23926,
#23927,#23928,#23929,#23930,#23931,#23932,#23933,#23934,#23935,#23936,#23937,
#23938,#23939,#23940,#23941,#23942,#23943,#23944,#23945,#23946,#23947,#23948,
#23949,#23950,#23951,#23952,#23953,#23954,#23955,#23956,#23957,#23958,#23959,
#23960,#23961,#23962,#23963,#23964,#23965,#23966,#23967,#23968,#23969,#23970,
#23971),.UNSPECIFIED.,.F.,.F.,(4,3,3,3,3,3,3,3,3,3,3,3,3,3,3,3,3,3,3,3,
3,3,3,3,3,3,3,3,3,3,3,3,3,3,3,3,3,3,3,3,3,3,3,3,3,3,3,3,3,3,3,3,3,3,3,3,
3,3,3,3,3,3,3,3,3,3,3,3,3,3,3,3,3,3,3,4),(77.5886599533119,77.6825471555259,
77.7767398883194,77.8710860075021,77.9657069232752,78.050746017554,78.1393759314319,
78.227892574898,78.3163196450021,78.4072225261305,78.495550055249,78.5838648255518,
78.6721881152372,78.7650267599353,78.8534816417544,78.9419973428485,79.0306385596478,
79.0435426940296,79.1321726079931,79.2206892515459,79.3091163217373,79.4000192028333,
79.4883467320409,79.5766615024333,79.6649847922087,79.7578234367828,79.8462783186919,
79.9347940198762,80.0234352367649,80.0363393705052,80.1249692843794,80.2134859278426,
80.3019129979443,80.3928158790738,80.4811434081918,80.5694581784947,80.6577814681809,
80.7506201128808,80.8390749947023,80.9275906957994,81.0162319126024,81.0291360469808,
81.117765960863,81.2062826043335,81.294709674442,81.3856125555688,81.4739400846921,
81.5622548549999,81.6505781446904,81.7434167893819,81.8318716712063,81.9203873723059,
82.0090285891106,82.0219327234563,82.1105626375695,82.199079281272,82.2875063516133,
82.3784092326531,82.4667367620094,82.5550515325498,82.6433748224724,82.7362134668373,
82.8246683488902,82.913184050217,83.0018252672459,83.0147293999319,83.1020973209263,
83.1893527800484,83.2765115668103,83.3636169079208,83.4506912588376,83.5377570429396,
83.6248803500429,83.7120318592111,83.7992975896713,83.8718452601179),
 .UNSPECIFIED.);
#1449=B_SPLINE_CURVE_WITH_KNOTS('',3,(#23973,#23974,#23975,#23976,#23977,
#23978,#23979,#23980,#23981,#23982,#23983,#23984,#23985,#23986,#23987,#23988,
#23989,#23990,#23991,#23992,#23993,#23994,#23995,#23996,#23997,#23998,#23999,
#24000,#24001,#24002,#24003,#24004,#24005,#24006,#24007,#24008,#24009,#24010,
#24011,#24012,#24013,#24014,#24015,#24016,#24017,#24018,#24019,#24020,#24021,
#24022,#24023,#24024,#24025,#24026,#24027,#24028,#24029,#24030,#24031,#24032,
#24033,#24034,#24035,#24036,#24037,#24038,#24039,#24040,#24041,#24042,#24043,
#24044,#24045,#24046,#24047,#24048,#24049,#24050,#24051,#24052,#24053,#24054,
#24055,#24056,#24057,#24058,#24059,#24060,#24061,#24062,#24063,#24064,#24065,
#24066,#24067,#24068,#24069,#24070,#24071,#24072,#24073,#24074,#24075,#24076,
#24077,#24078,#24079,#24080,#24081,#24082,#24083,#24084,#24085,#24086,#24087,
#24088,#24089,#24090,#24091,#24092,#24093,#24094,#24095,#24096,#24097,#24098,
#24099,#24100,#24101,#24102,#24103,#24104,#24105,#24106,#24107,#24108,#24109,
#24110,#24111,#24112,#24113,#24114,#24115,#24116,#24117,#24118,#24119,#24120,
#24121,#24122,#24123,#24124,#24125,#24126,#24127,#24128,#24129,#24130,#24131,
#24132,#24133,#24134,#24135,#24136,#24137,#24138,#24139,#24140,#24141,#24142,
#24143,#24144,#24145,#24146,#24147,#24148,#24149,#24150,#24151,#24152,#24153,
#24154,#24155,#24156,#24157,#24158,#24159,#24160,#24161,#24162,#24163,#24164,
#24165,#24166,#24167,#24168,#24169,#24170,#24171,#24172,#24173,#24174,#24175,
#24176,#24177,#24178,#24179,#24180,#24181,#24182,#24183,#24184,#24185,#24186,
#24187,#24188,#24189,#24190,#24191,#24192,#24193,#24194,#24195,#24196,#24197,
#24198),.UNSPECIFIED.,.F.,.F.,(4,3,3,3,3,3,3,3,3,3,3,3,3,3,3,3,3,3,3,3,
3,3,3,3,3,3,3,3,3,3,3,3,3,3,3,3,3,3,3,3,3,3,3,3,3,3,3,3,3,3,3,3,3,3,3,3,
3,3,3,3,3,3,3,3,3,3,3,3,3,3,3,3,3,3,3,4),(83.87184526032,84.0075260764075,
84.0961559902256,84.1846726336294,84.2730997036684,84.3640025848202,84.452330113868,
84.540644884098,84.6289681737088,84.7218068185024,84.8102617002428,84.8987774012569,
84.9874186179747,85.0003227528831,85.0889526682576,85.1774693132255,85.2658963848344,
85.3567992654,85.4451267960223,85.5334415678257,85.621764859007,85.7146035015949,
85.8030583848844,85.8915740874398,85.980215305679,85.9931194293586,86.0817493404684,
86.1702659811702,86.2586930485167,86.3495959306814,86.4379234570766,86.5262382246736,
86.6145615116734,86.7074001602136,86.7958550394226,86.884370737933,86.973011952201,
86.9859161058342,87.074546020048,87.163062663826,87.2514897342175,87.342392615229,
87.4307201445741,87.5190349150805,87.6073582049465,87.7001968492873,87.7886517312281,
87.8771674324237,87.9658086492954,87.9787127823098,88.0673427067238,88.1558593607685,
88.2442864414803,88.3351893186435,88.423516858375,88.5118316392743,88.6001549395281,
88.6929935693425,88.7814484615617,88.8699641729969,88.9586053999911,88.9715094587854,
89.0601393486193,89.1486559680495,89.2370830141535,89.3279859042919,89.4163134096509,
89.504628156324,89.5929514225349,89.6857901007164,89.7742449596661,89.8627606381013,
89.9514018326752,89.964306135261,90.0930929644909,90.1550305674995),
 .UNSPECIFIED.);
#1450=B_SPLINE_CURVE_WITH_KNOTS('',3,(#24200,#24201,#24202,#24203,#24204,
#24205,#24206,#24207,#24208,#24209,#24210,#24211,#24212,#24213,#24214,#24215,
#24216,#24217,#24218,#24219,#24220,#24221,#24222,#24223,#24224,#24225,#24226,
#24227,#24228,#24229,#24230,#24231,#24232,#24233,#24234,#24235,#24236,#24237,
#24238,#24239,#24240,#24241,#24242,#24243,#24244,#24245,#24246,#24247,#24248,
#24249,#24250,#24251,#24252,#24253,#24254,#24255,#24256,#24257,#24258,#24259,
#24260,#24261,#24262,#24263,#24264,#24265,#24266,#24267,#24268,#24269,#24270,
#24271,#24272,#24273,#24274,#24275,#24276,#24277,#24278,#24279,#24280,#24281,
#24282,#24283,#24284,#24285,#24286,#24287,#24288,#24289,#24290,#24291,#24292,
#24293,#24294,#24295,#24296,#24297,#24298,#24299,#24300,#24301,#24302,#24303,
#24304,#24305,#24306,#24307,#24308,#24309,#24310,#24311,#24312,#24313,#24314,
#24315,#24316,#24317,#24318,#24319,#24320,#24321,#24322,#24323,#24324,#24325,
#24326,#24327,#24328,#24329,#24330,#24331,#24332,#24333,#24334,#24335,#24336,
#24337,#24338,#24339,#24340,#24341,#24342,#24343,#24344,#24345,#24346,#24347,
#24348,#24349,#24350,#24351,#24352,#24353,#24354,#24355,#24356,#24357,#24358,
#24359,#24360,#24361,#24362,#24363,#24364,#24365,#24366,#24367,#24368,#24369,
#24370,#24371,#24372,#24373,#24374,#24375,#24376,#24377,#24378,#24379,#24380,
#24381,#24382,#24383,#24384,#24385,#24386,#24387,#24388,#24389,#24390,#24391,
#24392,#24393,#24394,#24395,#24396,#24397,#24398,#24399,#24400,#24401,#24402,
#24403,#24404,#24405,#24406,#24407,#24408,#24409,#24410,#24411,#24412,#24413,
#24414,#24415,#24416,#24417,#24418,#24419,#24420,#24421,#24422,#24423,#24424,
#24425,#24426,#24427,#24428),.UNSPECIFIED.,.F.,.F.,(4,3,3,3,3,3,3,3,3,3,
3,3,3,3,3,3,3,3,3,3,3,3,3,3,3,3,3,3,3,3,3,3,3,3,3,3,3,3,3,3,3,3,3,3,3,3,
3,3,3,3,3,3,3,3,3,3,3,3,3,3,3,3,3,3,3,3,3,3,3,3,3,3,3,3,3,3,4),(90.1550305677032,
90.2422286500628,90.331587920272,90.4186598142627,90.5057103608812,90.5927619928027,
90.6838471975362,90.7710171033747,90.8582443197431,90.9455937102727,90.9571028117365,
91.0457327981164,91.1342495144537,91.2226766577066,91.3135795115198,91.4019071140074,
91.4902219576328,91.578545320514,91.6713838624385,91.7598388164566,91.8483545893981,
91.9369958771135,91.9498994882121,92.0385292015879,92.1270456444749,92.2154725141616,
92.3063754704774,92.394702800838,92.4830173733404,92.5713404663955,92.6641793909685,
92.7526340809014,92.8411495917615,92.929790621805,92.9426961646877,93.0313262273738,
93.1198430183502,93.2082702345105,93.2991730603421,93.3875007310339,93.4758156410106,
93.5641390683264,93.6569775115356,93.745432524614,93.8339483547674,93.9225896967489,
93.9354928411633,94.02412322868,94.1126403489231,94.2010678983342,94.2919706007473,
94.3802986123506,94.4686138654714,94.5569376377754,94.6497756077413,94.7382309671927,
94.8267471441431,94.9153888314088,94.9282895176388,95.0169178075138,95.1054328253063,
95.1938582700114,95.2847617605242,95.3730876751616,95.461400837815,95.5497225284144,
95.6425634448394,95.7310167637837,95.8195309146251,95.9081706083371,95.9210861941144,
96.0134105729702,96.1055811446663,96.1975615385315,96.2894289573287,96.3811619125729,
96.4382158746791),.UNSPECIFIED.);
#1451=B_SPLINE_CURVE_WITH_KNOTS('',3,(#24429,#24430,#24431,#24432,#24433,
#24434,#24435,#24436,#24437,#24438,#24439,#24440,#24441,#24442,#24443,#24444,
#24445,#24446,#24447,#24448,#24449,#24450,#24451,#24452,#24453,#24454,#24455,
#24456,#24457,#24458,#24459,#24460,#24461,#24462,#24463,#24464,#24465,#24466,
#24467,#24468,#24469,#24470,#24471,#24472,#24473,#24474,#24475,#24476,#24477,
#24478,#24479,#24480,#24481,#24482,#24483,#24484,#24485,#24486,#24487,#24488,
#24489,#24490,#24491,#24492,#24493,#24494,#24495,#24496,#24497,#24498,#24499,
#24500,#24501,#24502,#24503,#24504,#24505,#24506,#24507,#24508,#24509,#24510,
#24511,#24512,#24513,#24514,#24515,#24516,#24517,#24518,#24519,#24520,#24521,
#24522,#24523,#24524,#24525,#24526,#24527,#24528,#24529,#24530,#24531,#24532,
#24533,#24534,#24535,#24536,#24537,#24538,#24539,#24540,#24541,#24542,#24543,
#24544,#24545,#24546,#24547,#24548,#24549,#24550,#24551,#24552,#24553,#24554,
#24555,#24556,#24557,#24558,#24559,#24560,#24561,#24562,#24563,#24564,#24565,
#24566,#24567,#24568,#24569,#24570,#24571,#24572,#24573,#24574,#24575,#24576,
#24577,#24578,#24579,#24580,#24581,#24582,#24583,#24584,#24585,#24586,#24587,
#24588,#24589,#24590,#24591,#24592,#24593,#24594,#24595,#24596,#24597,#24598,
#24599,#24600,#24601,#24602,#24603,#24604,#24605,#24606,#24607,#24608,#24609,
#24610,#24611,#24612,#24613,#24614,#24615,#24616,#24617,#24618,#24619,#24620,
#24621,#24622,#24623,#24624,#24625,#24626,#24627,#24628,#24629,#24630,#24631,
#24632,#24633,#24634,#24635,#24636,#24637,#24638,#24639,#24640,#24641,#24642,
#24643,#24644,#24645,#24646,#24647,#24648,#24649,#24650,#24651,#24652,#24653,
#24654),.UNSPECIFIED.,.F.,.F.,(4,3,3,3,3,3,3,3,3,3,3,3,3,3,3,3,3,3,3,3,
3,3,3,3,3,3,3,3,3,3,3,3,3,3,3,3,3,3,3,3,3,3,3,3,3,3,3,3,3,3,3,3,3,3,3,3,
3,3,3,3,3,3,3,3,3,3,3,3,3,3,3,3,3,3,3,4),(96.43821587489,96.5315094285364,
96.6271027890498,96.7208092089047,96.8173460397473,96.91388287059,97.0025156379104,
97.0910351607441,97.1794651323696,97.2703669342066,97.3586974008322,97.447015116803,
97.5353413570371,97.6281759045442,97.7166337216183,97.8051523522997,97.8937964729189,
97.9066795470656,97.9952966599497,98.0838004811807,98.1722147232329,98.2631224107714,
98.3514371783157,98.4397392336869,98.5280498687933,98.6209064574802,98.7093489527241,
98.7978523607349,98.8864814906074,98.8994762235411,98.9881227028305,99.0766558550366,
99.1650993584394,99.2559960511365,99.3443397248907,99.4326705052216,99.5210096533517,
99.613825465018,99.7022956800214,99.7908265321604,99.8794825519452,99.8922729000167,
99.9809176811722,100.069449400606,100.157891734552,100.248788964794,100.337132121611,
100.425462626552,100.513801739934,100.606618699073,100.695089479045,100.783621101387,
100.872278175145,100.885069576492,100.973601443402,101.062019817221,101.150348512407,
101.241288229977,101.329517737987,101.417734784873,101.505960752869,101.594217025517,
101.682573743482,101.770990913672,101.859536359584,101.877866252968,101.965380714648,
102.052782232462,102.14008559453,102.227334731498,102.314552007684,102.401759755091,
102.489020034314,102.576307694746,102.663699300999,102.721401181691),
 .UNSPECIFIED.);
#1452=B_SPLINE_CURVE_WITH_KNOTS('',3,(#24657,#24658,#24659,#24660,#24661,
#24662,#24663,#24664,#24665,#24666,#24667,#24668,#24669,#24670,#24671,#24672,
#24673,#24674,#24675,#24676,#24677,#24678,#24679,#24680,#24681,#24682,#24683,
#24684,#24685,#24686,#24687,#24688,#24689,#24690,#24691,#24692,#24693,#24694,
#24695,#24696,#24697,#24698,#24699,#24700,#24701,#24702,#24703,#24704,#24705,
#24706,#24707,#24708,#24709,#24710,#24711,#24712,#24713,#24714,#24715,#24716,
#24717,#24718,#24719,#24720,#24721,#24722,#24723,#24724,#24725,#24726,#24727,
#24728,#24729,#24730,#24731,#24732,#24733,#24734,#24735,#24736,#24737,#24738,
#24739,#24740,#24741,#24742,#24743,#24744,#24745,#24746,#24747,#24748,#24749,
#24750,#24751,#24752,#24753,#24754,#24755,#24756,#24757,#24758,#24759,#24760,
#24761,#24762,#24763,#24764,#24765,#24766,#24767,#24768,#24769,#24770,#24771,
#24772,#24773,#24774,#24775,#24776,#24777,#24778,#24779,#24780,#24781,#24782,
#24783,#24784),.UNSPECIFIED.,.F.,.F.,(4,2,2,2,2,2,2,2,2,2,2,2,2,2,2,2,2,
2,2,2,2,2,2,2,2,2,2,2,2,2,2,2,2,2,2,2,2,2,2,2,2,2,2,2,2,2,2,2,2,2,2,2,2,
2,2,2,2,2,2,2,2,2,2,4),(0.00539620386092574,0.0581762748395569,0.0959465799780152,
0.114155907866814,0.129776929780304,0.14055985506542,0.150346261073067,
0.16647834135212,0.237291353387592,0.267515101724101,0.280511188113101,
0.290873769283408,0.297218081100971,0.303663604114955,0.314768974021879,
0.370321305386931,0.424463887562305,0.443465444336362,0.454819404756714,
0.465338872506723,0.479704411904614,0.516399202169655,0.57761423998528,
0.604512541065404,0.61325634689013,0.619213408423627,0.626006074952694,
0.639135832994514,0.699879326694402,0.753414703569547,0.76852834728937,
0.779073894490983,0.790001188858396,0.807203307949951,0.870090824473551,
0.923376749124762,0.933196757388839,0.939316960334243,0.945722527967118,
0.956813247809548,1.01214832155096,1.05354584725591,1.07260368326006,1.08870839604174,
1.09948989162646,1.11031322198308,1.12664871539946,1.19803286914717,1.22931305578496,
1.24254347292066,1.25301844025526,1.25930840592584,1.26559972502294,1.27612086586066,
1.33807763094068,1.39465125576289,1.40991623036985,1.42053776130304,1.43152512354768,
1.4487957670082,1.50163948973854,1.54490804705874,1.56065504609305,1.57246993836349),
 .UNSPECIFIED.);
#1453=B_SPLINE_CURVE_WITH_KNOTS('',3,(#24788,#24789,#24790,#24791,#24792,
#24793,#24794,#24795,#24796,#24797,#24798,#24799,#24800,#24801,#24802,#24803,
#24804,#24805,#24806,#24807,#24808,#24809,#24810,#24811,#24812,#24813,#24814,
#24815,#24816,#24817,#24818,#24819,#24820,#24821,#24822,#24823,#24824,#24825,
#24826,#24827,#24828,#24829,#24830,#24831,#24832,#24833,#24834,#24835,#24836,
#24837,#24838,#24839,#24840,#24841,#24842,#24843,#24844,#24845,#24846,#24847,
#24848,#24849,#24850,#24851,#24852,#24853,#24854,#24855,#24856,#24857,#24858,
#24859,#24860),.UNSPECIFIED.,.F.,.F.,(4,3,3,3,3,3,3,3,3,3,3,3,3,3,3,3,3,
3,3,3,3,3,3,3,4),(-47.1238898038469,-46.9950727644704,-46.9016897087544,
-46.8093989437482,-46.717232941916,-46.6251631638475,-46.5331552357951,
-46.4411785207822,-46.3492073946448,-46.2572162437137,-46.1651145240901,
-46.0729548859248,-45.9806268533618,-45.9088930322787,-45.8132628505972,
-45.71777443611,-45.6175646760721,-45.5223118547511,-45.4271236077411,-45.3319796663271,
-45.2368598072655,-45.1417182743927,-45.046565882262,-44.9513501488818,
-44.9160963558065),.UNSPECIFIED.);
#1454=B_SPLINE_CURVE_WITH_KNOTS('',3,(#24861,#24862,#24863,#24864,#24865,
#24866,#24867,#24868,#24869,#24870,#24871,#24872,#24873,#24874,#24875,#24876,
#24877,#24878,#24879,#24880,#24881,#24882,#24883,#24884,#24885,#24886,#24887,
#24888,#24889,#24890,#24891,#24892,#24893,#24894,#24895,#24896,#24897,#24898,
#24899,#24900),.UNSPECIFIED.,.F.,.F.,(4,2,2,2,2,2,2,2,2,2,2,2,2,2,2,2,2,
2,2,4),(-4.06042171078719,-3.99441154909979,-3.97878930540769,-3.96800786165842,
-3.95822415119664,-3.94210020820236,-3.87130478593638,-3.84103412307938,
-3.8280268247646,-3.81765891600555,-3.81131440486851,-3.80487196973302,
-3.79377772423557,-3.73802395486263,-3.67705048918811,-3.66158326588681,
-3.65088958922245,-3.63987943928295,-3.62267948655661,-3.60215374024631),
 .UNSPECIFIED.);
#1455=B_SPLINE_CURVE_WITH_KNOTS('',3,(#24948,#24949,#24950,#24951,#24952,
#24953,#24954,#24955,#24956,#24957,#24958,#24959,#24960,#24961),
 .UNSPECIFIED.,.F.,.F.,(4,2,2,2,2,2,4),(-0.361085602979245,-0.357000077685616,
-0.27844614120804,-0.199252098686416,-0.109491424797441,-0.0546153104605399,
-1.74415845322073E-7),.UNSPECIFIED.);
#1456=B_SPLINE_CURVE_WITH_KNOTS('',3,(#24963,#24964,#24965,#24966,#24967,
#24968,#24969,#24970,#24971),.UNSPECIFIED.,.F.,.F.,(4,1,1,1,1,1,4),(-0.0350009483246411,
-0.0280198882249107,-0.016804534164689,-0.00558918010446727,0.00562617395575443,
0.0280568820761978,0.0350536140949925),.UNSPECIFIED.);
#1457=B_SPLINE_CURVE_WITH_KNOTS('',3,(#24973,#24974,#24975,#24976,#24977,
#24978,#24979,#24980,#24981,#24982,#24983,#24984,#24985,#24986),
 .UNSPECIFIED.,.F.,.F.,(4,2,2,2,2,2,4),(-0.469080395753844,-0.397348524872784,
-0.325269326748868,-0.207248260222546,-0.103131005525517,0.,0.00535949284075881),
 .UNSPECIFIED.);
#1458=B_SPLINE_CURVE_WITH_KNOTS('',3,(#24997,#24998,#24999,#25000,#25001,
#25002,#25003,#25004,#25005,#25006,#25007,#25008,#25009,#25010,#25011,#25012,
#25013,#25014,#25015,#25016,#25017,#25018,#25019,#25020,#25021,#25022,#25023,
#25024,#25025,#25026,#25027,#25028,#25029,#25030,#25031,#25032,#25033,#25034,
#25035,#25036,#25037,#25038,#25039,#25040,#25041,#25042,#25043,#25044,#25045),
 .UNSPECIFIED.,.F.,.F.,(4,3,3,3,3,3,3,3,3,3,3,3,3,3,3,3,4),(-0.0350029095584539,
-0.0326784650318294,-0.03034917662837,-0.0280198882249105,-0.0254680596894552,
-0.0229200914464411,-0.0203748859852383,-0.0178336153267085,-0.0168045341646888,
-0.0144744152626023,-0.0121456081055165,-0.00981763332868959,-0.00748893840388418,
-0.00558918010446715,-0.00301830868335975,-0.000444599004916765,-5.90823278986403E-12),
 .UNSPECIFIED.);
#1459=B_SPLINE_CURVE_WITH_KNOTS('',3,(#25048,#25049,#25050,#25051,#25052,
#25053),.UNSPECIFIED.,.F.,.F.,(4,2,4),(-0.954074778386004,-0.905023768660029,
-0.855972758934053),.UNSPECIFIED.);
#1460=B_SPLINE_CURVE_WITH_KNOTS('',3,(#25055,#25056,#25057,#25058,#25059,
#25060,#25061),.UNSPECIFIED.,.F.,.F.,(4,3,4),(-0.0490510097259763,0.,0.0490510097259751),
 .UNSPECIFIED.);
#1461=B_SPLINE_CURVE_WITH_KNOTS('',3,(#25064,#25065,#25066,#25067,#25068,
#25069,#25070,#25071,#25072,#25073,#25074,#25075,#25076,#25077,#25078,#25079,
#25080,#25081,#25082,#25083,#25084,#25085,#25086,#25087,#25088,#25089,#25090,
#25091,#25092,#25093,#25094,#25095,#25096,#25097,#25098,#25099,#25100,#25101,
#25102,#25103,#25104,#25105,#25106,#25107,#25108,#25109,#25110,#25111,#25112),
 .UNSPECIFIED.,.F.,.F.,(4,3,3,3,3,3,3,3,3,3,3,3,3,3,3,3,4),(3.46944695195361E-18,
0.00256903169244048,0.00514025006054238,0.00562617395575452,0.00815140445096736,
0.0106763863582272,0.0132007974759858,0.0157247394590576,0.0168415280159762,
0.0191777755034903,0.0215148133424174,0.0238521887988676,0.0261921437071731,
0.0280568820761979,0.0305976323694871,0.033145591663878,0.0350439246442522),
 .UNSPECIFIED.);
#1462=B_SPLINE_CURVE_WITH_KNOTS('',3,(#25167,#25168,#25169,#25170,#25171,
#25172,#25173,#25174,#25175,#25176,#25177,#25178,#25179,#25180),
 .UNSPECIFIED.,.F.,.F.,(4,2,2,2,2,2,4),(-0.00536726751032349,-9.33357504392246E-9,
0.103199017039813,0.207237213246338,0.325156745312053,0.39724917198956,
0.468998855549633),.UNSPECIFIED.);
#1463=B_SPLINE_CURVE_WITH_KNOTS('',3,(#25182,#25183,#25184,#25185,#25186,
#25187,#25188,#25189,#25190,#25191,#25192,#25193,#25194,#25195),
 .UNSPECIFIED.,.F.,.F.,(4,2,2,2,2,2,4),(1.29845166431681E-6,0.0546083462055371,
0.109479711095743,0.199263575998483,0.278476799071752,0.357016538590781,
0.361096115615465),.UNSPECIFIED.);
#1464=B_SPLINE_CURVE_WITH_KNOTS('',3,(#25424,#25425,#25426,#25427,#25428,
#25429,#25430,#25431,#25432,#25433,#25434,#25435,#25436,#25437,#25438,#25439,
#25440,#25441,#25442,#25443,#25444,#25445,#25446,#25447,#25448,#25449,#25450,
#25451,#25452,#25453,#25454,#25455,#25456,#25457,#25458,#25459,#25460,#25461,
#25462,#25463,#25464,#25465,#25466,#25467,#25468,#25469,#25470,#25471,#25472,
#25473,#25474,#25475,#25476,#25477,#25478,#25479,#25480,#25481,#25482,#25483,
#25484,#25485,#25486,#25487,#25488,#25489,#25490,#25491,#25492,#25493,#25494,
#25495,#25496,#25497,#25498,#25499,#25500,#25501,#25502,#25503,#25504,#25505,
#25506,#25507,#25508,#25509,#25510,#25511,#25512,#25513,#25514,#25515,#25516,
#25517,#25518,#25519,#25520,#25521,#25522,#25523),.UNSPECIFIED.,.F.,.F.,
(4,3,3,3,3,3,3,3,3,3,3,3,3,3,3,3,3,3,3,3,3,3,3,3,3,3,3,3,3,3,3,3,3,4),(-2.19769548978374,
-2.16996208153018,-2.13535871400152,-2.10082245618501,-2.09476556787962,
-2.08923073045232,-2.0551999841314,-2.02127001257704,-1.99454552012076,
-1.98991819571071,-1.95669919080343,-1.92379392379268,-1.89175881298667,
-1.87244139578649,-1.86490525090243,-1.85913416106667,-1.85495455874982,
-1.82334168177451,-1.81899725957887,-1.78691133993479,-1.75455244345232,
-1.73856969434239,-1.73229684856998,-1.72680262056442,-1.69537207398216,
-1.66392310425677,-1.63300450698346,-1.61621134169549,-1.60686948326227,
-1.60236537222576,-1.57213504949349,-1.54232837915983,-1.51334659517059,
-1.49894425059128),.UNSPECIFIED.);
#1465=B_SPLINE_CURVE_WITH_KNOTS('',3,(#25525,#25526,#25527,#25528,#25529,
#25530,#25531,#25532,#25533,#25534,#25535,#25536,#25537,#25538,#25539,#25540,
#25541,#25542,#25543,#25544,#25545,#25546,#25547,#25548,#25549,#25550,#25551,
#25552,#25553,#25554,#25555,#25556,#25557,#25558,#25559,#25560,#25561,#25562,
#25563,#25564,#25565,#25566,#25567,#25568,#25569,#25570,#25571,#25572,#25573,
#25574,#25575,#25576,#25577,#25578,#25579,#25580,#25581,#25582,#25583,#25584,
#25585,#25586,#25587,#25588,#25589,#25590,#25591,#25592,#25593,#25594,#25595,
#25596,#25597,#25598,#25599,#25600,#25601,#25602,#25603,#25604,#25605,#25606,
#25607,#25608,#25609,#25610,#25611,#25612,#25613,#25614,#25615,#25616,#25617,
#25618,#25619,#25620,#25621),.UNSPECIFIED.,.F.,.F.,(4,3,3,3,3,3,3,3,3,3,
3,3,3,3,3,3,3,3,3,3,3,3,3,3,3,3,3,3,3,3,3,3,4),(-2.19794260024569,-2.16379459538134,
-2.12909478229254,-2.09474478574741,-2.0892597211607,-2.05520722562912,
-2.02140659959258,-1.99927981030521,-1.99390270623858,-1.98887593211283,
-1.95581388327196,-1.92314427933987,-1.89138524127318,-1.86791965517696,
-1.8605499603638,-1.85650011315063,-1.84464664343001,-1.81269774603171,
-1.78035895899146,-1.74810662597683,-1.73375644174792,-1.72933691089787,
-1.69753405795295,-1.66620981151358,-1.63416765531588,-1.61814657721703,
-1.61003028450692,-1.60438481581443,-1.60212549911818,-1.57201964467436,
-1.5426911199921,-1.52221163485995,-1.49894425059015),.UNSPECIFIED.);
#1466=B_SPLINE_CURVE_WITH_KNOTS('',3,(#25622,#25623,#25624,#25625),
 .UNSPECIFIED.,.F.,.F.,(4,4),(-0.0136507999019738,0.),.UNSPECIFIED.);
#1467=B_SPLINE_CURVE_WITH_KNOTS('',3,(#25851,#25852,#25853,#25854,#25855,
#25856,#25857,#25858,#25859,#25860,#25861,#25862,#25863,#25864,#25865,#25866,
#25867,#25868,#25869,#25870,#25871,#25872,#25873,#25874,#25875,#25876,#25877,
#25878,#25879,#25880,#25881,#25882,#25883,#25884,#25885,#25886,#25887,#25888,
#25889,#25890,#25891,#25892,#25893,#25894,#25895,#25896,#25897,#25898,#25899,
#25900,#25901,#25902,#25903,#25904,#25905,#25906,#25907,#25908,#25909,#25910,
#25911,#25912,#25913,#25914,#25915,#25916,#25917,#25918,#25919,#25920,#25921,
#25922,#25923,#25924,#25925,#25926,#25927,#25928,#25929,#25930,#25931,#25932,
#25933,#25934,#25935,#25936,#25937,#25938,#25939,#25940,#25941,#25942,#25943,
#25944),.UNSPECIFIED.,.F.,.F.,(4,3,3,3,3,3,3,3,3,3,3,3,3,3,3,3,3,3,3,3,
3,3,3,3,3,3,3,3,3,3,3,4),(-232.946686419845,-232.920698623695,-232.888128466004,
-232.854634003,-232.836299126277,-232.828986333775,-232.82374876418,-232.789594601998,
-232.753900834196,-232.718207066393,-232.707936860927,-232.703263378653,
-232.667316137156,-232.631177781828,-232.595515553508,-232.577842315535,
-232.562697236381,-232.560080409211,-232.524280232497,-232.488406293369,
-232.451648585627,-232.416879702357,-232.409368374264,-232.371464878899,
-232.333481887168,-232.295618139985,-232.276686266394,-232.264081625322,
-232.257754392803,-232.218756617189,-232.179856440503,-232.164324022216),
 .UNSPECIFIED.);
#1468=B_SPLINE_CURVE_WITH_KNOTS('',3,(#25945,#25946,#25947,#25948),
 .UNSPECIFIED.,.F.,.F.,(4,4),(0.,0.0138563661205195),.UNSPECIFIED.);
#1469=B_SPLINE_CURVE_WITH_KNOTS('',3,(#25949,#25950,#25951,#25952,#25953,
#25954,#25955,#25956,#25957,#25958,#25959,#25960,#25961,#25962,#25963,#25964,
#25965,#25966,#25967,#25968,#25969,#25970,#25971,#25972,#25973,#25974,#25975,
#25976,#25977,#25978,#25979,#25980,#25981,#25982,#25983,#25984,#25985,#25986,
#25987,#25988,#25989,#25990,#25991,#25992,#25993,#25994,#25995,#25996,#25997,
#25998,#25999,#26000,#26001,#26002,#26003,#26004,#26005,#26006,#26007,#26008,
#26009,#26010,#26011,#26012,#26013,#26014,#26015,#26016,#26017,#26018,#26019,
#26020,#26021,#26022,#26023,#26024,#26025,#26026,#26027,#26028,#26029,#26030,
#26031,#26032,#26033,#26034,#26035,#26036,#26037,#26038,#26039),
 .UNSPECIFIED.,.F.,.F.,(4,3,3,3,3,3,3,3,3,3,3,3,3,3,3,3,3,3,3,3,3,3,3,3,
3,3,3,3,3,3,4),(-482.256901778709,-482.224225803402,-482.190525587978,-482.156852378964,
-482.150327631204,-482.144056954824,-482.109513167315,-482.074286620043,
-482.051899343887,-482.039111838982,-482.033818937828,-481.99768233578,
-481.961478406429,-481.925962153481,-481.896304483897,-481.891074900579,
-481.855343675935,-481.819332394006,-481.782400925057,-481.748150002002,
-481.740976721928,-481.703311159677,-481.665167855225,-481.62701437128,
-481.595344288617,-481.589293307268,-481.584346741121,-481.545122580121,
-481.50612183907,-481.500182765298,-481.468537766939),.UNSPECIFIED.);
#1470=B_SPLINE_CURVE_WITH_KNOTS('',3,(#26048,#26049,#26050,#26051),
 .UNSPECIFIED.,.F.,.F.,(4,4),(68.198771421486,69.1672389387709),
 .UNSPECIFIED.);
#1471=B_SPLINE_CURVE_WITH_KNOTS('',3,(#26054,#26055,#26056,#26057,#26058,
#26059,#26060,#26061,#26062,#26063,#26064,#26065,#26066,#26067,#26068,#26069,
#26070,#26071,#26072,#26073,#26074,#26075,#26076,#26077,#26078,#26079,#26080,
#26081,#26082,#26083,#26084,#26085,#26086,#26087,#26088,#26089,#26090,#26091,
#26092,#26093,#26094,#26095,#26096,#26097,#26098,#26099,#26100,#26101,#26102,
#26103,#26104,#26105,#26106,#26107,#26108),.UNSPECIFIED.,.F.,.F.,(4,3,3,
3,3,3,3,3,3,3,3,3,3,3,3,3,3,3,4),(68.1990165158139,68.2867039372834,68.3743981543787,
68.4621196239386,68.5499348194578,68.6378063115861,68.7257986904822,68.744531877364,
68.8318666265745,68.9190930016561,69.0062345365395,69.0933171048388,69.1803688850522,
69.2674110254065,69.354464662252,69.4416035010195,69.5287857172442,69.6161043390497,
69.6911556575798),.UNSPECIFIED.);
#1472=B_SPLINE_CURVE_WITH_KNOTS('',3,(#26114,#26115,#26116,#26117,#26118,
#26119,#26120,#26121,#26122,#26123,#26124,#26125,#26126,#26127,#26128,#26129,
#26130,#26131,#26132,#26133,#26134,#26135,#26136,#26137,#26138,#26139,#26140,
#26141,#26142,#26143,#26144,#26145,#26146,#26147,#26148,#26149,#26150,#26151,
#26152,#26153,#26154,#26155,#26156,#26157,#26158,#26159,#26160,#26161,#26162,
#26163,#26164,#26165,#26166,#26167,#26168,#26169,#26170,#26171,#26172,#26173,
#26174,#26175,#26176,#26177,#26178,#26179,#26180,#26181,#26182,#26183,#26184,
#26185,#26186,#26187,#26188,#26189,#26190,#26191,#26192,#26193,#26194,#26195,
#26196,#26197,#26198,#26199,#26200,#26201,#26202,#26203,#26204,#26205,#26206,
#26207,#26208,#26209,#26210,#26211,#26212,#26213,#26214,#26215,#26216,#26217,
#26218,#26219,#26220,#26221,#26222,#26223,#26224,#26225,#26226,#26227,#26228,
#26229,#26230,#26231,#26232,#26233,#26234,#26235,#26236,#26237,#26238,#26239,
#26240,#26241,#26242,#26243,#26244,#26245,#26246,#26247,#26248,#26249,#26250,
#26251,#26252,#26253,#26254,#26255,#26256,#26257,#26258,#26259,#26260,#26261),
 .UNSPECIFIED.,.F.,.F.,(4,3,3,3,3,3,3,3,3,3,3,3,3,3,3,3,3,3,3,3,3,3,3,3,
3,3,3,3,3,3,3,3,3,3,3,3,3,3,3,3,3,3,3,3,3,3,3,3,3,4),(61.9152074670456,
62.0028392502741,62.0905179625085,62.1783353503388,62.2505508730523,62.3384131475251,
62.4261650959704,62.5138296608294,62.6044320992451,62.6919987313428,62.779552535813,
62.8671141164615,62.9547040775598,63.0423902308967,63.1301338862199,63.2180014802831,
63.2386491681549,63.3265146658182,63.4142701282254,63.5019384895468,63.5925396112606,
63.6801107100817,63.7676692197789,63.8552357377434,63.9428308619984,64.0305224830768,
64.1182717900469,64.2061452583331,64.2267474632576,64.3144870789918,64.4021162042687,
64.4896579267435,64.5803064056956,64.6677509157514,64.7551830721912,64.8426236080885,
64.9300932575184,65.0176607782296,65.1052866424268,65.1930385556437,65.2148457583603,
65.3017898443855,65.3885981523834,65.4753288625677,65.5620035755417,65.6486438406302,
65.7352974265419,65.8219556596735,65.9086836728027,65.9734457253856),
 .UNSPECIFIED.);
#1473=B_SPLINE_CURVE_WITH_KNOTS('',3,(#26262,#26263,#26264,#26265,#26266,
#26267,#26268),.UNSPECIFIED.,.F.,.F.,(4,1,1,1,4),(65.9734462067016,66.2029440534629,
67.1910423485656,68.1791406436682,68.198771421486),.UNSPECIFIED.);
#1474=B_SPLINE_CURVE_WITH_KNOTS('',3,(#26270,#26271,#26272,#26273,#26274,
#26275,#26276,#26277,#26278,#26279,#26280,#26281,#26282,#26283,#26284,#26285,
#26286,#26287,#26288,#26289,#26290,#26291,#26292,#26293,#26294,#26295,#26296,
#26297,#26298,#26299,#26300,#26301,#26302,#26303,#26304,#26305,#26306,#26307,
#26308,#26309,#26310,#26311,#26312,#26313,#26314,#26315,#26316,#26317,#26318,
#26319,#26320,#26321,#26322,#26323,#26324,#26325,#26326,#26327,#26328,#26329,
#26330,#26331,#26332,#26333,#26334,#26335,#26336,#26337,#26338,#26339,#26340,
#26341,#26342,#26343,#26344,#26345,#26346,#26347,#26348,#26349,#26350,#26351),
 .UNSPECIFIED.,.F.,.F.,(4,3,3,3,3,3,3,3,3,3,3,3,3,3,3,3,3,3,3,3,3,3,3,3,
3,3,3,4),(65.9734457255614,66.0599244006815,66.1484757614912,66.2348343901556,
66.3211731338775,66.4075137224388,66.4977191136188,66.5841760425287,66.6706891415639,
66.7573212530809,66.7683352871587,66.8560751038854,66.9437044304637,67.0312463543199,
67.1218947578126,67.2093394682341,67.2967718243368,67.3842125589907,67.4716824060662,
67.5592501218174,67.6468761797695,67.7346282834129,67.7564335822614,67.8444394353351,
67.9330837054548,68.0208783079558,68.1099474118848,68.1990165158139),
 .UNSPECIFIED.);
#1475=B_SPLINE_CURVE_WITH_KNOTS('',3,(#26352,#26353,#26354,#26355,#26356,
#26357,#26358,#26359,#26360,#26361,#26362,#26363,#26364,#26365,#26366,#26367,
#26368,#26369,#26370,#26371,#26372,#26373,#26374,#26375,#26376,#26377,#26378,
#26379,#26380,#26381,#26382,#26383,#26384,#26385,#26386,#26387,#26388,#26389,
#26390,#26391,#26392,#26393,#26394,#26395,#26396,#26397,#26398,#26399,#26400,
#26401,#26402,#26403,#26404,#26405,#26406,#26407,#26408,#26409,#26410,#26411,
#26412,#26413,#26414,#26415,#26416,#26417,#26418,#26419,#26420,#26421,#26422,
#26423,#26424,#26425,#26426,#26427,#26428,#26429,#26430,#26431,#26432,#26433,
#26434,#26435,#26436,#26437,#26438,#26439,#26440,#26441,#26442,#26443,#26444,
#26445,#26446,#26447,#26448,#26449,#26450,#26451,#26452,#26453,#26454,#26455,
#26456,#26457,#26458,#26459,#26460,#26461,#26462,#26463,#26464,#26465,#26466,
#26467,#26468,#26469,#26470,#26471,#26472,#26473,#26474,#26475,#26476,#26477,
#26478,#26479,#26480,#26481,#26482,#26483,#26484,#26485,#26486,#26487,#26488,
#26489,#26490,#26491,#26492,#26493,#26494,#26495,#26496,#26497,#26498,#26499),
 .UNSPECIFIED.,.F.,.F.,(4,3,3,3,3,3,3,3,3,3,3,3,3,3,3,3,3,3,3,3,3,3,3,3,
3,3,3,3,3,3,3,3,3,3,3,3,3,3,3,3,3,3,3,3,3,3,3,3,3,4),(61.9160292898655,
62.003765986239,62.0914154584642,62.1819812894997,62.2695333123404,62.3570727013311,
62.4446200755284,62.532196054615,62.6198685560932,62.7075987803768,62.7954531982411,
62.815942106748,62.9037916043167,62.9915308699443,63.0791828597822,63.1697900525408,
63.2573444543976,63.3448861767483,63.4324358359914,63.520014049116,63.6076887678098,
63.6954211583331,63.7832778180181,63.8040404018507,63.8918717835893,63.979592882304,
64.0672266762862,64.1578406788696,64.2453769286839,64.3329005466778,64.4204321688873,
64.5079924320004,64.5956494187184,64.6833641842158,64.7712035068591,64.7921386969534,
64.8800009524886,64.9677528821818,65.0554174284929,65.1460198739383,65.2335864881031,
65.3211402748971,65.4087018381435,65.4962917821319,65.5839779188708,65.6717215578754,
65.7595891361461,65.780236992056,65.9057469402362,65.9734457253856),
 .UNSPECIFIED.);
#1476=B_SPLINE_CURVE_WITH_KNOTS('',3,(#26505,#26506,#26507,#26508,#26509,
#26510,#26511,#26512,#26513,#26514,#26515,#26516,#26517,#26518,#26519,#26520,
#26521,#26522,#26523,#26524,#26525,#26526,#26527,#26528,#26529,#26530,#26531,
#26532,#26533,#26534,#26535,#26536,#26537,#26538,#26539,#26540,#26541,#26542,
#26543,#26544,#26545,#26546,#26547,#26548,#26549,#26550,#26551,#26552,#26553,
#26554,#26555,#26556,#26557,#26558,#26559,#26560,#26561,#26562,#26563,#26564,
#26565,#26566,#26567,#26568,#26569,#26570,#26571,#26572,#26573,#26574,#26575,
#26576,#26577,#26578,#26579,#26580,#26581,#26582,#26583,#26584,#26585,#26586,
#26587,#26588,#26589,#26590,#26591,#26592,#26593,#26594,#26595,#26596,#26597,
#26598,#26599,#26600,#26601,#26602,#26603,#26604,#26605,#26606,#26607,#26608,
#26609,#26610,#26611,#26612,#26613,#26614,#26615,#26616,#26617,#26618,#26619,
#26620,#26621,#26622,#26623,#26624,#26625,#26626,#26627,#26628,#26629,#26630,
#26631,#26632,#26633,#26634,#26635,#26636,#26637,#26638,#26639,#26640,#26641,
#26642,#26643,#26644,#26645,#26646,#26647,#26648,#26649,#26650,#26651,#26652),
 .UNSPECIFIED.,.F.,.F.,(4,3,3,3,3,3,3,3,3,3,3,3,3,3,3,3,3,3,3,3,3,3,3,3,
3,3,3,3,3,3,3,3,3,3,3,3,3,3,3,3,3,3,3,3,3,3,3,3,3,4),(55.6329415823545,
55.7205103087394,55.8080534505669,55.8955916358262,55.9831454839555,56.0707895120438,
56.1584796275128,56.2463091812715,56.3219611024363,56.4098069678268,56.4975425704886,
56.5851908713359,56.6757994371112,56.7633501093486,56.8508880936569,56.9384340105917,
57.0260084812995,57.1136794763125,57.2014081498481,57.2892611303658,57.3100593975389,
57.3979057700926,57.4856418852267,57.5732907031754,57.6638990768587,57.7514502743065,
57.8389887858891,57.9265352315721,58.014110231911,58.1017817551768,58.1895109567624,
58.2773644610362,58.2981576926416,58.3860015379222,58.4737351205031,58.5613814036833,
58.6519907266909,58.7395393999614,58.8270753956588,58.9146193364734,59.0021918456963,
59.0898609105614,59.1775876700309,59.265438774201,59.2862559877443,59.3872570953136,
59.4837999140162,59.5800852540891,59.6759906400734,59.6902604180213),
 .UNSPECIFIED.);
#1477=B_SPLINE_CURVE_WITH_KNOTS('',3,(#26653,#26654,#26655,#26656,#26657,
#26658,#26659,#26660,#26661,#26662,#26663,#26664,#26665,#26666,#26667,#26668,
#26669,#26670,#26671,#26672,#26673,#26674,#26675,#26676,#26677,#26678,#26679,
#26680,#26681,#26682,#26683,#26684,#26685,#26686,#26687,#26688,#26689,#26690,
#26691,#26692,#26693,#26694,#26695,#26696,#26697,#26698,#26699,#26700,#26701,
#26702,#26703,#26704,#26705,#26706,#26707,#26708,#26709,#26710,#26711,#26712,
#26713,#26714,#26715,#26716,#26717,#26718,#26719,#26720,#26721,#26722,#26723,
#26724,#26725,#26726,#26727,#26728,#26729,#26730,#26731,#26732,#26733,#26734),
 .UNSPECIFIED.,.F.,.F.,(4,3,3,3,3,3,3,3,3,3,3,3,3,3,3,3,3,3,3,3,3,3,3,3,
3,3,3,4),(59.6902604182061,59.7791601363368,59.8680903388289,59.9570692322848,
60.0461757616844,60.1353527655857,60.2246849720358,60.2743542828469,60.362203797533,
60.4499430803699,60.5375950874869,60.6282022737948,60.715756692995,60.8032984326827,
60.8908481092374,60.978426339629,61.0661010754383,61.153833483008,61.2416901595109,
61.2624525779496,61.350268063159,61.4379804811472,61.525610640487,61.6131792828027,
61.7007144613418,61.7882299492699,61.875765618165,61.9152074670456),
 .UNSPECIFIED.);
#1478=B_SPLINE_CURVE_WITH_KNOTS('',3,(#26736,#26737,#26738,#26739,#26740,
#26741,#26742,#26743,#26744,#26745,#26746,#26747,#26748,#26749,#26750,#26751,
#26752,#26753,#26754,#26755,#26756,#26757,#26758,#26759,#26760,#26761,#26762,
#26763,#26764,#26765,#26766,#26767,#26768,#26769,#26770,#26771,#26772,#26773,
#26774,#26775,#26776,#26777,#26778,#26779,#26780,#26781,#26782,#26783,#26784,
#26785,#26786,#26787,#26788,#26789,#26790,#26791,#26792,#26793,#26794,#26795,
#26796,#26797,#26798,#26799,#26800,#26801,#26802,#26803,#26804,#26805,#26806,
#26807,#26808,#26809,#26810,#26811,#26812,#26813,#26814,#26815,#26816,#26817),
 .UNSPECIFIED.,.F.,.F.,(4,3,3,3,3,3,3,3,3,3,3,3,3,3,3,3,3,3,3,3,3,3,3,3,
3,3,3,4),(59.6902604182061,59.8288576938286,59.85164722144,59.9394935907456,
60.0272297026167,60.114878517291,60.2054868921975,60.2930380863645,60.3805765946698,
60.4681230370823,60.5556980341614,60.6433695541988,60.7310987525705,60.8189522536764,
60.8397455165427,60.9275893686412,61.0153229580445,61.1029692480439,61.1935785684941,
61.2811272485317,61.3686632509655,61.4562071984788,61.5437797143553,61.6314487857747,
61.7191755517482,61.8070266623,61.8278438116454,61.9160292898655),
 .UNSPECIFIED.);
#1479=B_SPLINE_CURVE_WITH_KNOTS('',3,(#26818,#26819,#26820,#26821,#26822,
#26823,#26824,#26825,#26826,#26827,#26828,#26829,#26830,#26831,#26832,#26833,
#26834,#26835,#26836,#26837,#26838,#26839,#26840,#26841,#26842,#26843,#26844,
#26845,#26846,#26847,#26848,#26849,#26850,#26851,#26852,#26853,#26854,#26855,
#26856,#26857,#26858,#26859,#26860,#26861,#26862,#26863,#26864,#26865,#26866,
#26867,#26868,#26869,#26870,#26871,#26872,#26873,#26874,#26875,#26876,#26877,
#26878,#26879,#26880,#26881,#26882,#26883,#26884,#26885,#26886,#26887,#26888,
#26889,#26890,#26891,#26892,#26893,#26894,#26895,#26896,#26897,#26898,#26899,
#26900,#26901,#26902,#26903,#26904,#26905,#26906,#26907,#26908,#26909,#26910,
#26911,#26912,#26913,#26914,#26915,#26916,#26917,#26918,#26919,#26920,#26921,
#26922,#26923,#26924,#26925,#26926,#26927,#26928,#26929,#26930,#26931,#26932,
#26933,#26934,#26935,#26936,#26937,#26938,#26939,#26940,#26941,#26942,#26943,
#26944,#26945,#26946,#26947,#26948,#26949,#26950,#26951,#26952,#26953,#26954,
#26955,#26956,#26957,#26958,#26959,#26960,#26961,#26962,#26963,#26964,#26965),
 .UNSPECIFIED.,.F.,.F.,(4,3,3,3,3,3,3,3,3,3,3,3,3,3,3,3,3,3,3,3,3,3,3,3,
3,3,3,3,3,3,3,3,3,3,3,3,3,3,3,3,3,3,3,3,3,3,3,3,3,4),(55.6319201599848,
55.7196005837777,55.8094273124036,55.8992540410294,55.9870997806171,56.0748352588762,
56.162483436848,56.2530920492585,56.3406426031537,56.4281804709919,56.5157262734477,
56.603300631787,56.6909715180913,56.7787000849292,56.8665529624602,56.8873523361321,
56.9751981693186,57.0629337418575,57.1505820146696,57.2411905917402,57.3287412412526,
57.4162792048268,57.5038251030318,57.591399557027,57.6790705383681,57.7667991999897,
57.8546521712214,57.8754506312347,57.9632961259926,58.051031359628,58.1386792934676,
58.2292879975763,58.3168383100931,58.4043759379858,58.4919215021854,58.5794956242163,
58.6671662782576,58.7548946149278,58.8427472670603,58.8635489263374,58.9501115740607,
59.0365644100789,59.1229218421432,59.2092266551714,59.2955006634414,59.3817656498755,
59.4680807244374,59.554422813523,59.6408625970588,59.6902604180514),
 .UNSPECIFIED.);
#1480=B_SPLINE_CURVE_WITH_KNOTS('',3,(#26971,#26972,#26973,#26974,#26975,
#26976,#26977,#26978,#26979,#26980,#26981,#26982,#26983,#26984,#26985,#26986,
#26987,#26988,#26989,#26990,#26991,#26992,#26993,#26994,#26995,#26996,#26997,
#26998,#26999,#27000,#27001,#27002,#27003,#27004,#27005,#27006,#27007,#27008,
#27009,#27010,#27011,#27012,#27013,#27014,#27015,#27016,#27017,#27018,#27019,
#27020,#27021,#27022,#27023,#27024,#27025,#27026,#27027,#27028,#27029,#27030,
#27031,#27032,#27033,#27034,#27035,#27036,#27037,#27038,#27039,#27040,#27041,
#27042,#27043,#27044,#27045,#27046,#27047,#27048,#27049,#27050,#27051,#27052,
#27053,#27054,#27055,#27056,#27057,#27058,#27059,#27060,#27061,#27062,#27063,
#27064,#27065,#27066,#27067,#27068,#27069,#27070,#27071,#27072,#27073,#27074,
#27075,#27076,#27077,#27078,#27079,#27080,#27081,#27082,#27083,#27084,#27085,
#27086,#27087,#27088,#27089,#27090,#27091,#27092,#27093,#27094,#27095,#27096,
#27097,#27098,#27099,#27100,#27101,#27102,#27103,#27104,#27105,#27106,#27107,
#27108,#27109,#27110,#27111,#27112,#27113,#27114,#27115,#27116,#27117,#27118,
#27119,#27120,#27121),.UNSPECIFIED.,.F.,.F.,(4,3,3,3,3,3,3,3,3,3,3,3,3,
3,3,3,3,3,3,3,3,3,3,3,3,3,3,3,3,3,3,3,3,3,3,3,3,3,3,3,3,3,3,3,3,3,3,3,3,
3,4),(49.3489872945652,49.4052730367176,49.4931187667722,49.5808542357431,
49.6685024046791,49.7591110205717,49.8466615661085,49.9341994258518,50.0217452204837,
50.109319571278,50.1969904504838,50.2847190104756,50.3725718815769,50.3933713318203,
50.4812170646052,50.5689525362668,50.6566007078512,50.7472093227352,50.8347598707998,
50.9222977330224,51.0098435300823,51.0974178832511,51.1850887647406,51.2728173269658,
51.3606702002109,51.381469626923,51.4693153753648,51.5570508627688,51.6446990501612,
51.7353076591443,51.8228582230782,51.9103961011649,51.9979419140664,52.0855162830366,
52.1731871801893,52.2609157580148,52.3487686466512,52.3695679220256,52.4574136261298,
52.5451490691642,52.6327972122078,52.7234058378229,52.8109563577401,52.8984941920087,
52.9860399613381,53.0736142870294,53.1612851415514,53.2490136770757,53.3368665242072,
53.3576662171283,53.4070751110265),.UNSPECIFIED.);
#1481=B_SPLINE_CURVE_WITH_KNOTS('',3,(#27122,#27123,#27124,#27125,#27126,
#27127,#27128,#27129,#27130,#27131,#27132,#27133,#27134,#27135,#27136,#27137,
#27138,#27139,#27140,#27141,#27142,#27143,#27144,#27145,#27146,#27147,#27148,
#27149,#27150,#27151,#27152,#27153,#27154,#27155,#27156,#27157,#27158,#27159,
#27160,#27161,#27162,#27163,#27164,#27165,#27166,#27167,#27168,#27169,#27170,
#27171,#27172,#27173,#27174,#27175,#27176,#27177,#27178,#27179,#27180,#27181,
#27182,#27183,#27184,#27185,#27186,#27187,#27188,#27189,#27190,#27191,#27192,
#27193,#27194,#27195,#27196,#27197,#27198,#27199,#27200,#27201,#27202,#27203),
 .UNSPECIFIED.,.F.,.F.,(4,3,3,3,3,3,3,3,3,3,3,3,3,3,3,3,3,3,3,3,3,3,3,3,
3,3,3,4),(53.4070751111794,53.4942487792892,53.581315479733,53.6682989026037,
53.7552259023249,53.8421238514233,53.9290140393189,54.0159177450201,54.102908698297,
54.1899450618072,54.2771175328094,54.345764512231,54.4336103459984,54.5213459191207,
54.6089941925175,54.6996027693695,54.7871534194668,54.8746913836249,54.9622372824117,
55.0498117369875,55.1374827189024,55.2252113810947,55.3130643528886,55.3338628073336,
55.4216973721277,55.5094350678335,55.5970786676283,55.6329415823545),
 .UNSPECIFIED.);
#1482=B_SPLINE_CURVE_WITH_KNOTS('',3,(#27205,#27206,#27207,#27208,#27209,
#27210,#27211,#27212,#27213,#27214,#27215,#27216,#27217,#27218,#27219,#27220,
#27221,#27222,#27223,#27224,#27225,#27226,#27227,#27228,#27229,#27230,#27231,
#27232,#27233,#27234,#27235,#27236,#27237,#27238,#27239,#27240,#27241,#27242,
#27243,#27244,#27245,#27246,#27247,#27248,#27249,#27250,#27251,#27252,#27253,
#27254,#27255,#27256,#27257,#27258,#27259,#27260,#27261,#27262,#27263,#27264,
#27265,#27266,#27267,#27268,#27269,#27270,#27271,#27272,#27273,#27274,#27275,
#27276,#27277,#27278,#27279,#27280,#27281,#27282,#27283,#27284,#27285,#27286),
 .UNSPECIFIED.,.F.,.F.,(4,3,3,3,3,3,3,3,3,3,3,3,3,3,3,3,3,3,3,3,3,3,3,3,
3,3,3,4),(53.4070751110265,53.4979084720332,53.5888357596706,53.6799484289355,
53.7711596831757,53.8625643336905,53.9230574508241,54.0109031991677,54.0986386864732,
54.186286873767,54.276895482787,54.3644460466224,54.4519839246107,54.5395297374141,
54.6271041062866,54.7147750033428,54.8025035810724,54.8903564696145,54.9111557459267,
55.001251297684,55.0889717707487,55.176611913228,55.2641924455928,55.3561243741908,
55.4436628150252,55.5312019731037,55.61878222435,55.6319201599848),
 .UNSPECIFIED.);
#1483=B_SPLINE_CURVE_WITH_KNOTS('',3,(#27287,#27288,#27289,#27290,#27291,
#27292,#27293,#27294,#27295,#27296,#27297,#27298,#27299,#27300,#27301,#27302,
#27303,#27304,#27305,#27306,#27307,#27308,#27309,#27310,#27311,#27312,#27313,
#27314,#27315,#27316,#27317,#27318,#27319,#27320,#27321,#27322,#27323,#27324,
#27325,#27326,#27327,#27328,#27329,#27330,#27331,#27332,#27333,#27334,#27335,
#27336,#27337,#27338,#27339,#27340,#27341,#27342,#27343,#27344,#27345,#27346,
#27347,#27348,#27349,#27350,#27351,#27352,#27353,#27354,#27355,#27356,#27357,
#27358,#27359,#27360,#27361,#27362,#27363,#27364,#27365,#27366,#27367,#27368,
#27369,#27370,#27371,#27372,#27373,#27374,#27375,#27376,#27377,#27378,#27379,
#27380,#27381,#27382,#27383,#27384,#27385,#27386,#27387,#27388,#27389,#27390,
#27391,#27392,#27393,#27394,#27395,#27396,#27397,#27398,#27399,#27400,#27401,
#27402,#27403,#27404,#27405,#27406,#27407,#27408,#27409,#27410,#27411,#27412,
#27413,#27414,#27415,#27416,#27417,#27418,#27419,#27420,#27421,#27422,#27423,
#27424,#27425,#27426,#27427,#27428,#27429,#27430,#27431),.UNSPECIFIED.,
 .F.,.F.,(4,3,3,3,3,3,3,3,3,3,3,3,3,3,3,3,3,3,3,3,3,3,3,3,3,3,3,3,3,3,3,
3,3,3,3,3,3,3,3,3,3,3,3,3,3,3,3,3,4),(49.3496195384547,49.4371668507027,
49.5247045899421,49.612253376003,49.7018560996056,49.7895356797267,49.8800999750701,
49.9706642704134,50.0585100036378,50.1462454757683,50.2338936478499,50.3245022625582,
50.4120528111866,50.4995906739965,50.5871364716665,50.6747108254672,50.7623817076176,
50.8501102705212,50.9379631444655,50.9587625655161,51.0466083011504,51.134343775701,
51.2219919502098,51.3126005640109,51.4001511150689,51.487688980305,51.5752347803949,
51.6628091366067,51.7504800211437,51.8382085864225,51.9260614627063,51.9468608606187,
52.0347065906943,52.1224420596861,52.2100902286431,52.3006988445279,52.3882493900852,
52.4757872498489,52.5633330445013,52.650907395315,52.7385782745406,52.8263068345526,
52.9141597056729,52.9349591557214,53.0281706542195,53.1228967683669,53.2156926069346,
53.311383858872,53.4070751108094),.UNSPECIFIED.);
#1484=B_SPLINE_CURVE_WITH_KNOTS('',3,(#27437,#27438,#27439,#27440,#27441,
#27442,#27443,#27444),.UNSPECIFIED.,.F.,.F.,(4,1,1,1,1,4),(43.0656672236125,
43.4766832661016,44.4647815612043,45.452879856307,46.4409781514096,47.1238898038469),
 .UNSPECIFIED.);
#1485=B_SPLINE_CURVE_WITH_KNOTS('',3,(#27445,#27446,#27447,#27448,#27449,
#27450,#27451,#27452,#27453,#27454,#27455,#27456,#27457,#27458,#27459,#27460,
#27461,#27462,#27463,#27464,#27465,#27466,#27467,#27468,#27469,#27470,#27471,
#27472,#27473,#27474,#27475,#27476,#27477,#27478,#27479,#27480,#27481,#27482,
#27483,#27484,#27485,#27486,#27487,#27488,#27489,#27490,#27491,#27492,#27493,
#27494,#27495,#27496,#27497,#27498,#27499,#27500,#27501,#27502,#27503,#27504,
#27505,#27506,#27507,#27508,#27509,#27510,#27511,#27512,#27513,#27514,#27515,
#27516,#27517,#27518,#27519,#27520,#27521,#27522,#27523),.UNSPECIFIED.,
 .F.,.F.,(4,3,3,3,3,3,3,3,3,3,3,3,3,3,3,3,3,3,3,3,3,3,3,3,3,3,4),(47.1238899834251,
47.2279237124283,47.3331422464939,47.4290764465123,47.5169221797334,47.6046576518605,
47.6923058239389,47.7829144386485,47.8704649872736,47.9580028500801,48.0455486477467,
48.1331230015439,48.2207938836911,48.3085224465917,48.3963753205325,48.417174741615,
48.5050237765636,48.5927617437342,48.6804116075757,48.7679951400718,48.8555434981,
48.9430773171428,49.0306172170903,49.1182278887984,49.2058765988617,49.2936398438844,
49.3489872945652),.UNSPECIFIED.);
#1486=B_SPLINE_CURVE_WITH_KNOTS('',3,(#27525,#27526,#27527,#27528,#27529,
#27530,#27531,#27532,#27533,#27534,#27535,#27536,#27537,#27538,#27539,#27540,
#27541,#27542,#27543,#27544,#27545,#27546,#27547,#27548,#27549,#27550,#27551,
#27552,#27553,#27554,#27555,#27556,#27557,#27558,#27559,#27560,#27561,#27562,
#27563,#27564,#27565,#27566,#27567,#27568,#27569,#27570,#27571,#27572,#27573,
#27574,#27575,#27576,#27577,#27578,#27579,#27580,#27581,#27582,#27583,#27584,
#27585,#27586,#27587,#27588,#27589,#27590,#27591,#27592,#27593,#27594,#27595,
#27596,#27597,#27598,#27599,#27600,#27601,#27602,#27603,#27604,#27605,#27606),
 .UNSPECIFIED.,.F.,.F.,(4,3,3,3,3,3,3,3,3,3,3,3,3,3,3,3,3,3,3,3,3,3,3,3,
3,3,3,4),(47.1238898040527,47.210492156019,47.2969993784341,47.3841829161559,
47.4705790288969,47.5569581549671,47.6433419919605,47.7311234140224,47.8176268261185,
47.9060472531633,47.9944676802081,48.0823134140176,48.1700488867384,48.2576970594146,
48.3483056739016,48.4358562231318,48.5233940865448,48.6109398848189,48.6985142392238,
48.7861851219757,48.8739136854801,48.9617665600191,48.9825659753107,49.0743293660967,
49.162052739274,49.2496992777742,49.3372797397587,49.3496195384547),
 .UNSPECIFIED.);
#1487=B_SPLINE_CURVE_WITH_KNOTS('',3,(#27607,#27608,#27609,#27610,#27611,
#27612,#27613,#27614,#27615,#27616,#27617,#27618,#27619,#27620,#27621,#27622,
#27623,#27624,#27625,#27626,#27627,#27628,#27629,#27630,#27631,#27632,#27633,
#27634,#27635,#27636,#27637,#27638,#27639,#27640,#27641,#27642,#27643,#27644,
#27645,#27646,#27647,#27648,#27649,#27650,#27651,#27652,#27653,#27654,#27655,
#27656,#27657,#27658,#27659,#27660,#27661,#27662,#27663,#27664,#27665,#27666,
#27667,#27668,#27669,#27670,#27671,#27672,#27673,#27674,#27675,#27676,#27677,
#27678,#27679,#27680,#27681,#27682,#27683,#27684,#27685,#27686,#27687,#27688,
#27689,#27690,#27691,#27692,#27693,#27694,#27695,#27696,#27697,#27698,#27699,
#27700,#27701,#27702,#27703,#27704,#27705,#27706,#27707,#27708,#27709,#27710,
#27711,#27712,#27713,#27714,#27715,#27716,#27717,#27718,#27719,#27720,#27721,
#27722,#27723,#27724,#27725,#27726,#27727,#27728,#27729,#27730,#27731,#27732,
#27733,#27734,#27735,#27736,#27737,#27738,#27739,#27740,#27741,#27742,#27743,
#27744,#27745,#27746,#27747,#27748,#27749,#27750,#27751),.UNSPECIFIED.,
 .F.,.F.,(4,3,3,3,3,3,3,3,3,3,3,3,3,3,3,3,3,3,3,3,3,3,3,3,3,3,3,3,3,3,3,
3,3,3,3,3,3,3,3,3,3,3,3,3,3,3,3,3,4),(43.0661513688595,43.1539804562812,
43.2417024687189,43.3293403545273,43.4184321226861,43.505980034342,43.5935177611447,
43.6810659230641,43.7713180672474,43.8589965048089,43.9505355023032,44.0420744997974,
44.1299202333019,44.217655705717,44.3053038780874,44.395912492689,44.4834630416144,
44.5710009047237,44.6585467026954,44.7461210567996,44.8337919392548,44.9215205024643,
45.0093733767133,45.0301727949001,45.1180185284566,45.2057540009238,45.2934021733465,
45.3840107879285,45.471561336906,45.5590992000672,45.6466449980905,45.7342193522462,
45.8218902347522,45.9096187980123,45.997471672311,46.0182710900028,46.1061168234813,
46.1938522958706,46.2815004682155,46.3721090828267,46.4596596317277,46.5471974948129,
46.6347432927609,46.7223176468418,46.8099885292745,46.8977170924621,46.9855699666899,
47.0063693851054,47.1238898038469),.UNSPECIFIED.);
#1488=B_SPLINE_CURVE_WITH_KNOTS('',3,(#27757,#27758,#27759,#27760,#27761,
#27762,#27763,#27764,#27765,#27766,#27767,#27768,#27769,#27770,#27771,#27772,
#27773,#27774,#27775,#27776,#27777,#27778,#27779,#27780,#27781,#27782,#27783,
#27784,#27785,#27786,#27787,#27788,#27789,#27790,#27791,#27792,#27793,#27794,
#27795,#27796,#27797,#27798,#27799,#27800,#27801,#27802,#27803,#27804,#27805,
#27806,#27807,#27808,#27809,#27810,#27811,#27812,#27813,#27814,#27815,#27816,
#27817,#27818,#27819,#27820,#27821,#27822,#27823,#27824,#27825,#27826,#27827,
#27828,#27829,#27830,#27831,#27832,#27833,#27834,#27835,#27836,#27837,#27838,
#27839,#27840,#27841,#27842,#27843,#27844,#27845,#27846,#27847,#27848,#27849,
#27850,#27851,#27852,#27853,#27854,#27855,#27856,#27857,#27858,#27859,#27860,
#27861,#27862,#27863,#27864,#27865,#27866,#27867,#27868,#27869,#27870,#27871,
#27872,#27873,#27874,#27875,#27876,#27877,#27878,#27879,#27880,#27881,#27882,
#27883,#27884,#27885,#27886,#27887,#27888,#27889,#27890,#27891,#27892,#27893,
#27894,#27895,#27896,#27897,#27898,#27899,#27900,#27901,#27902,#27903,#27904),
 .UNSPECIFIED.,.F.,.F.,(4,3,3,3,3,3,3,3,3,3,3,3,3,3,3,3,3,3,3,3,3,3,3,3,
3,3,3,3,3,3,3,3,3,3,3,3,3,3,3,3,3,3,3,3,3,3,3,3,3,4),(36.7834594513572,
36.8710696055442,36.9586338461866,37.0461753273144,37.1337146746301,37.2212725072833,
37.308921977867,37.3966200728502,37.4844541454934,37.5480934954857,37.6359392290401,
37.7236747015056,37.811322873927,37.9019314885097,37.9894820374872,38.0770199006489,
38.1645656986731,38.2521400528301,38.3398109353381,38.4275394986005,38.5153923729021,
38.5361917905883,38.6240375240927,38.7117729965076,38.7994211688778,38.8900297834795,
38.9775803324048,39.0651181955139,39.1526639934854,39.2402383475895,39.3279092300444,
39.4156377932538,39.5034906675027,39.524290085691,39.6121358192108,39.6998712916411,
39.7875194640268,39.8781280786227,39.9656786275633,40.0532164906878,40.1407622886745,
40.2283366427937,40.3160075252636,40.4037360884876,40.491588962751,40.5123883807937,
40.6152734140351,40.7176836287931,40.819249582201,40.8407042874444),
 .UNSPECIFIED.);
#1489=B_SPLINE_CURVE_WITH_KNOTS('',3,(#27905,#27906,#27907,#27908,#27909,
#27910),.UNSPECIFIED.,.F.,.F.,(4,1,1,4),(40.8407044966673,41.5004866758963,
42.488584970999,43.0656672236125),.UNSPECIFIED.);
#1490=B_SPLINE_CURVE_WITH_KNOTS('',3,(#27912,#27913,#27914,#27915,#27916,
#27917,#27918,#27919,#27920,#27921,#27922,#27923,#27924,#27925,#27926,#27927,
#27928,#27929,#27930,#27931,#27932,#27933,#27934,#27935,#27936,#27937,#27938,
#27939,#27940,#27941,#27942,#27943,#27944,#27945,#27946,#27947,#27948,#27949,
#27950,#27951,#27952,#27953,#27954,#27955,#27956,#27957,#27958,#27959,#27960,
#27961,#27962,#27963,#27964,#27965,#27966,#27967,#27968,#27969,#27970,#27971,
#27972,#27973,#27974,#27975,#27976,#27977,#27978,#27979,#27980,#27981,#27982,
#27983,#27984,#27985,#27986,#27987,#27988,#27989,#27990,#27991,#27992,#27993),
 .UNSPECIFIED.,.F.,.F.,(4,3,3,3,3,3,3,3,3,3,3,3,3,3,3,3,3,3,3,3,3,3,3,3,
3,3,3,4),(40.840704496801,40.9592420556452,41.0777796144894,41.165625347994,
41.2533608204091,41.3410089927796,41.4316176073812,41.5191681563067,41.606706019416,
41.6942518173877,41.7818261714919,41.869497053947,41.9572256171564,42.0450784914055,
42.0658779095921,42.1537236431118,42.2414591155421,42.3291072879277,42.4197159025236,
42.5072664514642,42.5948043145885,42.6823501125752,42.7699244666943,42.8575953491641,
42.9453239123882,43.0331767866515,43.0539762046948,43.0661513688595),
 .UNSPECIFIED.);
#1491=B_SPLINE_CURVE_WITH_KNOTS('',3,(#27994,#27995,#27996,#27997,#27998,
#27999,#28000,#28001,#28002,#28003,#28004,#28005,#28006,#28007,#28008,#28009,
#28010,#28011,#28012,#28013,#28014,#28015,#28016,#28017,#28018,#28019,#28020,
#28021,#28022,#28023,#28024,#28025,#28026,#28027,#28028,#28029,#28030,#28031,
#28032,#28033,#28034,#28035,#28036,#28037,#28038,#28039,#28040,#28041,#28042,
#28043,#28044,#28045,#28046,#28047,#28048,#28049,#28050,#28051,#28052,#28053,
#28054,#28055,#28056,#28057,#28058,#28059,#28060,#28061,#28062,#28063,#28064,
#28065,#28066,#28067,#28068,#28069,#28070,#28071,#28072,#28073,#28074,#28075,
#28076,#28077,#28078,#28079,#28080,#28081,#28082,#28083,#28084,#28085,#28086,
#28087,#28088,#28089,#28090,#28091,#28092,#28093,#28094,#28095,#28096,#28097,
#28098,#28099,#28100,#28101,#28102,#28103,#28104,#28105,#28106,#28107,#28108,
#28109,#28110,#28111,#28112,#28113,#28114,#28115,#28116,#28117,#28118,#28119,
#28120,#28121,#28122,#28123,#28124,#28125,#28126,#28127,#28128,#28129,#28130,
#28131,#28132,#28133,#28134,#28135,#28136,#28137,#28138,#28139,#28140,#28141),
 .UNSPECIFIED.,.F.,.F.,(4,3,3,3,3,3,3,3,3,3,3,3,3,3,3,3,3,3,3,3,3,3,3,3,
3,3,3,3,3,3,3,3,3,3,3,3,3,3,3,3,3,3,3,3,3,3,3,3,3,4),(36.782489025435,36.8701315883539,
36.9578193726307,37.0456477851092,37.1253864340788,37.2132321678722,37.3009676405799,
37.388615813246,37.4792244277379,37.5667749769658,37.6543128403794,37.7418586386567,
37.8294329930681,37.9171038758305,38.004832439348,38.0926853139034,38.1134847291814,
38.2013304626339,38.2890659349965,38.3767141073143,38.4673227219356,38.5548732708085,
38.6424111338651,38.7299569317841,38.8175312858352,38.9052021682385,38.9929307313962,
39.0807836055944,39.1015830242841,39.1894287577675,39.2771642301606,39.3648124025089,
39.4554210171186,39.5429715660202,39.6305094291052,39.7180552270518,39.8056295811307,
39.8933004635602,39.9810290267434,40.0688819009665,40.0896813193868,40.1764746119568,
40.2631324614172,40.3497129319938,40.4362377296806,40.5227285080445,40.609232549189,
40.6957418296306,40.7823191590372,40.8407044966673),.UNSPECIFIED.);
#1492=B_SPLINE_CURVE_WITH_KNOTS('',3,(#28147,#28148,#28149,#28150,#28151,
#28152,#28153,#28154,#28155,#28156,#28157,#28158,#28159,#28160,#28161,#28162,
#28163,#28164,#28165,#28166,#28167,#28168,#28169,#28170,#28171,#28172,#28173,
#28174,#28175,#28176,#28177,#28178,#28179,#28180,#28181,#28182,#28183,#28184,
#28185,#28186,#28187,#28188,#28189,#28190,#28191,#28192,#28193,#28194,#28195,
#28196,#28197,#28198,#28199,#28200,#28201,#28202,#28203,#28204,#28205,#28206,
#28207,#28208,#28209,#28210,#28211,#28212,#28213,#28214,#28215,#28216,#28217,
#28218,#28219,#28220,#28221,#28222,#28223,#28224,#28225,#28226,#28227,#28228,
#28229,#28230,#28231,#28232,#28233,#28234,#28235,#28236,#28237,#28238,#28239,
#28240,#28241,#28242,#28243,#28244,#28245,#28246,#28247,#28248,#28249,#28250,
#28251,#28252,#28253,#28254,#28255,#28256,#28257,#28258,#28259,#28260,#28261,
#28262,#28263,#28264,#28265,#28266,#28267,#28268,#28269,#28270,#28271,#28272,
#28273,#28274,#28275,#28276,#28277,#28278,#28279,#28280,#28281,#28282,#28283,
#28284,#28285,#28286,#28287,#28288,#28289,#28290,#28291,#28292,#28293,#28294),
 .UNSPECIFIED.,.F.,.F.,(4,3,3,3,3,3,3,3,3,3,3,3,3,3,3,3,3,3,3,3,3,3,3,3,
3,3,3,3,3,3,3,3,3,3,3,3,3,3,3,3,3,3,3,3,3,3,3,3,3,4),(30.4992123502324,
30.5870542145733,30.631405429767,30.7192511601337,30.8069866293569,30.8946347984857,
30.9852434142837,31.0727939598643,31.1603318195962,31.2478776141616,31.3354519648342,
31.4231228438373,31.5108514035789,31.5987042743628,31.6195037248697,31.707349460417,
31.7950849349003,31.8827331093615,31.9733417231879,32.0608922742473,32.1484301395027,
32.2359759396303,32.3235502958981,32.4112211805172,32.4989497458933,32.5868026222967,
32.6076020199723,32.69544775317,32.7831832252783,32.8708313973422,32.9614400120588,
33.0489905606806,33.1365284234879,33.2240742211596,33.311648574966,33.3993194571285,
33.4870480200478,33.5749008940125,33.595700315075,33.6831656270259,33.7705208710584,
33.857789457399,33.9452556738879,34.0324300625443,34.1195929028326,34.2067652159563,
34.2944537092947,34.3817525654606,34.4696358773854,34.5575191893102),
 .UNSPECIFIED.);
#1493=B_SPLINE_CURVE_WITH_KNOTS('',3,(#28295,#28296,#28297,#28298,#28299,
#28300,#28301,#28302,#28303,#28304,#28305,#28306,#28307,#28308,#28309,#28310,
#28311,#28312,#28313,#28314,#28315,#28316,#28317,#28318,#28319,#28320,#28321,
#28322,#28323,#28324,#28325,#28326,#28327,#28328,#28329,#28330,#28331,#28332,
#28333,#28334,#28335,#28336,#28337,#28338,#28339,#28340,#28341,#28342,#28343,
#28344,#28345,#28346,#28347,#28348,#28349,#28350,#28351,#28352,#28353,#28354,
#28355,#28356,#28357,#28358,#28359,#28360,#28361,#28362,#28363,#28364,#28365,
#28366,#28367,#28368,#28369,#28370,#28371,#28372,#28373,#28374,#28375,#28376,
#28377,#28378,#28379),.UNSPECIFIED.,.F.,.F.,(4,3,3,3,3,3,3,3,3,3,3,3,3,
3,3,3,3,3,3,3,3,3,3,3,3,3,3,3,4),(34.5575191894877,34.5837986101777,34.6716443439734,
34.7593798166834,34.8470279893519,34.937636603843,35.0251871530733,35.1127250164892,
35.2002708147692,35.287845169183,35.3755160519479,35.4632446154677,35.5510974900254,
35.5718969052803,35.6597426387321,35.7474781110943,35.8351262834116,35.925734898033,
36.0132854469052,36.1008233099611,36.1883691078795,36.2759434619307,36.3636143443333,
36.4513429074904,36.5391957816878,36.559995200383,36.6478465408607,36.7355748488331,
36.7834594513572),.UNSPECIFIED.);
#1494=B_SPLINE_CURVE_WITH_KNOTS('',3,(#28381,#28382,#28383,#28384,#28385,
#28386,#28387,#28388,#28389,#28390,#28391,#28392,#28393,#28394,#28395,#28396,
#28397,#28398,#28399,#28400,#28401,#28402,#28403,#28404,#28405,#28406,#28407,
#28408,#28409,#28410,#28411,#28412,#28413,#28414,#28415,#28416,#28417,#28418,
#28419,#28420,#28421,#28422,#28423,#28424,#28425,#28426,#28427,#28428,#28429,
#28430,#28431,#28432,#28433,#28434,#28435,#28436,#28437,#28438,#28439,#28440,
#28441,#28442,#28443,#28444,#28445,#28446,#28447,#28448,#28449,#28450,#28451,
#28452,#28453,#28454,#28455,#28456,#28457,#28458,#28459,#28460,#28461,#28462),
 .UNSPECIFIED.,.F.,.F.,(4,3,3,3,3,3,3,3,3,3,3,3,3,3,3,3,3,3,3,3,3,3,3,3,
3,3,3,4),(34.5575191894877,34.6462452281606,34.7349963989685,34.8237912713786,
34.9127093964719,35.001694277295,35.0908349295251,35.1491898438735,35.2370355770745,
35.3247710491863,35.4124192212535,35.5030278359688,35.5905783845939,35.6781162474045,
35.7656620450795,35.8532363988891,35.9409072810548,36.0286358439772,36.1164887179452,
36.1372881389761,36.2251186640309,36.3128459868409,36.4004909011797,36.4880741337705,
36.5756228794804,36.6631518391531,36.7506985294834,36.782489025435),
 .UNSPECIFIED.);
#1495=B_SPLINE_CURVE_WITH_KNOTS('',3,(#28463,#28464,#28465,#28466,#28467,
#28468,#28469,#28470,#28471,#28472,#28473,#28474,#28475,#28476,#28477,#28478,
#28479,#28480,#28481,#28482,#28483,#28484,#28485,#28486,#28487,#28488,#28489,
#28490,#28491,#28492,#28493,#28494,#28495,#28496,#28497,#28498,#28499,#28500,
#28501,#28502,#28503,#28504,#28505,#28506,#28507,#28508,#28509,#28510,#28511,
#28512,#28513,#28514,#28515,#28516,#28517,#28518,#28519,#28520,#28521,#28522,
#28523,#28524,#28525,#28526,#28527,#28528,#28529,#28530,#28531,#28532,#28533,
#28534,#28535,#28536,#28537,#28538,#28539,#28540,#28541,#28542,#28543,#28544,
#28545,#28546,#28547,#28548,#28549,#28550,#28551,#28552,#28553,#28554,#28555,
#28556,#28557,#28558,#28559,#28560,#28561,#28562,#28563,#28564,#28565,#28566,
#28567,#28568,#28569,#28570,#28571,#28572,#28573,#28574,#28575,#28576,#28577,
#28578,#28579,#28580,#28581,#28582,#28583,#28584,#28585,#28586,#28587,#28588,
#28589,#28590,#28591,#28592,#28593,#28594,#28595,#28596,#28597,#28598,#28599,
#28600,#28601,#28602,#28603,#28604,#28605,#28606,#28607),.UNSPECIFIED.,
 .F.,.F.,(4,3,3,3,3,3,3,3,3,3,3,3,3,3,3,3,3,3,3,3,3,3,3,3,3,3,3,3,3,3,3,
3,3,3,3,3,3,3,3,3,3,3,3,3,3,3,3,3,4),(30.5002119601245,30.5877840746677,
30.6753288207514,30.7628668275658,30.8504187144882,30.9380598353038,31.0257454406997,
31.1135727002447,31.1967966634628,31.2846424112103,31.3723778980337,31.4600260849591,
31.5506346941599,31.6381852579116,31.7257231359216,31.8132689488522,31.9008433179572,
31.9885142154005,32.0762427936085,32.1640956827569,32.1848949585655,32.2727406910854,
32.3604761625352,32.4481243339609,32.5387329489243,32.6262834969632,32.7138213592091,
32.8013671563419,32.888941509632,32.9766123913153,33.0643409537762,33.1521938273171,
33.1729932536681,33.2608389840538,33.3485744532963,33.4362226224444,33.5268312382352,
33.614381783836,33.7019196435887,33.7894654381741,33.8770397888678,33.9647106678921,
34.0524392276545,34.1402920984597,34.1610915487708,34.2601984589017,34.3572237828832,
34.4573714860888,34.5575191892943),.UNSPECIFIED.);
#1496=B_SPLINE_CURVE_WITH_KNOTS('',3,(#28613,#28614,#28615,#28616,#28617,
#28618,#28619,#28620,#28621,#28622,#28623,#28624,#28625,#28626,#28627,#28628,
#28629,#28630,#28631,#28632,#28633,#28634,#28635,#28636,#28637,#28638,#28639,
#28640,#28641,#28642,#28643,#28644,#28645,#28646,#28647,#28648,#28649,#28650,
#28651,#28652,#28653,#28654,#28655,#28656,#28657,#28658,#28659,#28660,#28661,
#28662,#28663,#28664,#28665,#28666,#28667,#28668,#28669,#28670,#28671,#28672,
#28673,#28674,#28675,#28676,#28677,#28678,#28679,#28680,#28681,#28682,#28683,
#28684,#28685,#28686,#28687,#28688,#28689,#28690,#28691,#28692,#28693,#28694,
#28695,#28696,#28697,#28698,#28699,#28700,#28701,#28702,#28703,#28704,#28705,
#28706,#28707,#28708,#28709,#28710,#28711,#28712,#28713,#28714,#28715,#28716,
#28717,#28718,#28719,#28720,#28721,#28722,#28723,#28724,#28725,#28726,#28727,
#28728,#28729,#28730,#28731,#28732,#28733,#28734,#28735,#28736,#28737,#28738,
#28739,#28740,#28741,#28742,#28743,#28744,#28745,#28746,#28747,#28748,#28749,
#28750,#28751,#28752,#28753,#28754,#28755,#28756,#28757,#28758,#28759,#28760),
 .UNSPECIFIED.,.F.,.F.,(4,3,3,3,3,3,3,3,3,3,3,3,3,3,3,3,3,3,3,3,3,3,3,3,
3,3,3,3,3,3,3,3,3,3,3,3,3,3,3,3,3,3,3,3,3,3,3,3,3,4),(24.2165026702176,
24.304043926345,24.3916073461436,24.479264250075,24.5669730854259,24.6548135226413,
24.702815659151,24.7906611702751,24.8783964169397,24.9660443604867,25.0566530597075,
25.1442033736151,25.2317409998204,25.3192865592566,25.406860673447,25.4945313151421,
25.5822596368198,25.6701122702235,25.6909139542537,25.7787597849543,25.8664953555964,
25.9541436270979,26.0447522048802,26.1323028545467,26.2198408188163,26.3073867182571,
26.3949611740288,26.4826321579353,26.5703608225863,26.6582137974992,26.6790122493564,
26.7668579861124,26.854593462076,26.9422416382858,27.0328502515574,27.1204008050279,
27.2079386729366,27.2954844759584,27.3830588353586,27.470729723451,27.5584582925036,
27.6463111728529,27.667110544459,27.7558874872272,27.844547755712,27.9331107998525,
28.02158503414,28.1100063153203,28.198402509401,28.2743338823081),
 .UNSPECIFIED.);
#1497=B_SPLINE_CURVE_WITH_KNOTS('',3,(#28761,#28762,#28763,#28764,#28765,
#28766,#28767,#28768,#28769,#28770,#28771,#28772,#28773,#28774,#28775,#28776,
#28777,#28778,#28779,#28780,#28781,#28782,#28783,#28784,#28785,#28786,#28787,
#28788,#28789,#28790,#28791,#28792,#28793,#28794,#28795,#28796,#28797,#28798,
#28799,#28800,#28801,#28802,#28803,#28804,#28805,#28806,#28807,#28808,#28809,
#28810,#28811,#28812,#28813,#28814,#28815,#28816,#28817,#28818,#28819,#28820,
#28821,#28822,#28823,#28824,#28825,#28826,#28827,#28828,#28829,#28830,#28831,
#28832,#28833,#28834,#28835,#28836,#28837,#28838,#28839),.UNSPECIFIED.,
 .F.,.F.,(4,3,3,3,3,3,3,3,3,3,3,3,3,3,3,3,3,3,3,3,3,3,3,3,3,3,4),(28.274333882515,
28.3719019718884,28.4698037533802,28.5681844676917,28.6552088395617,28.7430545874032,
28.8307900743218,28.9184382613433,29.0090468705085,29.0965974343581,29.1841353124666,
29.271681125496,29.3592554947003,29.4469263922428,29.5346549705495,29.6225078597965,
29.6433071346644,29.731160848353,29.8189024061471,29.9065417520996,29.9941237136733,
30.0816689585669,30.169198122729,30.2567665282248,30.34435384216,30.4320320091579,
30.4992123502324),.UNSPECIFIED.);
#1498=B_SPLINE_CURVE_WITH_KNOTS('',3,(#28841,#28842,#28843,#28844,#28845,
#28846,#28847,#28848,#28849,#28850,#28851,#28852,#28853,#28854,#28855,#28856,
#28857,#28858,#28859,#28860,#28861,#28862,#28863,#28864,#28865,#28866,#28867,
#28868,#28869,#28870,#28871,#28872,#28873,#28874,#28875,#28876,#28877,#28878,
#28879,#28880,#28881,#28882,#28883,#28884,#28885,#28886,#28887,#28888,#28889,
#28890,#28891,#28892,#28893,#28894,#28895,#28896,#28897,#28898,#28899,#28900,
#28901,#28902,#28903,#28904,#28905,#28906,#28907,#28908,#28909,#28910,#28911,
#28912,#28913,#28914,#28915,#28916,#28917,#28918,#28919,#28920,#28921,#28922),
 .UNSPECIFIED.,.F.,.F.,(4,3,3,3,3,3,3,3,3,3,3,3,3,3,3,3,3,3,3,3,3,3,3,3,
3,3,3,4),(28.2743338824402,28.3615964636159,28.4487512272485,28.5358217800874,
28.6228345545296,28.709817282874,28.796791179032,28.883777445679,28.970850571241,
29.0579679319872,29.1452235371721,29.2206000732575,29.3084458100498,29.3961812860485,
29.4838294622926,29.5744380755511,29.6619886290536,29.7495264969936,29.8370723000451,
29.9246466594751,30.0123175475949,30.1000461166736,30.1878989970478,30.2086983683601,
30.2965346095156,30.3842739178244,30.471919062604,30.5002119601245),
 .UNSPECIFIED.);
#1499=B_SPLINE_CURVE_WITH_KNOTS('',3,(#28923,#28924,#28925,#28926,#28927,
#28928,#28929,#28930,#28931,#28932,#28933,#28934,#28935,#28936,#28937,#28938,
#28939,#28940,#28941,#28942,#28943,#28944,#28945,#28946,#28947,#28948,#28949,
#28950,#28951,#28952,#28953,#28954,#28955,#28956,#28957,#28958,#28959,#28960,
#28961,#28962,#28963,#28964,#28965,#28966,#28967,#28968,#28969,#28970,#28971,
#28972,#28973,#28974,#28975,#28976,#28977,#28978,#28979,#28980,#28981,#28982,
#28983,#28984,#28985,#28986,#28987,#28988,#28989,#28990,#28991,#28992,#28993,
#28994,#28995,#28996,#28997,#28998,#28999,#29000,#29001,#29002,#29003,#29004,
#29005,#29006,#29007,#29008,#29009,#29010,#29011,#29012,#29013,#29014,#29015,
#29016,#29017,#29018,#29019,#29020,#29021,#29022,#29023,#29024,#29025,#29026,
#29027,#29028,#29029,#29030,#29031,#29032,#29033,#29034,#29035,#29036,#29037,
#29038,#29039,#29040,#29041,#29042,#29043,#29044,#29045,#29046,#29047,#29048,
#29049,#29050,#29051,#29052,#29053,#29054,#29055,#29056,#29057,#29058,#29059,
#29060,#29061,#29062,#29063,#29064,#29065,#29066,#29067,#29068,#29069,#29070,
#29071,#29072,#29073),.UNSPECIFIED.,.F.,.F.,(4,3,3,3,3,3,3,3,3,3,3,3,3,
3,3,3,3,3,3,3,3,3,3,3,3,3,3,3,3,3,3,3,3,3,3,3,3,3,3,3,3,3,3,3,3,3,3,3,3,
3,4),(24.2162169687424,24.2801085977442,24.3679525734171,24.4556862627458,
24.5433326291174,24.6339419120835,24.7214906094836,24.809026607426,24.8965705285987,
24.9841429962742,25.0718119874431,25.1595386543509,25.2473896392159,25.2682068928468,
25.3560532509127,25.443789353695,25.531438161423,25.6220465397388,25.7095977323268,
25.7971362410408,25.8846826858492,25.9722576873129,26.0599292146498,26.1476584220326,
26.2355119345706,26.2563051879495,26.3441510274158,26.4318866090919,26.5195348938718,
26.6101434675193,26.6976941360126,26.7852321211407,26.8727780434585,26.9603525241144,
27.0480235357698,27.1357522298776,27.2236052365278,27.2444034830521,27.332248995167,
27.4199842428374,27.507632187404,27.5982408862479,27.6857912012032,27.7733288284647,
27.8608743889645,27.9484485042248,28.0361191469941,28.1238474697496,28.2117001042282,
28.2325017781548,28.2743338823081),.UNSPECIFIED.);
#1500=B_SPLINE_CURVE_WITH_KNOTS('',3,(#29079,#29080,#29081,#29082,#29083,
#29084,#29085,#29086,#29087,#29088,#29089,#29090,#29091,#29092,#29093,#29094,
#29095,#29096,#29097,#29098,#29099,#29100,#29101,#29102,#29103,#29104,#29105,
#29106,#29107,#29108,#29109,#29110,#29111,#29112,#29113,#29114,#29115,#29116,
#29117,#29118,#29119,#29120,#29121,#29122,#29123,#29124,#29125,#29126,#29127,
#29128,#29129,#29130,#29131,#29132,#29133,#29134,#29135,#29136,#29137,#29138,
#29139,#29140,#29141,#29142,#29143,#29144,#29145,#29146,#29147,#29148,#29149,
#29150,#29151,#29152,#29153,#29154,#29155,#29156,#29157,#29158,#29159,#29160),
 .UNSPECIFIED.,.F.,.F.,(4,3,3,3,3,3,3,3,3,3,3,3,3,3,3,3,3,3,3,3,3,3,3,3,
3,3,3,4),(15.7079632679489,15.7947000247825,15.8814152765578,15.9681303731201,
16.0548666599654,16.1417000066177,16.2285855560594,16.3156125279741,16.3753222369229,
16.4632671529562,16.551101682674,16.6388486586907,16.7294201428575,16.8170681804461,
16.904702862179,16.9923446932266,17.0800141787253,17.1677783645445,17.2555992653293,
17.3435423677208,17.3634205320255,17.4513971777302,17.5392714562485,17.6270639960291,
17.7147927338977,17.8024841872462,17.8901701658632,17.9330836177785),
 .UNSPECIFIED.);
#1501=B_SPLINE_CURVE_WITH_KNOTS('',3,(#29162,#29163,#29164,#29165,#29166),
 .UNSPECIFIED.,.F.,.F.,(4,1,4),(14.3991256467175,15.3872239418202,15.7079550816507),
 .UNSPECIFIED.);
#1502=B_SPLINE_CURVE_WITH_KNOTS('',3,(#29170,#29171,#29172,#29173,#29174,
#29175,#29176,#29177,#29178,#29179,#29180,#29181,#29182,#29183,#29184,#29185,
#29186,#29187,#29188,#29189,#29190,#29191,#29192,#29193,#29194,#29195,#29196,
#29197,#29198,#29199,#29200,#29201,#29202,#29203,#29204,#29205,#29206,#29207,
#29208,#29209,#29210,#29211,#29212,#29213,#29214,#29215,#29216,#29217,#29218,
#29219,#29220,#29221,#29222,#29223,#29224,#29225,#29226,#29227,#29228,#29229,
#29230,#29231,#29232,#29233,#29234,#29235,#29236),.UNSPECIFIED.,.F.,.F.,
(4,3,3,3,3,3,3,3,3,3,3,3,3,3,3,3,3,3,3,3,3,3,4),(13.8752089252097,13.9625451768154,
14.0497728503132,14.1369154800046,14.2239988322353,14.3110512064015,14.3980937504697,
14.4851476003848,14.5722863531229,14.6594683187599,14.7467864178897,14.8218327081244,
14.9086977820188,14.9954555529545,15.0845190173028,15.1711346234622,15.2577220080351,
15.3443027284837,15.435217863298,15.5218933969664,15.6086174094582,15.6954502207414,
15.7079632677406),.UNSPECIFIED.);
#1503=B_SPLINE_CURVE_WITH_KNOTS('',3,(#29237,#29238,#29239,#29240,#29241,
#29242,#29243,#29244,#29245,#29246,#29247,#29248,#29249,#29250,#29251,#29252,
#29253,#29254,#29255,#29256,#29257,#29258,#29259,#29260,#29261,#29262,#29263,
#29264,#29265,#29266,#29267,#29268,#29269,#29270,#29271,#29272,#29273,#29274,
#29275,#29276,#29277,#29278,#29279,#29280,#29281,#29282,#29283,#29284,#29285,
#29286,#29287,#29288,#29289,#29290,#29291,#29292,#29293,#29294,#29295,#29296,
#29297,#29298,#29299,#29300,#29301,#29302,#29303,#29304,#29305,#29306,#29307,
#29308,#29309,#29310,#29311,#29312,#29313,#29314,#29315,#29316,#29317,#29318),
 .UNSPECIFIED.,.F.,.F.,(4,3,3,3,3,3,3,3,3,3,3,3,3,3,3,3,3,3,3,3,3,3,3,3,
3,3,3,4),(15.7079632679489,15.8099310032271,15.8976761278721,15.985309708943,
16.0728548384208,16.1635016459094,16.2509469329345,16.3383788932871,16.4258182602526,
16.5132857674034,16.6008497171709,16.6884711726235,16.7762174884443,16.7980292983297,
16.8858955432857,16.9736516099389,17.0613204330381,17.1519213280874,17.2394925318178,
17.3270510142323,17.4146173727509,17.5022122053289,17.589903340914,17.6776520485815,
17.7655247566336,17.7861275934324,17.873977809986,17.9338553089788),
 .UNSPECIFIED.);
#1504=B_SPLINE_CURVE_WITH_KNOTS('',3,(#29324,#29325,#29326,#29327,#29328,
#29329,#29330,#29331,#29332,#29333,#29334,#29335,#29336,#29337,#29338,#29339,
#29340,#29341,#29342,#29343,#29344,#29345,#29346,#29347,#29348,#29349,#29350,
#29351,#29352,#29353,#29354,#29355,#29356,#29357,#29358,#29359,#29360,#29361,
#29362,#29363),.UNSPECIFIED.,.F.,.F.,(4,3,3,3,3,3,3,3,3,3,3,3,3,4),(-55.2918140047847,
-55.200308089966,-55.1089206909327,-55.013481383397,-54.9222481364232,-54.8310438513113,
-54.7398442083826,-54.6486248978994,-54.5573105633689,-54.4659402820255,
-54.3744361879659,-54.3454062306465,-54.2237243441527,-54.1159079025692),
 .UNSPECIFIED.);
#1505=B_SPLINE_CURVE_WITH_KNOTS('',3,(#29365,#29366,#29367,#29368,#29369,
#29370,#29371,#29372,#29373,#29374),.UNSPECIFIED.,.F.,.F.,(4,1,1,1,1,1,
1,4),(-54.1159079025692,-53.3573079355439,-52.3692096404412,-51.3811113453385,
-50.3930130502359,-49.4049147551332,-48.4168164600305,-47.8327225953897),
 .UNSPECIFIED.);
#1506=B_SPLINE_CURVE_WITH_KNOTS('',3,(#29376,#29377,#29378,#29379,#29380,
#29381,#29382,#29383,#29384,#29385,#29386,#29387,#29388,#29389,#29390,#29391,
#29392,#29393,#29394,#29395,#29396,#29397,#29398,#29399,#29400,#29401,#29402,
#29403,#29404,#29405,#29406,#29407,#29408,#29409,#29410,#29411,#29412,#29413,
#29414,#29415,#29416,#29417,#29418,#29419,#29420,#29421,#29422,#29423,#29424,
#29425,#29426,#29427,#29428,#29429,#29430,#29431,#29432,#29433,#29434,#29435,
#29436,#29437,#29438,#29439,#29440,#29441,#29442,#29443,#29444,#29445,#29446,
#29447,#29448,#29449,#29450,#29451,#29452,#29453,#29454,#29455,#29456,#29457,
#29458,#29459,#29460,#29461,#29462,#29463,#29464,#29465,#29466,#29467,#29468,
#29469,#29470,#29471,#29472,#29473,#29474,#29475,#29476,#29477,#29478,#29479,
#29480,#29481,#29482,#29483,#29484,#29485,#29486,#29487,#29488,#29489,#29490,
#29491,#29492,#29493,#29494,#29495,#29496,#29497,#29498,#29499,#29500,#29501,
#29502,#29503,#29504,#29505,#29506,#29507,#29508,#29509,#29510,#29511,#29512,
#29513,#29514,#29515,#29516,#29517,#29518,#29519,#29520,#29521,#29522,#29523,
#29524,#29525,#29526,#29527,#29528,#29529,#29530,#29531,#29532,#29533,#29534,
#29535,#29536,#29537,#29538,#29539,#29540,#29541,#29542,#29543,#29544,#29545,
#29546,#29547,#29548,#29549,#29550,#29551,#29552,#29553,#29554,#29555,#29556,
#29557,#29558,#29559,#29560,#29561,#29562,#29563,#29564,#29565,#29566,#29567,
#29568,#29569,#29570,#29571,#29572,#29573,#29574,#29575,#29576,#29577,#29578,
#29579,#29580,#29581,#29582,#29583,#29584,#29585,#29586,#29587,#29588,#29589,
#29590,#29591,#29592,#29593,#29594,#29595,#29596,#29597,#29598,#29599,#29600,
#29601,#29602,#29603,#29604,#29605,#29606,#29607,#29608,#29609,#29610,#29611,
#29612,#29613,#29614,#29615,#29616,#29617,#29618,#29619,#29620,#29621,#29622,
#29623,#29624,#29625,#29626,#29627,#29628,#29629,#29630,#29631,#29632,#29633,
#29634,#29635,#29636,#29637,#29638,#29639,#29640,#29641,#29642,#29643,#29644,
#29645,#29646,#29647,#29648,#29649,#29650,#29651,#29652,#29653,#29654,#29655,
#29656,#29657,#29658,#29659,#29660,#29661,#29662,#29663,#29664,#29665,#29666,
#29667,#29668,#29669,#29670,#29671,#29672,#29673,#29674,#29675,#29676,#29677,
#29678,#29679,#29680,#29681,#29682,#29683,#29684,#29685,#29686,#29687,#29688,
#29689,#29690,#29691,#29692,#29693,#29694,#29695,#29696,#29697,#29698,#29699,
#29700,#29701,#29702,#29703,#29704,#29705,#29706,#29707,#29708,#29709,#29710,
#29711,#29712,#29713,#29714,#29715,#29716,#29717,#29718,#29719),
 .UNSPECIFIED.,.F.,.F.,(4,2,2,2,2,2,2,2,2,2,2,2,2,2,2,2,2,2,2,2,2,2,2,2,
2,2,2,2,2,2,2,2,2,2,2,2,2,2,2,2,2,2,2,2,2,2,2,2,2,2,2,2,2,2,2,2,2,2,2,2,
2,2,2,2,2,2,2,2,2,2,2,2,2,2,2,2,2,2,2,2,2,2,2,2,2,2,2,2,2,2,2,2,2,2,2,2,
2,2,2,2,2,2,2,2,2,2,2,2,2,2,2,2,2,2,2,2,2,2,2,2,2,2,2,2,2,2,2,2,2,2,2,2,
2,2,2,2,2,2,2,2,2,2,2,2,2,2,2,2,2,2,2,2,2,2,2,2,2,2,2,2,2,2,2,2,2,2,2,2,
2,2,2,4),(-4.26994477188097,-4.18620642098893,-4.14748543155145,-4.13836516395927,
-4.13271644558837,-4.1270209789431,-4.11767887414803,-4.07387176272375,
-4.01754675939132,-3.98526852873032,-3.97244252517069,-3.962928101753,-3.95263455188417,
-3.93561297279341,-3.86906486919751,-3.83032039001781,-3.80888467938486,
-3.80115287219542,-3.79576180824508,-3.78960303190388,-3.77835581422881,
-3.7362332495788,-3.68241613757305,-3.64973455052119,-3.63685676513584,
-3.62733391275226,-3.61705919469465,-3.60013604758476,-3.53178867699976,
-3.49419379877283,-3.4731285686711,-3.46544214860115,-3.46005724725163,
-3.45387538386639,-3.44251852409717,-3.39772741841958,-3.35693498688948,
-3.3294400047532,-3.30871723415067,-3.29770329336156,-3.28926037190288,
-3.27811268307046,-3.25732552411916,-3.18265367848997,-3.14387805607392,
-3.13291347210378,-3.12687793802281,-3.1215052928004,-3.11482851828834,
-3.09758541865381,-3.01707586610079,-2.97968868891503,-2.96627243337736,
-2.95666593248693,-2.9465806454064,-2.93060660716385,-2.84360477723358,
-2.80473702597104,-2.79560979365303,-2.7899593655879,-2.78426455654238,
-2.77492746042689,-2.73211187317539,-2.67505866187918,-2.64257356381414,
-2.62972052078187,-2.62020133905442,-2.60991692082377,-2.59294487551698,
-2.52538738746047,-2.48729318260763,-2.46606554778313,-2.45835895299769,
-2.4529712260203,-2.4467995486916,-2.43549124031871,-2.39171201103291,-2.35042959737762,
-2.30917187563767,-2.29538278530595,-2.2857123488288,-2.27573191572309,
-2.26029141076709,-2.17923413867982,-2.14829963663161,-2.13533478824122,
-2.12516345695904,-2.11929233086499,-2.11377547208397,-2.10531130332818,
-2.07676876291054,-2.00666750220054,-1.97247547910195,-1.95909672289662,
-1.94959075765524,-1.93951659775975,-1.92360179357811,-1.8514479429695,
-1.80226477432625,-1.79069313230599,-1.78446566593839,-1.77909249592087,
-1.7714923613653,-1.7511068894382,-1.71554791286426,-1.64362474358197,-1.62699472507492,
-1.61677806746921,-1.60723191970796,-1.594200400812,-1.56026258045255,-1.49766369007068,
-1.461899074237,-1.45279208968934,-1.44714568458261,-1.4414459482241,-1.43208640880257,
-1.38696841275484,-1.3053997793046,-1.29002649639216,-1.2800590989145,-1.2703795523322,
-1.25653905821626,-1.2146844741299,-1.17235755187968,-1.1302969132056,-1.11905357834372,
-1.11289563802632,-1.10750398798881,-1.09976958887906,-1.07831825775197,
-1.03952673566653,-0.972988352111049,-0.955961612124122,-0.945666289777868,
-0.936151098026857,-0.923325275213903,-0.891051311495818,-0.834734568395268,
-0.790981030348268,-0.781640398928958,-0.775944849883415,-0.77029522471581,
-0.761171506665113,-0.722397011506791,-0.63515619010766,-0.619222062684149,
-0.609144749818193,-0.599534133867639,-0.586092366400709,-0.548451508328222,
-0.466073284500351,-0.449999401583243,-0.443099403504667,-0.437782511925628,
-0.43116817181859,-0.417199430816387,-0.39719431811366,-0.321105245779795,
-0.292257616498562,-0.28080797748469,-0.271268815467881,-0.261256811036364,
-0.245652941595711,-0.183326665219496,-0.122229251623277,-0.111399598244366,
-0.105391929826403,-0.0999461477571767,-0.0918711243274098,-0.067426883443743,
-0.000960198174506648),.UNSPECIFIED.);
#1507=B_SPLINE_CURVE_WITH_KNOTS('',3,(#29721,#29722,#29723,#29724,#29725,
#29726,#29727,#29728,#29729,#29730,#29731,#29732,#29733,#29734,#29735,#29736,
#29737,#29738,#29739,#29740,#29741,#29742,#29743,#29744,#29745,#29746,#29747,
#29748,#29749,#29750,#29751,#29752,#29753,#29754,#29755,#29756,#29757,#29758,
#29759,#29760,#29761,#29762,#29763,#29764,#29765,#29766,#29767,#29768,#29769,
#29770,#29771,#29772,#29773,#29774,#29775,#29776,#29777,#29778,#29779,#29780,
#29781,#29782,#29783,#29784,#29785,#29786,#29787,#29788,#29789,#29790,#29791,
#29792,#29793,#29794,#29795,#29796,#29797,#29798,#29799,#29800,#29801,#29802,
#29803,#29804,#29805,#29806,#29807,#29808,#29809,#29810,#29811,#29812,#29813,
#29814,#29815,#29816,#29817,#29818,#29819,#29820,#29821,#29822,#29823,#29824,
#29825,#29826,#29827,#29828,#29829,#29830,#29831,#29832,#29833,#29834,#29835,
#29836,#29837,#29838,#29839,#29840,#29841,#29842,#29843,#29844,#29845,#29846,
#29847,#29848,#29849,#29850,#29851,#29852,#29853,#29854,#29855,#29856,#29857,
#29858,#29859,#29860,#29861,#29862,#29863,#29864,#29865,#29866,#29867,#29868,
#29869,#29870,#29871,#29872,#29873,#29874,#29875,#29876,#29877,#29878,#29879,
#29880,#29881,#29882,#29883,#29884,#29885,#29886,#29887,#29888,#29889,#29890,
#29891,#29892,#29893,#29894,#29895,#29896,#29897,#29898,#29899,#29900,#29901,
#29902,#29903,#29904,#29905,#29906,#29907,#29908,#29909,#29910,#29911,#29912,
#29913,#29914,#29915,#29916,#29917,#29918,#29919,#29920,#29921,#29922,#29923,
#29924,#29925,#29926,#29927,#29928,#29929,#29930,#29931,#29932,#29933,#29934,
#29935,#29936,#29937,#29938,#29939,#29940,#29941,#29942,#29943,#29944,#29945,
#29946,#29947,#29948,#29949,#29950,#29951,#29952,#29953,#29954,#29955,#29956,
#29957,#29958,#29959,#29960,#29961,#29962,#29963,#29964,#29965,#29966,#29967,
#29968,#29969,#29970,#29971,#29972,#29973,#29974,#29975,#29976,#29977,#29978,
#29979,#29980,#29981,#29982,#29983,#29984,#29985,#29986,#29987,#29988,#29989,
#29990,#29991,#29992,#29993,#29994,#29995,#29996,#29997,#29998,#29999,#30000,
#30001,#30002,#30003,#30004,#30005,#30006,#30007,#30008,#30009,#30010,#30011,
#30012,#30013,#30014,#30015,#30016,#30017,#30018,#30019,#30020,#30021,#30022,
#30023,#30024,#30025,#30026,#30027,#30028,#30029,#30030,#30031,#30032,#30033,
#30034,#30035,#30036,#30037,#30038,#30039,#30040,#30041,#30042,#30043,#30044,
#30045,#30046,#30047,#30048,#30049,#30050,#30051,#30052,#30053,#30054,#30055,
#30056,#30057,#30058,#30059,#30060,#30061,#30062,#30063,#30064,#30065,#30066,
#30067,#30068,#30069,#30070,#30071,#30072),.UNSPECIFIED.,.F.,.F.,(4,2,2,
2,2,2,2,2,2,2,2,2,2,2,2,2,2,2,2,2,2,2,2,2,2,2,2,2,2,2,2,2,2,2,2,2,2,2,2,
2,2,2,2,2,2,2,2,2,2,2,2,2,2,2,2,2,2,2,2,2,2,2,2,2,2,2,2,2,2,2,2,2,2,2,2,
2,2,2,2,2,2,2,2,2,2,2,2,2,2,2,2,2,2,2,2,2,2,2,2,2,2,2,2,2,2,2,2,2,2,2,2,
2,2,2,2,2,2,2,2,2,2,2,2,2,2,2,2,2,2,2,2,2,2,2,2,2,2,2,2,2,2,2,2,2,2,2,2,
2,2,2,2,2,2,2,2,2,2,2,2,2,2,2,2,2,2,2,2,2,2,2,2,2,2,2,2,4),(-4.27059191801562,
-4.24196876919374,-4.22385973473245,-4.21436402168296,-4.2047751676493,
-4.1946519009215,-4.17849128458808,-4.10207530338911,-4.05747736067456,
-4.04585741665701,-4.03968862220837,-4.03429922385486,-4.02658418269025,
-4.00679767812497,-3.9310481657219,-3.89246027380088,-3.87892045828133,
-3.86929214802734,-3.86044047903144,-3.8457657369372,-3.79189565768603,
-3.74022540558451,-3.7152300526998,-3.70709742187507,-3.70164114629446,
-3.69565476708377,-3.68493039532081,-3.61049175689382,-3.57596808241161,
-3.55175292576472,-3.5401162660358,-3.53072659874922,-3.51975526209588,
-3.49985900339185,-3.42410203867415,-3.38181942257708,-3.37255216081011,
-3.36687202864412,-3.36120720764951,-3.35201198631407,-3.31420107234795,
-3.25323492456459,-3.21970159510757,-3.2067186663568,-3.19718017740198,
-3.18694605318795,-3.17022679534539,-3.09929802141095,-3.04794558651569,
-3.03769477720689,-3.03180690703177,-3.02636517558088,-3.01801162993682,
-2.99289972927415,-2.92837390344399,-2.88610869428038,-2.87223170651612,
-2.86254525807201,-2.85258627550684,-2.83725810609607,-2.75543053189016,
-2.71051949034609,-2.70116659430284,-2.69546802786206,-2.69049786443901,
-2.68204508448587,-2.65583878926124,-2.59236284249322,-2.55030675706438,
-2.53644714973095,-2.52676350204291,-2.51797328147161,-2.50366247518195,
-2.46132376792588,-2.39983496424085,-2.37276281360786,-2.36442868823619,
-2.35893608386402,-2.35302212044934,-2.34264660271004,-2.27692567609068,
-2.21880559498243,-2.20296746036063,-2.19290845743233,-2.18339444586113,
-2.16996592539066,-2.13525690721975,-2.06667648989202,-2.03778568923793,
-2.02909722412373,-2.02408557196433,-2.01844794309958,-2.00938220832573,
-1.97181297484136,-1.88660392951311,-1.86890798361453,-1.85847973501213,
-1.8490062034207,-1.83648414335042,-1.80649587787756,-1.75750249923547,
-1.70720830751179,-1.69585139718436,-1.68966948180517,-1.68428492311556,
-1.67659913041973,-1.65553851933186,-1.6179587234071,-1.54951016229661,
-1.53258769638991,-1.52231333433264,-1.51279091052716,-1.49991386167171,
-1.46723239588009,-1.41340729504675,-1.37135559917556,-1.36011268812664,
-1.35395488018644,-1.34856327250305,-1.34082883144026,-1.31937668193981,
-1.28058225159961,-1.21404980802564,-1.19702304675881,-1.18672779987367,
-1.17721273327544,-1.16438716502752,-1.13211441026811,-1.07580124171744,
-1.03204421945698,-1.02270368075276,-1.01700819448616,-1.01135863898363,
-1.00223504342647,-0.963461333270413,-0.876220907429709,-0.860287097017765,
-0.850209928659237,-0.840599412291213,-0.8271577199114,-0.789516498328059,
-0.707133350560775,-0.691064464453122,-0.684165315413099,-0.678848525449104,
-0.672233600903381,-0.658261341206739,-0.638249000282644,-0.562076359109543,
-0.533305600417685,-0.521863388103103,-0.51232601324372,-0.502311323061108,
-0.48669338720172,-0.426505026314306,-0.362914715334719,-0.352305199504254,
-0.346343060858523,-0.340876490943651,-0.332682258085611,-0.307070922609296,
-0.252718367043309,-0.202067395795723,-0.187470412963257,-0.178632854184781,
-0.168995201225525,-0.155394106272744,-0.116158525585101,-0.0675072931087099,
-0.0670493361224295,-0.0450770216706815,-0.022366969529527,-0.0144508372849338,
-0.00907719224608754,-0.0047451534040328,-0.000959030470956043),
 .UNSPECIFIED.);
#1508=B_SPLINE_CURVE_WITH_KNOTS('',3,(#30074,#30075,#30076,#30077,#30078,
#30079,#30080,#30081,#30082,#30083,#30084,#30085,#30086,#30087,#30088,#30089,
#30090,#30091,#30092,#30093,#30094,#30095,#30096,#30097,#30098,#30099,#30100,
#30101,#30102,#30103,#30104,#30105,#30106,#30107,#30108,#30109,#30110,#30111,
#30112,#30113,#30114,#30115,#30116,#30117,#30118,#30119,#30120,#30121,#30122,
#30123,#30124,#30125,#30126,#30127,#30128,#30129,#30130,#30131,#30132,#30133,
#30134,#30135,#30136,#30137,#30138,#30139,#30140,#30141,#30142,#30143,#30144,
#30145,#30146,#30147,#30148,#30149,#30150,#30151,#30152,#30153,#30154,#30155,
#30156,#30157,#30158,#30159,#30160,#30161,#30162,#30163,#30164,#30165,#30166,
#30167,#30168,#30169,#30170,#30171,#30172,#30173,#30174,#30175,#30176,#30177,
#30178,#30179,#30180,#30181,#30182,#30183,#30184,#30185,#30186,#30187,#30188,
#30189,#30190,#30191,#30192,#30193,#30194,#30195,#30196,#30197,#30198,#30199,
#30200,#30201,#30202,#30203,#30204,#30205,#30206,#30207,#30208,#30209,#30210,
#30211,#30212,#30213,#30214,#30215,#30216,#30217,#30218,#30219,#30220,#30221,
#30222,#30223,#30224,#30225,#30226,#30227,#30228,#30229,#30230,#30231,#30232,
#30233,#30234,#30235,#30236,#30237,#30238,#30239,#30240,#30241,#30242,#30243,
#30244,#30245,#30246,#30247,#30248,#30249,#30250,#30251,#30252,#30253,#30254,
#30255,#30256,#30257,#30258,#30259,#30260,#30261,#30262,#30263,#30264,#30265,
#30266,#30267,#30268,#30269,#30270,#30271,#30272,#30273,#30274,#30275,#30276,
#30277,#30278,#30279,#30280,#30281,#30282,#30283,#30284,#30285,#30286,#30287,
#30288,#30289,#30290,#30291,#30292,#30293,#30294,#30295,#30296,#30297,#30298,
#30299,#30300,#30301,#30302,#30303,#30304,#30305,#30306,#30307,#30308,#30309,
#30310,#30311,#30312,#30313,#30314,#30315,#30316,#30317,#30318,#30319,#30320,
#30321,#30322,#30323,#30324,#30325,#30326,#30327,#30328,#30329,#30330,#30331,
#30332,#30333,#30334,#30335,#30336,#30337,#30338,#30339,#30340,#30341,#30342,
#30343,#30344,#30345,#30346,#30347,#30348,#30349,#30350,#30351,#30352,#30353,
#30354,#30355,#30356,#30357,#30358,#30359,#30360,#30361,#30362,#30363,#30364,
#30365,#30366,#30367,#30368,#30369,#30370,#30371,#30372,#30373,#30374,#30375,
#30376,#30377,#30378,#30379,#30380,#30381,#30382,#30383,#30384,#30385,#30386,
#30387,#30388,#30389,#30390,#30391,#30392,#30393,#30394,#30395,#30396,#30397,
#30398,#30399,#30400,#30401,#30402,#30403,#30404,#30405,#30406,#30407,#30408,
#30409,#30410,#30411,#30412,#30413,#30414,#30415,#30416,#30417,#30418,#30419,
#30420,#30421),.UNSPECIFIED.,.F.,.F.,(4,2,2,2,2,2,2,2,2,2,2,2,2,2,2,2,2,
2,2,2,2,2,2,2,2,2,2,2,2,2,2,2,2,2,2,2,2,2,2,2,2,2,2,2,2,2,2,2,2,2,2,2,2,
2,2,2,2,2,2,2,2,2,2,2,2,2,2,2,2,2,2,2,2,2,2,2,2,2,2,2,2,2,2,2,2,2,2,2,2,
2,2,2,2,2,2,2,2,2,2,2,2,2,2,2,2,2,2,2,2,2,2,2,2,2,2,2,2,2,2,2,2,2,2,2,2,
2,2,2,2,2,2,2,2,2,2,2,2,2,2,2,2,2,2,2,2,2,2,2,2,2,2,2,2,2,2,2,2,2,2,2,2,
2,2,2,2,2,2,2,2,2,2,2,2,4),(-4.27099291113195,-4.266464075548,-4.25846610092608,
-4.22284627987283,-4.14635119199378,-4.12647918566429,-4.1156252107863,
-4.1062249692604,-4.09442948881289,-4.06926244810299,-3.99011528523554,
-3.96830854467324,-3.95346837490451,-3.94670007660745,-3.94138754650563,
-3.93453804617796,-3.91922072323176,-3.83584698203982,-3.79806031281057,
-3.78460172090393,-3.77498736201644,-3.7649133777217,-3.7490002974327,-3.66762253793479,
-3.62340905519277,-3.61407699980543,-3.60838289395051,-3.60273079761969,
-3.59359710676578,-3.55710914958582,-3.49504748197602,-3.46123755733844,
-3.44822066030172,-3.43867653977123,-3.42845412352372,-3.41179586747999,
-3.34021578835372,-3.30450202143598,-3.29041457656111,-3.27959073875487,
-3.27358360377101,-3.26819858381542,-3.26146880012321,-3.24340801540968,
-3.16369703152365,-3.12642415779366,-3.11301856627768,-3.10341281972251,
-3.09332229619814,-3.07732659932846,-3.00017490859292,-2.95592437902261,
-2.94434122084579,-2.93817978999186,-2.93278823333152,-2.92627709777846,
-2.91016961746748,-2.82829614018731,-2.79071216369558,-2.77727426492673,
-2.76766321536158,-2.75758269966035,-2.74163727572168,-2.65447839340239,
-2.61568461334936,-2.60655987211153,-2.6009094857119,-2.5952131896192,-2.58587111963385,
-2.54248341076492,-2.48584218022855,-2.45347152157958,-2.44063196235395,
-2.43111386450161,-2.420822269382,-2.40381814841478,-2.33682795930802,-2.29836226612503,
-2.27701414368539,-2.26929205754578,-2.26390161694497,-2.25773650472261,
-2.24646125443373,-2.20357032769012,-2.16700473506239,-2.13606478807834,
-2.1135685383291,-2.10222937034251,-2.09284818677295,-2.08161537459901,
-2.05971027894229,-2.02994806028376,-1.99186116166522,-1.94848061949773,
-1.93718865135284,-1.93102000245057,-1.92563076012284,-1.91791598320443,
-1.89662793927592,-1.85835013282568,-1.79100066448291,-1.77401034316466,
-1.76372156539718,-1.75420267842852,-1.74135673226162,-1.7089312763956,
-1.65208699634823,-1.60903933941161,-1.59970120932987,-1.59400579612362,
-1.58835482119974,-1.57922670532033,-1.54037476529806,-1.45326322400859,
-1.43729871276704,-1.4272146040629,-1.41760598670955,-1.40418125471026,
-1.3667153212992,-1.28561399789435,-1.26891543270601,-1.2623120143564,-1.25690172972326,
-1.25080046643083,-1.23951427236896,-1.19797493461773,-1.11624440267149,
-1.10089580363026,-1.0909334432926,-1.08125090775278,-1.06739220833942,
-1.02532173857338,-0.961712205757408,-0.935704859037054,-0.927270708071229,
-0.922304264842921,-0.916601822835038,-0.907227809063822,-0.861559780905584,
-0.780832725859486,-0.765336953352046,-0.75534614776708,-0.745683764837783,
-0.731937761270912,-0.691145525187078,-0.650394722631387,-0.605678622013436,
-0.59432687984587,-0.588146235882582,-0.582761387013465,-0.575073374129285,
-0.553995070382472,-0.516359572221459,-0.448017162750547,-0.43108946189134,
-0.420814126135779,-0.411292149147035,-0.398417761941058,-0.365756510244991,
-0.31199608865096,-0.269864906689862,-0.258619690997774,-0.252461531790012,
-0.247070793091353,-0.239338863655453,-0.217901235764803,-0.179150092056855,
-0.112958905251992,-0.095720350753044,-0.0853839561810169,-0.0758848815394095,
-0.0631639249328616,-0.0421650876622171,-0.000963736707009938),
 .UNSPECIFIED.);
#1509=B_SPLINE_CURVE_WITH_KNOTS('',3,(#30423,#30424,#30425,#30426,#30427,
#30428,#30429,#30430,#30431,#30432,#30433,#30434,#30435,#30436,#30437,#30438,
#30439,#30440,#30441,#30442,#30443,#30444,#30445,#30446,#30447,#30448,#30449,
#30450,#30451,#30452,#30453,#30454,#30455,#30456,#30457,#30458,#30459,#30460,
#30461,#30462,#30463,#30464,#30465,#30466,#30467,#30468,#30469,#30470,#30471,
#30472,#30473,#30474,#30475,#30476,#30477,#30478,#30479,#30480,#30481,#30482,
#30483,#30484,#30485,#30486,#30487,#30488,#30489,#30490,#30491,#30492,#30493,
#30494,#30495,#30496,#30497,#30498,#30499,#30500,#30501,#30502,#30503,#30504,
#30505,#30506,#30507,#30508,#30509,#30510,#30511,#30512,#30513,#30514,#30515,
#30516,#30517,#30518,#30519,#30520,#30521,#30522,#30523,#30524,#30525,#30526,
#30527,#30528,#30529,#30530,#30531,#30532,#30533,#30534,#30535,#30536,#30537,
#30538,#30539,#30540,#30541,#30542,#30543,#30544,#30545,#30546,#30547,#30548,
#30549,#30550,#30551,#30552,#30553,#30554,#30555,#30556,#30557,#30558,#30559,
#30560,#30561,#30562,#30563,#30564,#30565,#30566,#30567,#30568,#30569,#30570,
#30571,#30572,#30573,#30574,#30575,#30576,#30577,#30578,#30579,#30580,#30581,
#30582,#30583,#30584,#30585,#30586,#30587,#30588,#30589,#30590,#30591,#30592,
#30593,#30594,#30595,#30596,#30597,#30598,#30599,#30600,#30601,#30602,#30603,
#30604,#30605,#30606,#30607,#30608,#30609,#30610,#30611,#30612,#30613,#30614,
#30615,#30616,#30617,#30618,#30619,#30620,#30621,#30622,#30623,#30624,#30625,
#30626,#30627,#30628,#30629,#30630,#30631,#30632,#30633),.UNSPECIFIED.,
 .F.,.F.,(4,3,3,3,3,3,3,3,3,3,3,3,3,3,3,3,3,3,3,3,3,3,3,3,3,3,3,3,3,3,3,
3,3,3,3,3,3,3,3,3,3,3,3,3,3,3,3,3,3,3,3,3,3,3,3,3,3,3,3,3,3,3,3,3,3,3,3,
3,3,3,4),(-10.1336107521151,-10.017486513996,-9.89908884700098,-9.88098295102664,
-9.78894122224417,-9.69701994766574,-9.60519272248596,-9.51343026067752,
-9.42170138808768,-9.32998237581279,-9.23824950910818,-9.14642186088112,
-9.05454468136134,-8.96251924502228,-8.89288465592398,-8.80084066000415,
-8.70891707457303,-8.61708749846466,-8.52532263580296,-8.43359133268255,
-8.34186986332005,-8.25013451607053,-8.15830436661682,-8.06642467072822,
-7.97439671930638,-7.90478636082131,-7.81276140508728,-7.72085691549409,
-7.6290464653389,-7.53730069544524,-7.44558845793987,-7.35388600441363,
-7.26216960055253,-7.17035816644906,-7.07849708693619,-6.98648740025403,
-6.91668806571865,-6.82463070078096,-6.73269385008227,-6.64085112820093,
-6.54907335094584,-6.45732927942366,-6.36559520220907,-6.27384742214499,
-6.18200518523899,-6.09011357583558,-5.99807411505652,-5.92858977061598,
-5.83652902859249,-5.74458848180794,-5.6527417543435,-5.56095952832278,
-5.46921073849288,-5.37747168097957,-5.28571866596906,-5.19387083580786,
-5.10197342617237,-5.00992788930343,-4.94049147551332,-4.84856262580369,
-4.75675446703766,-4.66504044681348,-4.57339086587097,-4.4817746379953,
-4.39016790339688,-4.29854681612798,-4.20682949572377,-4.11506200406451,
-4.02314408866267,-3.95239318041066,-3.85042544513253),.UNSPECIFIED.);
#1510=B_SPLINE_CURVE_WITH_KNOTS('',3,(#30635,#30636,#30637,#30638,#30639,
#30640,#30641,#30642,#30643,#30644,#30645,#30646,#30647,#30648,#30649,#30650,
#30651,#30652,#30653,#30654,#30655,#30656,#30657,#30658,#30659,#30660,#30661,
#30662,#30663,#30664,#30665,#30666,#30667,#30668,#30669,#30670,#30671,#30672,
#30673,#30674,#30675,#30676,#30677,#30678,#30679,#30680,#30681,#30682,#30683,
#30684,#30685,#30686,#30687,#30688,#30689,#30690,#30691,#30692,#30693,#30694,
#30695,#30696,#30697,#30698,#30699,#30700,#30701,#30702,#30703,#30704,#30705,
#30706,#30707,#30708,#30709,#30710,#30711,#30712,#30713,#30714,#30715,#30716,
#30717,#30718,#30719,#30720,#30721,#30722,#30723,#30724,#30725,#30726,#30727,
#30728,#30729,#30730,#30731,#30732,#30733,#30734,#30735,#30736,#30737,#30738,
#30739,#30740,#30741,#30742,#30743,#30744,#30745,#30746,#30747,#30748,#30749,
#30750,#30751,#30752,#30753,#30754,#30755,#30756,#30757,#30758,#30759,#30760,
#30761,#30762,#30763,#30764),.UNSPECIFIED.,.F.,.F.,(4,3,3,3,3,3,3,3,3,3,
3,3,3,3,3,3,3,3,3,3,3,3,3,3,3,3,3,3,3,3,3,3,3,3,3,3,3,3,3,3,3,3,3,4),(-3.85042544488316,
-3.75945190295832,-3.66858690682526,-3.5778051867396,-3.48706798717163,
-3.39635049713639,-3.30562792853275,-3.21482096840684,-3.12397023871895,
-3.03297757043926,-2.96429488530799,-2.87216006434223,-2.78014388468642,
-2.68822009607798,-2.59635901488637,-2.50453030368522,-2.41271036638796,
-2.32087562022036,-2.22894526869475,-2.13696478019728,-2.04483612179992,
-1.97619659020533,-1.88505763453743,-1.79403955625527,-1.70311489517017,
-1.61225058727509,-1.52141701981664,-1.43058953389116,-1.33974348102385,
-1.24878999878472,-1.15778146793944,-1.06660647517532,-0.988098295102664,
-0.893598760241011,-0.799235993918247,-0.704988418491972,-0.610850401373128,
-0.516776419061244,-0.422747137412085,-0.328743266848281,-0.234720546922284,
-0.140689749940641,-0.0465973135355168,0.),.UNSPECIFIED.);
#1511=B_SPLINE_CURVE_WITH_KNOTS('',3,(#30768,#30769,#30770,#30771,#30772,
#30773,#30774,#30775,#30776,#30777,#30778,#30779,#30780,#30781,#30782,#30783,
#30784,#30785,#30786,#30787,#30788,#30789,#30790,#30791,#30792,#30793,#30794,
#30795,#30796,#30797,#30798,#30799,#30800,#30801,#30802,#30803,#30804,#30805,
#30806,#30807,#30808,#30809,#30810,#30811,#30812,#30813,#30814,#30815,#30816,
#30817,#30818,#30819,#30820,#30821,#30822,#30823,#30824,#30825,#30826,#30827,
#30828,#30829,#30830,#30831,#30832,#30833,#30834,#30835,#30836,#30837,#30838,
#30839,#30840,#30841,#30842,#30843,#30844,#30845,#30846,#30847,#30848,#30849,
#30850,#30851,#30852,#30853,#30854,#30855,#30856,#30857,#30858,#30859,#30860,
#30861,#30862,#30863,#30864,#30865,#30866,#30867,#30868,#30869,#30870,#30871,
#30872,#30873,#30874,#30875,#30876,#30877,#30878,#30879,#30880,#30881,#30882,
#30883,#30884,#30885,#30886,#30887,#30888,#30889,#30890,#30891,#30892,#30893,
#30894,#30895,#30896,#30897,#30898,#30899,#30900,#30901,#30902,#30903,#30904,
#30905,#30906,#30907,#30908,#30909,#30910,#30911,#30912,#30913,#30914,#30915,
#30916,#30917,#30918,#30919,#30920,#30921,#30922,#30923,#30924,#30925,#30926,
#30927,#30928,#30929,#30930,#30931,#30932,#30933,#30934,#30935,#30936,#30937,
#30938,#30939,#30940,#30941,#30942,#30943,#30944,#30945,#30946,#30947,#30948,
#30949,#30950,#30951,#30952,#30953,#30954,#30955,#30956,#30957),
 .UNSPECIFIED.,.F.,.F.,(4,3,3,3,3,3,3,3,3,3,3,3,3,3,3,3,3,3,3,3,3,3,3,3,
3,3,3,3,3,3,3,3,3,3,3,3,3,3,3,3,3,3,3,3,3,3,3,3,3,3,3,3,3,3,3,3,3,3,3,3,
3,3,3,4),(2.01768719304049,2.10919291876739,2.20058006524129,2.29604441774963,
2.38727725380577,2.47848107942686,2.56968021481692,2.66089897020055,2.75221272523854,
2.84358238516307,2.93508590684933,2.96429488530799,3.0564803252153,3.14854810958801,
3.24052442375695,3.33243923003933,3.42432238696052,3.51619743540617,3.6080879034695,
3.70007461531119,3.79211190089602,3.88429752531008,3.95239318041065,4.04432800087469,
4.13614097705616,4.22785866602567,4.31951017706319,4.41112726861152,4.5027338011772,
4.59435362057034,4.6860680271731,4.77783168822558,4.8697443072756,4.94049147551332,
5.03255291168521,5.12449399472506,5.21634110133997,5.30812346936105,5.39987225566984,
5.49161116437988,5.5833638854286,5.67521119852403,5.76710796646895,5.85915266427401,
5.92858977061598,6.02064516556175,6.11258043755713,6.20442197039764,6.29619914784264,
6.38794298120279,6.47967718160351,6.57142544618978,6.66326872452,6.75516168605004,
6.84720299360337,6.91668806571864,7.00839095829693,7.09997843134294,7.19147474290257,
7.28290406726057,7.37430063642504,7.46567838122102,7.55708352464962,7.59202292841098),
 .UNSPECIFIED.);
#1512=B_SPLINE_CURVE_WITH_KNOTS('',3,(#30959,#30960,#30961,#30962,#30963,
#30964,#30965,#30966,#30967,#30968,#30969),.UNSPECIFIED.,.F.,.F.,(4,1,1,
1,1,1,1,1,4),(7.59202890078445,7.9047863608213,8.89288465592397,9.88098295102663,
10.8690812461293,11.857179541232,12.8452778363346,13.8333761314373,13.8752082355906),
 .UNSPECIFIED.);
#1513=B_SPLINE_CURVE_WITH_KNOTS('',3,(#30971,#30972,#30973,#30974,#30975,
#30976,#30977,#30978,#30979,#30980,#30981,#30982,#30983,#30984,#30985,#30986,
#30987,#30988,#30989,#30990,#30991,#30992,#30993,#30994,#30995,#30996,#30997,
#30998,#30999,#31000,#31001,#31002,#31003,#31004,#31005,#31006,#31007,#31008,
#31009,#31010,#31011,#31012,#31013,#31014,#31015,#31016,#31017,#31018,#31019,
#31020,#31021,#31022,#31023,#31024,#31025,#31026,#31027,#31028,#31029,#31030,
#31031,#31032,#31033,#31034,#31035,#31036,#31037,#31038,#31039,#31040,#31041,
#31042,#31043,#31044,#31045,#31046,#31047,#31048,#31049,#31050,#31051,#31052,
#31053,#31054,#31055,#31056,#31057,#31058,#31059,#31060,#31061,#31062,#31063,
#31064,#31065,#31066,#31067,#31068,#31069,#31070,#31071,#31072,#31073,#31074,
#31075,#31076,#31077,#31078,#31079,#31080,#31081,#31082,#31083,#31084,#31085,
#31086,#31087,#31088,#31089,#31090,#31091,#31092,#31093,#31094,#31095,#31096,
#31097,#31098,#31099,#31100,#31101,#31102,#31103,#31104,#31105,#31106,#31107,
#31108,#31109,#31110,#31111,#31112,#31113,#31114,#31115,#31116,#31117,#31118,
#31119,#31120,#31121,#31122,#31123,#31124,#31125,#31126,#31127,#31128,#31129,
#31130,#31131,#31132,#31133,#31134,#31135,#31136,#31137,#31138,#31139,#31140,
#31141,#31142,#31143,#31144,#31145,#31146,#31147,#31148,#31149,#31150,#31151,
#31152,#31153,#31154,#31155,#31156,#31157,#31158,#31159,#31160,#31161,#31162,
#31163,#31164,#31165,#31166,#31167,#31168,#31169,#31170,#31171,#31172,#31173,
#31174,#31175,#31176,#31177,#31178,#31179,#31180,#31181,#31182,#31183,#31184,
#31185,#31186,#31187,#31188,#31189,#31190,#31191,#31192,#31193,#31194,#31195,
#31196,#31197,#31198,#31199,#31200,#31201,#31202,#31203,#31204,#31205,#31206,
#31207,#31208,#31209,#31210,#31211,#31212,#31213,#31214,#31215,#31216,#31217,
#31218,#31219,#31220,#31221,#31222,#31223,#31224,#31225,#31226,#31227,#31228,
#31229,#31230,#31231,#31232,#31233,#31234,#31235,#31236,#31237,#31238,#31239,
#31240,#31241,#31242,#31243,#31244,#31245,#31246,#31247,#31248,#31249,#31250,
#31251,#31252,#31253,#31254,#31255,#31256,#31257,#31258,#31259,#31260,#31261,
#31262,#31263,#31264,#31265,#31266,#31267,#31268,#31269,#31270,#31271,#31272,
#31273,#31274,#31275,#31276,#31277,#31278,#31279,#31280,#31281,#31282,#31283,
#31284,#31285,#31286,#31287,#31288,#31289,#31290,#31291,#31292,#31293,#31294,
#31295,#31296,#31297,#31298,#31299,#31300,#31301,#31302,#31303,#31304,#31305,
#31306,#31307,#31308,#31309,#31310,#31311,#31312),.UNSPECIFIED.,.F.,.F.,
(4,2,2,2,2,2,2,2,2,2,2,2,2,2,2,2,2,2,2,2,2,2,2,2,2,2,2,2,2,2,2,2,2,2,2,
2,2,2,2,2,2,2,2,2,2,2,2,2,2,2,2,2,2,2,2,2,2,2,2,2,2,2,2,2,2,2,2,2,2,2,2,
2,2,2,2,2,2,2,2,2,2,2,2,2,2,2,2,2,2,2,2,2,2,2,2,2,2,2,2,2,2,2,2,2,2,2,2,
2,2,2,2,2,2,2,2,2,2,2,2,2,2,2,2,2,2,2,2,2,2,2,2,2,2,2,2,2,2,2,2,2,2,2,2,
2,2,2,2,2,2,2,2,2,2,2,2,2,2,2,2,2,2,2,2,2,2,2,2,2,2,2,4),(-4.27089550160095,
-4.26517093009983,-4.18123377942425,-4.13980108553207,-4.12599656693906,
-4.11632340353083,-4.10634692432074,-4.09092671351489,-4.00973421500502,
-3.96441499067419,-3.95505115903307,-3.94935053670693,-3.94438229721522,
-3.93593906273184,-3.90983752462709,-3.84626927776244,-3.8041967477589,
-3.79033657123392,-3.78065340802285,-3.77069077844753,-3.75534238978773,
-3.67365803391384,-3.63212870657385,-3.62084368969843,-3.61474250017146,
-3.60933198563307,-3.60272781227625,-3.58602573065649,-3.5048816664091,
-3.46740131169902,-3.45397454743088,-3.44436565340207,-3.43428232848595,
-3.41832126817335,-3.34092267968528,-3.29682961633398,-3.28526354800635,
-3.27910572276471,-3.27371342578226,-3.26719761375624,-3.25105995527236,
-3.19051813212376,-3.1446368186399,-3.12453272638999,-3.11363457299039,
-3.10423849812787,-3.09250395483874,-3.06770642499166,-2.98799946304298,
-2.95592737000991,-2.94719050940168,-2.94161991935152,-2.93654941666119,
-2.92754293325874,-2.8944870210215,-2.829609429513,-2.7951264879124,-2.78202987735722,
-2.772473569767,-2.76228023253695,-2.74576771617694,-2.66525527218807,-2.62467953748322,
-2.61350269589351,-2.60742321570966,-2.60200449469963,-2.59409760503653,
-2.57287744220049,-2.51046474718343,-2.462199071591,-2.44788001265044,-2.43811287274056,
-2.42825372293763,-2.41344534966472,-2.35579901995858,-2.30724301837016,
-2.28301056581025,-2.27495728114019,-2.2695144563339,-2.26349655763637,
-2.25262026322153,-2.19237202379743,-2.13597359955294,-2.11694124915784,
-2.10614409607742,-2.09682750617894,-2.08499817093511,-2.05962298215849,
-2.02252994071289,-1.96288673037515,-1.94578058017786,-1.93911857689346,
-1.9336955680881,-1.92762955663532,-1.91651694983403,-1.87649278064731,
-1.79783370866518,-1.77995205978646,-1.7694868830076,-1.76002277520293,
-1.74757650557126,-1.71813133022915,-1.67071097035882,-1.61772008756554,
-1.60645360980525,-1.60035651507718,-1.59494524779244,-1.58708134607396,
-1.56454638328828,-1.52220498480293,-1.46078901403587,-1.4436628033303,
-1.43334763739714,-1.4238392855057,-1.41106156139208,-1.3791631951668,-1.32414037672917,
-1.28223715222047,-1.27099909595084,-1.26484220774146,-1.25945011139248,
-1.25171318800143,-1.2302420421733,-1.19138861738065,-1.1249430073584,-1.10791202952862,
-1.09761573810651,-1.08810065055242,-1.07527651756836,-1.04301705294725,
-0.986751959088537,-0.942925866470926,-0.933584792995982,-0.927889083643446,
-0.922239411376962,-0.913115784663209,-0.874345994377888,-0.787093790670101,
-0.771161480803704,-0.761084405453528,-0.751473390862406,-0.738030012317473,
-0.700375138696203,-0.617897070267363,-0.602099374380554,-0.595138008132656,
-0.589817498414164,-0.583254470744053,-0.569569680107619,-0.499819830595,
-0.448627527377693,-0.434018654330641,-0.425179199719389,-0.415543495170319,
-0.401952960884438,-0.362824529424473,-0.320821812002546,-0.275403697620598,
-0.264007693896237,-0.25781770456701,-0.252435726399069,-0.244766763022211,
-0.223838005099873,-0.186658553656164,-0.118079923396639,-0.100927462738524,
-0.0906075946626851,-0.0811018260956066,-0.0683382198453528,-0.0467905167351216,
-0.000959392972239935),.UNSPECIFIED.);
#1514=B_SPLINE_CURVE_WITH_KNOTS('',3,(#31314,#31315,#31316,#31317,#31318,
#31319,#31320,#31321,#31322,#31323,#31324,#31325,#31326,#31327,#31328,#31329,
#31330,#31331,#31332,#31333,#31334,#31335,#31336,#31337,#31338,#31339,#31340,
#31341,#31342,#31343,#31344,#31345,#31346,#31347,#31348,#31349,#31350,#31351,
#31352,#31353,#31354,#31355,#31356,#31357,#31358,#31359,#31360,#31361,#31362,
#31363,#31364,#31365,#31366,#31367,#31368,#31369,#31370,#31371,#31372,#31373,
#31374,#31375,#31376,#31377,#31378,#31379,#31380,#31381,#31382,#31383,#31384,
#31385,#31386,#31387,#31388,#31389,#31390,#31391,#31392,#31393,#31394,#31395,
#31396,#31397,#31398,#31399,#31400,#31401,#31402,#31403,#31404,#31405,#31406,
#31407,#31408,#31409,#31410,#31411,#31412,#31413,#31414,#31415,#31416,#31417,
#31418,#31419,#31420,#31421,#31422,#31423,#31424,#31425,#31426,#31427,#31428,
#31429,#31430,#31431,#31432,#31433,#31434,#31435,#31436,#31437,#31438,#31439,
#31440,#31441,#31442,#31443,#31444,#31445,#31446,#31447,#31448,#31449,#31450,
#31451,#31452,#31453,#31454,#31455,#31456,#31457,#31458,#31459,#31460,#31461,
#31462,#31463,#31464,#31465,#31466,#31467,#31468,#31469,#31470,#31471,#31472,
#31473,#31474,#31475,#31476,#31477,#31478,#31479,#31480,#31481,#31482,#31483,
#31484,#31485,#31486,#31487,#31488,#31489,#31490,#31491,#31492,#31493,#31494,
#31495,#31496,#31497,#31498,#31499,#31500,#31501,#31502,#31503,#31504,#31505,
#31506,#31507,#31508,#31509,#31510,#31511,#31512,#31513,#31514,#31515,#31516,
#31517,#31518,#31519,#31520,#31521,#31522,#31523,#31524,#31525,#31526,#31527,
#31528,#31529,#31530,#31531,#31532,#31533,#31534,#31535,#31536,#31537,#31538,
#31539,#31540,#31541,#31542,#31543,#31544,#31545,#31546,#31547,#31548,#31549,
#31550,#31551,#31552,#31553,#31554,#31555,#31556,#31557,#31558,#31559,#31560,
#31561,#31562,#31563,#31564,#31565,#31566,#31567,#31568,#31569,#31570,#31571,
#31572,#31573,#31574,#31575,#31576,#31577,#31578,#31579,#31580,#31581,#31582,
#31583,#31584,#31585,#31586,#31587,#31588,#31589,#31590,#31591,#31592,#31593,
#31594,#31595,#31596,#31597,#31598,#31599,#31600,#31601,#31602,#31603,#31604,
#31605,#31606,#31607,#31608,#31609,#31610,#31611,#31612,#31613,#31614,#31615,
#31616,#31617,#31618,#31619,#31620,#31621,#31622,#31623,#31624,#31625,#31626,
#31627,#31628,#31629,#31630,#31631,#31632,#31633,#31634,#31635,#31636,#31637,
#31638,#31639,#31640,#31641,#31642,#31643,#31644,#31645,#31646,#31647,#31648,
#31649,#31650,#31651,#31652,#31653,#31654,#31655,#31656,#31657,#31658,#31659,
#31660,#31661),.UNSPECIFIED.,.F.,.F.,(4,2,2,2,2,2,2,2,2,2,2,2,2,2,2,2,2,
2,2,2,2,2,2,2,2,2,2,2,2,2,2,2,2,2,2,2,2,2,2,2,2,2,2,2,2,2,2,2,2,2,2,2,2,
2,2,2,2,2,2,2,2,2,2,2,2,2,2,2,2,2,2,2,2,2,2,2,2,2,2,2,2,2,2,2,2,2,2,2,2,
2,2,2,2,2,2,2,2,2,2,2,2,2,2,2,2,2,2,2,2,2,2,2,2,2,2,2,2,2,2,2,2,2,2,2,2,
2,2,2,2,2,2,2,2,2,2,2,2,2,2,2,2,2,2,2,2,2,2,2,2,2,2,2,2,2,2,2,2,2,2,2,2,
2,2,2,2,2,2,2,2,2,2,2,2,4),(-4.27016132765278,-4.2112933202812,-4.20202621727073,
-4.1941439983737,-4.18872991176856,-4.18264127270548,-4.17141590587009,
-4.11595626621906,-4.07009735564466,-4.04121112713488,-4.02884459941924,
-4.01939047852455,-4.00888580743757,-3.99080278362926,-3.91246175026595,
-3.87253667468467,-3.86143619608755,-3.85537283050901,-3.84994924814343,
-3.84200841905082,-3.82052645479384,-3.74461384980817,-3.70794553426337,
-3.69460505185852,-3.68501080169383,-3.67490140660616,-3.6588067905035,
-3.57238481555369,-3.53320348741931,-3.52406179256984,-3.51840823148544,
-3.51271651486387,-3.50339420602896,-3.46168860634024,-3.42168424363258,
-3.38991116432299,-3.36700456619755,-3.3555932551898,-3.3462116208593,-3.33504805244734,
-3.31418300921281,-3.23959808303002,-3.20084933621331,-3.18988740258155,
-3.18385203640618,-3.17847855423334,-3.17179972801083,-3.15454027921675,
-3.07404034493659,-3.03665243215943,-3.02323521415283,-3.01362784597951,
-3.00354148483392,-2.98756536511546,-2.90055980055357,-2.86168713740885,
-2.85255900884707,-2.84690804108186,-2.84121277593298,-2.83187493925176,
-2.78905785216877,-2.73199844915205,-2.69951029298848,-2.68665618080192,
-2.67713625246302,-2.66685107389063,-2.64987789974936,-2.5823088934531,
-2.54421466958434,-2.5229862880412,-2.51527921356779,-2.50989108551139,
-2.503718853469,-2.49240941414251,-2.44862204888924,-2.41009652685683,-2.36652312301965,
-2.35253863718015,-2.34283295534659,-2.33290013246453,-2.31770674073402,
-2.23497999469098,-2.19065164227658,-2.18131587386556,-2.17562088259492,
-2.1706483244467,-2.1621820429767,-2.13581900001301,-2.07622559070618,-2.03160467454466,
-2.01724075066862,-2.00844146095637,-1.99876623410861,-1.98495524315478,
-1.9434547363968,-1.90177199693798,-1.85868848206746,-1.8474076777392,-1.84124133775524,
-1.83585130554631,-1.82813153975872,-1.80680383850205,-1.7684028924635,
-1.70124533199585,-1.68424494671686,-1.67395405996442,-1.66443572907638,
-1.65159442865682,-1.61920668485835,-1.56249664292403,-1.51926539518677,
-1.50992598662808,-1.50423025552043,-1.49857949384636,-1.48945247207566,
-1.45062538199959,-1.36346436946267,-1.34750959691089,-1.33742737246164,
-1.32781763989175,-1.31438646629687,-1.27685908989308,-1.19532435209695,
-1.17898205826183,-1.17243380662568,-1.16703497676674,-1.16089863805806,
-1.14943922239367,-1.10633803877844,-1.02724840718897,-1.01151465493938,
-1.00147641792631,-0.991842302640632,-0.978264214302576,-0.939271129256164,
-0.896531646657189,-0.851618226349477,-0.840254431533927,-0.834070969216295,
-0.828686668497398,-0.821003440626908,-0.79996425555181,-0.762450604030013,
-0.693891345236649,-0.676975752088803,-0.666702592654482,-0.657179400770686,
-0.644298369146377,-0.611586782263747,-0.563397731297679,-0.512409737917154,
-0.502906066999759,-0.497175980974361,-0.491557451777441,-0.482582854080362,
-0.446723656507844,-0.370051694683377,-0.346049064324514,-0.334448777622994,
-0.325061346118745,-0.314061961633378,-0.293416407200125,-0.266069109142431,
-0.225172804988896,-0.180290567047164,-0.168929076004839,-0.16274629938351,
-0.157362182986379,-0.149678652385427,-0.12863492964186,-0.0911060083721691,
-0.0216916045340881,-0.00927743633556165,-0.000959649626902801),
 .UNSPECIFIED.);
#1515=B_SPLINE_CURVE_WITH_KNOTS('',3,(#31663,#31664,#31665,#31666,#31667,
#31668,#31669,#31670,#31671,#31672,#31673,#31674,#31675,#31676,#31677,#31678,
#31679,#31680,#31681,#31682,#31683,#31684,#31685,#31686,#31687,#31688,#31689,
#31690,#31691,#31692,#31693,#31694,#31695,#31696,#31697,#31698,#31699,#31700,
#31701,#31702,#31703,#31704,#31705,#31706,#31707,#31708,#31709,#31710,#31711,
#31712,#31713,#31714,#31715,#31716,#31717,#31718,#31719,#31720,#31721,#31722,
#31723,#31724,#31725,#31726,#31727,#31728,#31729,#31730,#31731,#31732,#31733,
#31734,#31735,#31736,#31737,#31738,#31739,#31740,#31741,#31742,#31743,#31744,
#31745,#31746,#31747,#31748,#31749,#31750,#31751,#31752,#31753,#31754,#31755,
#31756,#31757,#31758,#31759,#31760,#31761,#31762,#31763,#31764,#31765,#31766,
#31767,#31768,#31769,#31770,#31771,#31772,#31773,#31774,#31775,#31776,#31777,
#31778,#31779,#31780,#31781,#31782,#31783,#31784,#31785,#31786,#31787,#31788,
#31789,#31790,#31791,#31792,#31793,#31794,#31795,#31796,#31797,#31798,#31799,
#31800,#31801,#31802,#31803,#31804,#31805,#31806,#31807,#31808,#31809,#31810,
#31811,#31812,#31813,#31814,#31815,#31816,#31817,#31818,#31819,#31820,#31821,
#31822,#31823,#31824,#31825,#31826,#31827,#31828,#31829,#31830,#31831,#31832,
#31833,#31834,#31835,#31836,#31837,#31838,#31839,#31840,#31841,#31842,#31843,
#31844,#31845,#31846,#31847,#31848,#31849,#31850,#31851,#31852,#31853,#31854,
#31855,#31856,#31857,#31858,#31859,#31860,#31861,#31862,#31863,#31864,#31865,
#31866,#31867,#31868,#31869,#31870,#31871,#31872,#31873,#31874,#31875,#31876,
#31877,#31878,#31879,#31880,#31881,#31882,#31883,#31884,#31885,#31886,#31887,
#31888,#31889,#31890,#31891,#31892,#31893,#31894,#31895,#31896,#31897,#31898,
#31899,#31900,#31901,#31902,#31903,#31904,#31905,#31906,#31907,#31908,#31909,
#31910,#31911,#31912,#31913,#31914,#31915,#31916,#31917,#31918,#31919,#31920,
#31921,#31922,#31923,#31924,#31925,#31926,#31927,#31928,#31929,#31930,#31931,
#31932,#31933,#31934,#31935,#31936,#31937,#31938,#31939,#31940,#31941,#31942,
#31943,#31944,#31945,#31946,#31947,#31948,#31949,#31950,#31951,#31952,#31953,
#31954,#31955,#31956,#31957,#31958,#31959,#31960,#31961,#31962,#31963,#31964,
#31965,#31966,#31967,#31968,#31969,#31970,#31971,#31972,#31973,#31974,#31975,
#31976,#31977,#31978,#31979,#31980,#31981,#31982,#31983,#31984,#31985,#31986,
#31987,#31988,#31989,#31990,#31991,#31992,#31993,#31994,#31995,#31996,#31997,
#31998,#31999,#32000,#32001,#32002,#32003,#32004,#32005,#32006),
 .UNSPECIFIED.,.F.,.F.,(4,2,2,2,2,2,2,2,2,2,2,2,2,2,2,2,2,2,2,2,2,2,2,2,
2,2,2,2,2,2,2,2,2,2,2,2,2,2,2,2,2,2,2,2,2,2,2,2,2,2,2,2,2,2,2,2,2,2,2,2,
2,2,2,2,2,2,2,2,2,2,2,2,2,2,2,2,2,2,2,2,2,2,2,2,2,2,2,2,2,2,2,2,2,2,2,2,
2,2,2,2,2,2,2,2,2,2,2,2,2,2,2,2,2,2,2,2,2,2,2,2,2,2,2,2,2,2,2,2,2,2,2,2,
2,2,2,2,2,2,2,2,2,2,2,2,2,2,2,2,2,2,2,2,2,2,2,2,2,2,2,2,2,2,2,2,2,2,2,2,
2,2,2,4),(-4.27067861780142,-4.26537209255245,-4.2585959461785,-4.24767254749016,
-4.2272873009378,-4.14877591485979,-4.1100152384294,-4.10089250779693,-4.09524278424705,
-4.0895465358244,-4.08020356065768,-4.03645029757843,-3.98008273700803,
-3.94779107292332,-3.93496210902089,-3.92544603102557,-3.9151511372335,
-3.8981282388189,-3.83157514788041,-3.79283220017504,-3.77139620361843,
-3.76366362016086,-3.75827192944369,-3.75211263088738,-3.74086362864568,
-3.69870262149952,-3.64491001640648,-3.612235334683,-3.59935827587587,-3.58983546157847,
-3.57956035284238,-3.56263564160191,-3.48037186337755,-3.43882949132267,
-3.42958929142758,-3.42391472987895,-3.41824391805605,-3.40902113769835,
-3.37058355451726,-3.31012289936565,-3.27671842366527,-3.26375076897159,
-3.25421423664366,-3.24397366264229,-3.2272235896755,-3.14704924538102,
-3.10657471823022,-3.09540963246718,-3.08933259788933,-3.08391304973467,
-3.07600078710977,-3.05474005296049,-2.97857787688043,-2.94186473405767,
-2.92851816702505,-2.91892189858174,-2.9088124499461,-2.89272237261806,
-2.81627597515997,-2.77158303482065,-2.75995292357337,-2.75378200331587,
-2.74839310432892,-2.74068196566705,-2.72092399617808,-2.64312888050789,
-2.60614988584254,-2.59277503994756,-2.58317420700646,-2.57307382669278,
-2.55702914255223,-2.47034221775661,-2.43129187752549,-2.42215515245212,
-2.41650215942054,-2.41150086844904,-2.40287218523823,-2.37489242807534,
-2.30542949929917,-2.26995189861576,-2.25674068927914,-2.24716603637757,
-2.23701182531611,-2.22069747797986,-2.13532446255829,-2.09574400439092,
-2.08647722656653,-2.08079654930171,-2.07512991249371,-2.06593018061556,
-2.02546182071473,-1.94127043328855,-1.92470967133765,-1.91450603838393,
-1.90495281590672,-1.89188077529545,-1.85760965269131,-1.79362825149057,
-1.75955145527578,-1.75050118153279,-1.74486632306109,-1.73915366613821,
-1.72973266242786,-1.68217952637543,-1.60420617264449,-1.58831454344002,
-1.57824527411859,-1.56862946665225,-1.55515883449638,-1.51724310429662,
-1.4328055655712,-1.41974119733246,-1.41322582650967,-1.40783379076601,
-1.40167652356429,-1.39011240187944,-1.34604199136839,-1.26851379033042,
-1.25255893715664,-1.24247659978013,-1.23286674676947,-1.21943538242946,
-1.18190618232596,-1.10034676426858,-1.08403056184597,-1.07748570490152,
-1.07208649134622,-1.06594356706457,-1.05446086523337,-1.01116088618642,
-0.932468286232639,-0.916684793513309,-0.906634391221016,-0.897001873209618,
-0.883448318572225,-0.844734783202608,-0.778217793336078,-0.751203692416926,
-0.742683469744678,-0.737701932261014,-0.73202756107304,-0.722772157987534,
-0.680725957217797,-0.60569387976744,-0.586940432742266,-0.575279095677745,
-0.565895421002981,-0.554960670205056,-0.534630646378481,-0.490184825086574,
-0.431409910496945,-0.413161728988384,-0.405684177077472,-0.400329386632062,
-0.394039913575364,-0.381802615811599,-0.365163349046766,-0.316253129528295,
-0.259091569371166,-0.244197034621773,-0.234320187011864,-0.224565361362386,
-0.210319249629481,-0.163153509877998,-0.0951768006497754,-0.0773589536685485,
-0.0706388543599413,-0.0652493634815464,-0.0592081465942081,-0.0527098387532521,
-0.0374059006265811,-0.000998075931179162),.UNSPECIFIED.);
#1516=B_SPLINE_CURVE_WITH_KNOTS('',3,(#32007,#32008,#32009,#32010,#32011,
#32012,#32013,#32014,#32015,#32016,#32017,#32018,#32019,#32020,#32021,#32022,
#32023,#32024,#32025,#32026,#32027,#32028,#32029,#32030,#32031,#32032,#32033,
#32034,#32035,#32036,#32037,#32038,#32039,#32040,#32041,#32042,#32043,#32044,
#32045,#32046,#32047,#32048,#32049,#32050,#32051,#32052,#32053,#32054,#32055,
#32056,#32057,#32058,#32059,#32060,#32061,#32062,#32063,#32064,#32065,#32066,
#32067,#32068,#32069,#32070,#32071,#32072,#32073,#32074,#32075,#32076,#32077,
#32078,#32079,#32080,#32081,#32082,#32083,#32084,#32085,#32086,#32087,#32088,
#32089,#32090,#32091,#32092,#32093,#32094,#32095,#32096,#32097,#32098,#32099,
#32100,#32101,#32102,#32103,#32104,#32105,#32106,#32107,#32108,#32109,#32110,
#32111,#32112,#32113,#32114,#32115,#32116,#32117,#32118,#32119,#32120,#32121,
#32122,#32123,#32124,#32125,#32126,#32127,#32128,#32129,#32130,#32131,#32132,
#32133,#32134,#32135,#32136,#32137,#32138,#32139,#32140,#32141,#32142,#32143,
#32144,#32145,#32146,#32147,#32148,#32149,#32150,#32151,#32152,#32153,#32154,
#32155,#32156,#32157,#32158,#32159,#32160,#32161,#32162,#32163,#32164,#32165,
#32166,#32167,#32168,#32169,#32170,#32171,#32172,#32173,#32174,#32175,#32176,
#32177,#32178,#32179,#32180,#32181,#32182,#32183,#32184,#32185,#32186,#32187,
#32188,#32189,#32190,#32191,#32192,#32193,#32194,#32195,#32196,#32197,#32198,
#32199),.UNSPECIFIED.,.F.,.F.,(4,3,3,3,3,3,3,3,3,3,3,3,3,3,3,3,3,3,3,3,
3,3,3,3,3,3,3,3,3,3,3,3,3,3,3,3,3,3,3,3,3,3,3,3,3,3,3,3,3,3,3,3,3,3,3,3,
3,3,3,3,3,3,3,3,4),(51.5743200788773,51.6649277828395,51.7554520784406,
51.8459317845929,51.9363919168048,52.026857467403,52.1174090872171,52.2080050728962,
52.298745910618,52.3692096404412,52.4611387007398,52.5529470704279,52.644661301644,
52.7363110928568,52.8279275304985,52.9195344741252,53.0111557694502,53.1028732951607,
53.1946409909151,53.2865591063539,53.3573079355438,53.4495092586262,53.5415897364067,
53.6335755674778,53.7254950911433,53.8173800174986,53.9092538900192,54.0011402370549,
54.0931182965783,54.1851443977839,54.2773148220531,54.3454062306465,54.4375405184005,
54.5295561626478,54.6214794144077,54.7133399588713,54.8051681336385,54.8969875354656,
54.9888217477981,55.0807515713472,55.1727315343686,55.2648596767482,55.3335045257492,
55.4246445692492,55.5156637380849,55.606589491441,55.6974548906982,55.7882895490156,
55.8791181244371,55.9699652645748,56.0609198246063,56.1519294300429,56.2431054808996,
56.3216028208518,56.4161015484885,56.5104635039292,56.6047102669304,56.6988474743701,
56.7929206502446,56.886949130588,56.9809522068713,57.0749741487432,57.1690041771278,
57.2630958659899,57.3097011159545),.UNSPECIFIED.);
#1517=B_SPLINE_CURVE_WITH_KNOTS('',3,(#32202,#32203,#32204,#32205,#32206,
#32207,#32208,#32209,#32210,#32211,#32212,#32213,#32214,#32215,#32216,#32217,
#32218,#32219,#32220,#32221,#32222,#32223,#32224,#32225,#32226,#32227,#32228,
#32229,#32230,#32231,#32232,#32233,#32234,#32235,#32236,#32237,#32238,#32239,
#32240,#32241,#32242,#32243,#32244,#32245,#32246,#32247,#32248,#32249,#32250,
#32251,#32252,#32253,#32254,#32255,#32256,#32257,#32258,#32259,#32260,#32261,
#32262,#32263,#32264,#32265,#32266,#32267,#32268,#32269,#32270,#32271,#32272,
#32273,#32274,#32275,#32276,#32277,#32278,#32279,#32280,#32281,#32282,#32283,
#32284,#32285,#32286,#32287,#32288,#32289,#32290,#32291,#32292,#32293,#32294,
#32295,#32296,#32297,#32298,#32299,#32300,#32301,#32302,#32303,#32304,#32305,
#32306,#32307,#32308,#32309,#32310,#32311,#32312,#32313,#32314,#32315,#32316,
#32317,#32318,#32319,#32320,#32321,#32322,#32323,#32324,#32325,#32326,#32327,
#32328,#32329,#32330,#32331,#32332,#32333,#32334,#32335,#32336,#32337,#32338,
#32339,#32340,#32341,#32342,#32343,#32344,#32345,#32346,#32347,#32348,#32349),
 .UNSPECIFIED.,.F.,.F.,(4,3,3,3,3,3,3,3,3,3,3,3,3,3,3,3,3,3,3,3,3,3,3,3,
3,3,3,3,3,3,3,3,3,3,3,3,3,3,3,3,3,3,3,3,3,3,3,3,3,4),(17.9338553089788,
18.0215439040059,18.1091610711696,18.1967367502352,18.2842926731967,18.3718494470166,
18.4594276742157,18.5470991128665,18.6348218107834,18.7226771653382,18.774225888535,
18.8620580791135,18.949779824276,19.0374141030197,19.1280278630969,19.2155641927871,
19.3030877407944,19.390619143229,19.4781790367439,19.5658354343701,19.6535494818897,
19.7413879044324,19.7623241836377,19.8501737049915,19.9379129932197,20.0255650044576,
20.1161721887429,20.2037266088798,20.2912683483248,20.3788180234578,20.4663962512482,
20.5540709827269,20.6418033849509,20.7296600546718,20.7504224787404,20.8382696052408,
20.9260065029351,21.0136561309453,21.1042642113075,21.1918162824243,21.2793556897791,
21.3669030524404,21.454478990082,21.5421514761848,21.629881656649,21.7177361559214,
21.738520773843,21.851595669962,21.9625651261396,21.991148574894),
 .UNSPECIFIED.);
#1518=B_SPLINE_CURVE_WITH_KNOTS('',3,(#32350,#32351,#32352,#32353,#32354,
#32355,#32356,#32357,#32358,#32359,#32360,#32361,#32362,#32363,#32364,#32365,
#32366,#32367,#32368,#32369,#32370,#32371,#32372,#32373,#32374,#32375,#32376,
#32377,#32378,#32379,#32380,#32381,#32382,#32383,#32384,#32385,#32386,#32387,
#32388,#32389,#32390,#32391,#32392,#32393,#32394,#32395,#32396,#32397,#32398,
#32399,#32400,#32401,#32402,#32403,#32404,#32405,#32406,#32407,#32408,#32409,
#32410,#32411,#32412,#32413,#32414,#32415,#32416,#32417,#32418,#32419,#32420,
#32421,#32422,#32423,#32424,#32425,#32426,#32427,#32428,#32429,#32430,#32431),
 .UNSPECIFIED.,.F.,.F.,(4,3,3,3,3,3,3,3,3,3,3,3,3,3,3,3,3,3,3,3,3,3,3,3,
3,3,3,4),(21.9911485751285,22.07782353564,22.1644492228726,22.2510509271146,
22.3376501732404,22.4242684800746,22.5109767570387,22.5977358546946,22.6846237111792,
22.7266190689457,22.8144654301682,22.9022015361397,22.9898503470852,23.0804587242056,
23.1680099200613,23.2555484320559,23.3430948801545,23.4306698849134,23.5183414155381,
23.6060706262079,23.6939241420068,23.7147173640484,23.8025623224055,23.8903011418041,
23.9779408712635,24.0655226220768,24.1530722511086,24.2165026702176),
 .UNSPECIFIED.);
#1519=B_SPLINE_CURVE_WITH_KNOTS('',3,(#32433,#32434,#32435,#32436,#32437,
#32438,#32439,#32440,#32441,#32442,#32443,#32444,#32445,#32446,#32447,#32448,
#32449,#32450,#32451,#32452,#32453,#32454,#32455,#32456,#32457,#32458,#32459,
#32460,#32461,#32462,#32463,#32464,#32465,#32466,#32467,#32468,#32469,#32470,
#32471,#32472,#32473,#32474,#32475,#32476,#32477,#32478,#32479,#32480,#32481,
#32482,#32483,#32484,#32485,#32486,#32487,#32488,#32489,#32490,#32491,#32492,
#32493,#32494,#32495,#32496,#32497,#32498,#32499,#32500,#32501,#32502,#32503,
#32504,#32505,#32506,#32507,#32508,#32509,#32510,#32511),.UNSPECIFIED.,
 .F.,.F.,(4,3,3,3,3,3,3,3,3,3,3,3,3,3,3,3,3,3,3,3,3,3,3,3,3,3,4),(21.9911485753101,
22.0943756280195,22.1991438177791,22.3039120075388,22.3917615121359,22.4795007834467,
22.5671527776282,22.6577599682548,22.745314371099,22.832856093194,22.9204057509385,
23.0079839613211,23.09565867545,23.1833910603384,23.2712477128744,23.2920103026415,
23.3798611821018,23.46760091707,23.5552524705408,23.6428372873228,23.7303867997398,
23.8179216416748,23.9054624312907,23.9930721519065,24.0807198637846,24.168477835605,
24.2162169687424),.UNSPECIFIED.);
#1520=B_SPLINE_CURVE_WITH_KNOTS('',3,(#32512,#32513,#32514,#32515,#32516,
#32517,#32518,#32519,#32520,#32521,#32522,#32523,#32524,#32525,#32526,#32527,
#32528,#32529,#32530,#32531,#32532,#32533,#32534,#32535,#32536,#32537,#32538,
#32539,#32540,#32541,#32542,#32543,#32544,#32545,#32546,#32547,#32548,#32549,
#32550,#32551,#32552,#32553,#32554,#32555,#32556,#32557,#32558,#32559,#32560,
#32561,#32562,#32563,#32564,#32565,#32566,#32567,#32568,#32569,#32570,#32571,
#32572,#32573,#32574,#32575,#32576,#32577,#32578,#32579,#32580,#32581,#32582,
#32583,#32584,#32585,#32586,#32587,#32588,#32589,#32590,#32591,#32592,#32593,
#32594,#32595,#32596,#32597,#32598,#32599,#32600,#32601,#32602,#32603,#32604,
#32605,#32606,#32607,#32608,#32609,#32610,#32611,#32612,#32613,#32614,#32615,
#32616,#32617,#32618,#32619,#32620,#32621,#32622,#32623,#32624,#32625,#32626,
#32627,#32628,#32629,#32630,#32631,#32632,#32633,#32634,#32635,#32636,#32637,
#32638,#32639,#32640,#32641,#32642,#32643,#32644,#32645,#32646,#32647,#32648,
#32649,#32650,#32651,#32652,#32653,#32654,#32655,#32656,#32657,#32658,#32659),
 .UNSPECIFIED.,.F.,.F.,(4,3,3,3,3,3,3,3,3,3,3,3,3,3,3,3,3,3,3,3,3,3,3,3,
3,3,3,3,3,3,3,3,3,3,3,3,3,3,3,3,3,3,3,3,3,3,3,3,3,4),(17.9330836177785,
18.0207920357673,18.1085927320213,18.1964419063721,18.2844284749951,18.3515188271282,
18.4392641415273,18.5268979148076,18.6144432387119,18.7050899741517,18.7925354599518,
18.8799676203594,18.9674071884555,19.0548748976097,19.1424390496895,19.2300607078759,
19.3178072255313,19.3396171222308,19.4274832824099,19.5152392634936,19.6029080003411,
19.6935089274652,19.7810800438035,19.8686384385576,19.9562047092435,20.0437994539135,
20.1314905019181,20.2192391220966,20.3071117434506,20.3277154173335,20.4155758115876,
20.503326236269,20.5909896323957,20.6815926424008,20.7691589952233,20.8567128499074,
20.9442748102051,21.0318654805741,21.1195528264309,21.2072979580046,21.2951674297034,
21.3158137124362,21.4033376679948,21.4907559825063,21.5780897484102,21.6653599877815,
21.7525970742007,21.8398129836218,21.9270557282901,21.9911485751285),
 .UNSPECIFIED.);
#1521=B_SPLINE_CURVE_WITH_KNOTS('',3,(#32904,#32905,#32906,#32907,#32908,
#32909,#32910,#32911,#32912,#32913,#32914,#32915,#32916,#32917,#32918,#32919,
#32920,#32921,#32922,#32923,#32924,#32925,#32926,#32927,#32928,#32929,#32930,
#32931,#32932,#32933,#32934,#32935,#32936,#32937,#32938,#32939,#32940,#32941,
#32942,#32943,#32944,#32945,#32946,#32947,#32948,#32949,#32950,#32951,#32952,
#32953,#32954,#32955,#32956,#32957,#32958,#32959,#32960,#32961,#32962,#32963,
#32964,#32965,#32966,#32967,#32968,#32969,#32970,#32971,#32972,#32973,#32974,
#32975,#32976,#32977,#32978,#32979,#32980,#32981,#32982,#32983,#32984,#32985,
#32986,#32987,#32988,#32989,#32990,#32991,#32992,#32993,#32994,#32995,#32996,
#32997,#32998,#32999,#33000),.UNSPECIFIED.,.F.,.F.,(4,3,3,3,3,3,3,3,3,3,
3,3,3,3,3,3,3,3,3,3,3,3,3,3,3,3,3,3,3,3,3,3,4),(0.,0.0371582535577247,0.0748617881856257,
0.112715125949566,0.148381967323058,0.15512741629588,0.16010500092411,0.197066207831433,
0.233851108508262,0.269797208916457,0.300074600064785,0.306206454212408,
0.31126514519064,0.346541882858749,0.381619422387025,0.389927986336217,
0.425938753218444,0.446125992369769,0.452219114700122,0.457530832114577,
0.49237174121568,0.527498764190727,0.562156271439185,0.587436666429045,
0.594976497048954,0.600634884631193,0.63468210758544,0.667951164906714,
0.675839565696752,0.683329187302406,0.715805593816627,0.746543832162165,
0.76075981699454),.UNSPECIFIED.);
#1522=B_SPLINE_CURVE_WITH_KNOTS('',3,(#33001,#33002,#33003,#33004,#33005,
#33006,#33007,#33008,#33009,#33010,#33011,#33012,#33013,#33014,#33015,#33016,
#33017,#33018,#33019,#33020,#33021,#33022,#33023,#33024,#33025,#33026,#33027,
#33028,#33029,#33030,#33031,#33032,#33033,#33034,#33035,#33036,#33037,#33038,
#33039,#33040,#33041,#33042,#33043,#33044,#33045,#33046,#33047,#33048,#33049,
#33050,#33051,#33052,#33053,#33054,#33055,#33056,#33057,#33058,#33059,#33060,
#33061,#33062,#33063,#33064,#33065,#33066,#33067,#33068,#33069,#33070,#33071,
#33072,#33073,#33074,#33075,#33076,#33077,#33078,#33079,#33080,#33081,#33082,
#33083,#33084,#33085,#33086,#33087,#33088,#33089,#33090,#33091),
 .UNSPECIFIED.,.F.,.F.,(4,3,3,3,3,3,3,3,3,3,3,3,3,3,3,3,3,3,3,3,3,3,3,3,
3,3,3,3,3,3,4),(0.,0.0323971454667795,0.0650536488164166,0.0985250267045374,
0.129588581867118,0.13467228593443,0.168838432673145,0.203443204976229,
0.238107726142545,0.26707589046058,0.272862060653106,0.277501012548678,
0.313123984749285,0.348617864081868,0.35417215967219,0.388993021314974,
0.410899893444863,0.417113525277951,0.422029119319603,0.457837540262106,
0.49387383576635,0.530488931026721,0.565262803089615,0.571306516388801,
0.608618623127816,0.645997594535657,0.655870746107889,0.662594569309399,
0.701717300056918,0.740840030804437,0.757688813005636),.UNSPECIFIED.);
#1523=B_SPLINE_CURVE_WITH_KNOTS('',3,(#33336,#33337,#33338,#33339,#33340,
#33341,#33342,#33343,#33344,#33345,#33346,#33347,#33348,#33349,#33350,#33351,
#33352,#33353,#33354,#33355,#33356,#33357,#33358,#33359,#33360,#33361,#33362,
#33363,#33364,#33365,#33366,#33367,#33368,#33369,#33370,#33371,#33372,#33373,
#33374,#33375,#33376,#33377,#33378,#33379,#33380,#33381,#33382,#33383,#33384,
#33385,#33386,#33387,#33388,#33389,#33390,#33391,#33392,#33393,#33394,#33395,
#33396,#33397,#33398,#33399,#33400,#33401,#33402,#33403,#33404,#33405,#33406,
#33407,#33408,#33409,#33410,#33411,#33412,#33413,#33414,#33415,#33416,#33417,
#33418,#33419,#33420,#33421,#33422,#33423,#33424,#33425,#33426,#33427,#33428,
#33429),.UNSPECIFIED.,.F.,.F.,(4,3,3,3,3,3,3,3,3,3,3,3,3,3,3,3,3,3,3,3,
3,3,3,3,3,3,3,3,3,3,3,4),(0.,0.0323971106182625,0.0650535600024233,0.0985249065560379,
0.12958844247305,0.134672211515514,0.168838316865248,0.20344306680887,0.23810760081696,
0.267075785377979,0.272860859709737,0.277498564566242,0.313121517298547,
0.348615432551105,0.354172159672169,0.388993050154282,0.41089992209137,
0.417113614967599,0.422029263005729,0.457357723104148,0.493337814845609,
0.529931916187903,0.556146362990719,0.565213636980827,0.571306505714019,
0.608618620517587,0.645997591303791,0.6558707597048,0.662594586404321,0.70171730860435,
0.74084003080438,0.757688816127246),.UNSPECIFIED.);
#1524=B_SPLINE_CURVE_WITH_KNOTS('',3,(#33430,#33431,#33432,#33433,#33434,
#33435,#33436,#33437,#33438,#33439,#33440,#33441,#33442,#33443,#33444,#33445,
#33446,#33447,#33448,#33449,#33450,#33451,#33452,#33453,#33454,#33455,#33456,
#33457,#33458,#33459,#33460,#33461,#33462,#33463,#33464,#33465,#33466,#33467,
#33468,#33469,#33470,#33471,#33472,#33473,#33474,#33475,#33476,#33477,#33478,
#33479,#33480,#33481,#33482,#33483,#33484,#33485,#33486,#33487,#33488,#33489,
#33490,#33491,#33492,#33493,#33494,#33495,#33496,#33497,#33498,#33499,#33500,
#33501,#33502,#33503,#33504,#33505,#33506,#33507,#33508,#33509,#33510,#33511,
#33512,#33513,#33514,#33515,#33516,#33517,#33518,#33519,#33520,#33521,#33522,
#33523),.UNSPECIFIED.,.F.,.F.,(4,3,3,3,3,3,3,3,3,3,3,3,3,3,3,3,3,3,3,3,
3,3,3,3,3,3,3,3,3,3,3,4),(3.15881253341124E-15,0.037509298934911,0.0752806849453368,
0.113182237345987,0.136543756612647,0.150023018727175,0.156484526466218,
0.162775149619923,0.199734977082873,0.236494912447612,0.272408734754427,
0.300074391479266,0.306205590700807,0.311264773878789,0.346804545360892,
0.381619091867029,0.38992798633622,0.425957306860802,0.454093087159789,
0.459010598705686,0.494000696219774,0.529122663331113,0.563682436557196,
0.594976556680381,0.600634899827219,0.634691065010384,0.662654256798317,
0.675839591841063,0.684660531999309,0.717119975802094,0.746543832162118,
0.760759816994502),.UNSPECIFIED.);
#1525=B_SPLINE_CURVE_WITH_KNOTS('',3,(#33535,#33536,#33537,#33538,#33539,
#33540,#33541,#33542),.UNSPECIFIED.,.F.,.F.,(4,2,2,4),(-1.55140558439687,
-1.49530246566204,-1.28032845030884,-1.06535443495564),.UNSPECIFIED.);
#1526=B_SPLINE_CURVE_WITH_KNOTS('',3,(#33544,#33545,#33546,#33547,#33548,
#33549,#33550,#33551,#33552,#33553),.UNSPECIFIED.,.F.,.F.,(4,2,2,2,4),(0.479243585826225,
0.566096001425061,0.754791726540168,0.943487451655276,1.03033986725411),
 .UNSPECIFIED.);
#1527=B_SPLINE_CURVE_WITH_KNOTS('',3,(#33555,#33556,#33557,#33558,#33559,
#33560,#33561,#33562,#33563,#33564,#33565,#33566,#33567,#33568),
 .UNSPECIFIED.,.F.,.F.,(4,2,2,2,2,2,4),(-1.55140558439687,-1.49530246566204,
-1.28032845030884,-1.06535443495564,-0.850380419602444,-0.635406404249244,
-0.579303285514419),.UNSPECIFIED.);
#1528=B_SPLINE_CURVE_WITH_KNOTS('',3,(#33570,#33571,#33572,#33573,#33574,
#33575,#33576,#33577,#33578,#33579),.UNSPECIFIED.,.F.,.F.,(4,2,2,2,4),(1.98882703890656,
2.0756794545054,2.26437517962051,2.45307090473561,2.53992332033445),
 .UNSPECIFIED.);
#1529=B_SPLINE_CURVE_WITH_KNOTS('',3,(#33580,#33581,#33582,#33583,#33584,
#33585,#33586,#33587),.UNSPECIFIED.,.F.,.F.,(4,2,2,4),(-1.06535443495564,
-0.850380419602443,-0.635406404249243,-0.57930328551442),.UNSPECIFIED.);
#1530=B_SPLINE_CURVE_WITH_KNOTS('',3,(#33590,#33591,#33592,#33593,#33594,
#33595,#33596,#33597,#33598,#33599,#33600,#33601,#33602,#33603,#33604,#33605,
#33606,#33607),.UNSPECIFIED.,.F.,.F.,(4,2,2,2,2,2,2,2,4),(-2.26535091124315,
-2.07657500399737,-1.88779909675158,-1.69901651879018,-1.51023394082877,
-1.32145136286736,-1.13266878490596,-0.94389287766017,-0.755116970414384),
 .UNSPECIFIED.);
#1531=B_SPLINE_CURVE_WITH_KNOTS('',3,(#33609,#33610,#33611,#33612,#33613,
#33614,#33615,#33616,#33617,#33618,#33619,#33620,#33621,#33622,#33623,#33624,
#33625,#33626,#33627),.UNSPECIFIED.,.F.,.F.,(4,2,2,2,3,2,2,2,4),(2.26535091124315,
2.45412681848894,2.64290272573473,2.83168530369613,3.02046788165754,3.20925045961894,
3.39803303758035,3.58680894482614,3.77558485207192),.UNSPECIFIED.);
#1532=B_SPLINE_CURVE_WITH_KNOTS('',3,(#33630,#33631,#33632,#33633,#33634,
#33635,#33636,#33637,#33638,#33639,#33640,#33641,#33642,#33643,#33644,#33645,
#33646,#33647,#33648,#33649,#33650,#33651,#33652,#33653,#33654,#33655,#33656,
#33657,#33658,#33659,#33660,#33661,#33662,#33663),.UNSPECIFIED.,.T.,.F.,
(4,2,2,2,2,2,2,2,2,2,2,2,2,2,2,2,4),(-3.02046788165754,-2.83168530369613,
-2.64290272573473,-2.45412681848894,-2.26535091124315,-2.07657500399737,
-1.88779909675158,-1.69901651879018,-1.51023394082877,-1.32145136286736,
-1.13266878490596,-0.943892877660171,-0.755116970414385,-0.566341063168599,
-0.377565155922813,-0.188782577961406,0.),.UNSPECIFIED.);
#1533=B_SPLINE_CURVE_WITH_KNOTS('',3,(#33667,#33668,#33669,#33670,#33671,
#33672,#33673,#33674),.UNSPECIFIED.,.F.,.F.,(4,2,2,4),(-1.55140558439687,
-1.49530246566204,-1.28032845030884,-1.06535443495564),.UNSPECIFIED.);
#1534=B_SPLINE_CURVE_WITH_KNOTS('',3,(#33676,#33677,#33678,#33679,#33680,
#33681,#33682,#33683,#33684,#33685),.UNSPECIFIED.,.F.,.F.,(4,2,2,2,4),(1.98882703890656,
2.0756794545054,2.26437517962051,2.45307090473561,2.53992332033445),
 .UNSPECIFIED.);
#1535=B_SPLINE_CURVE_WITH_KNOTS('',3,(#33687,#33688,#33689,#33690,#33691,
#33692,#33693,#33694,#33695,#33696,#33697,#33698,#33699,#33700),
 .UNSPECIFIED.,.F.,.F.,(4,2,2,2,2,2,4),(-1.55140558439687,-1.49530246566204,
-1.28032845030884,-1.06535443495564,-0.850380419602444,-0.635406404249244,
-0.57930328551442),.UNSPECIFIED.);
#1536=B_SPLINE_CURVE_WITH_KNOTS('',3,(#33702,#33703,#33704,#33705,#33706,
#33707,#33708,#33709,#33710,#33711),.UNSPECIFIED.,.F.,.F.,(4,2,2,2,4),(0.479243585826223,
0.566096001425061,0.754791726540169,0.943487451655276,1.03033986725411),
 .UNSPECIFIED.);
#1537=B_SPLINE_CURVE_WITH_KNOTS('',3,(#33712,#33713,#33714,#33715,#33716,
#33717,#33718,#33719),.UNSPECIFIED.,.F.,.F.,(4,2,2,4),(-1.06535443495564,
-0.850380419602443,-0.635406404249243,-0.57930328551442),.UNSPECIFIED.);
#1538=B_SPLINE_CURVE_WITH_KNOTS('',3,(#34265,#34266,#34267,#34268,#34269,
#34270,#34271,#34272,#34273,#34274,#34275,#34276,#34277,#34278,#34279,#34280,
#34281,#34282,#34283),.UNSPECIFIED.,.F.,.F.,(4,2,2,2,3,2,2,2,4),(2.26050146390194,
2.44886175450614,2.63722204511035,2.82556593417816,3.01390982324597,3.20225371231378,
3.39059760138159,3.5789578919858,3.76731818259),.UNSPECIFIED.);
#1539=B_SPLINE_CURVE_WITH_KNOTS('',3,(#34290,#34291,#34292,#34293,#34294,
#34295,#34296,#34297,#34298,#34299,#34300,#34301,#34302,#34303,#34304,#34305,
#34306,#34307,#34308),.UNSPECIFIED.,.F.,.F.,(4,2,2,2,3,2,2,2,4),(2.26051113353486,
2.44887185347984,2.63723257342483,2.82557647618218,3.01392037893953,3.20226428169689,
3.39060818445424,3.57896890439922,3.76732962434421),.UNSPECIFIED.);
#1540=VERTEX_POINT('',#6191);
#1541=VERTEX_POINT('',#6192);
#1542=VERTEX_POINT('',#6229);
#1543=VERTEX_POINT('',#6231);
#1544=VERTEX_POINT('',#6269);
#1545=VERTEX_POINT('',#6270);
#1546=VERTEX_POINT('',#6307);
#1547=VERTEX_POINT('',#6309);
#1548=VERTEX_POINT('',#6347);
#1549=VERTEX_POINT('',#6349);
#1550=VERTEX_POINT('',#6351);
#1551=VERTEX_POINT('',#6355);
#1552=VERTEX_POINT('',#6358);
#1553=VERTEX_POINT('',#6359);
#1554=VERTEX_POINT('',#6364);
#1555=VERTEX_POINT('',#6366);
#1556=VERTEX_POINT('',#6370);
#1557=VERTEX_POINT('',#6372);
#1558=VERTEX_POINT('',#6376);
#1559=VERTEX_POINT('',#6380);
#1560=VERTEX_POINT('',#6386);
#1561=VERTEX_POINT('',#6388);
#1562=VERTEX_POINT('',#6395);
#1563=VERTEX_POINT('',#6397);
#1564=VERTEX_POINT('',#6401);
#1565=VERTEX_POINT('',#6403);
#1566=VERTEX_POINT('',#6410);
#1567=VERTEX_POINT('',#6411);
#1568=VERTEX_POINT('',#6413);
#1569=VERTEX_POINT('',#6418);
#1570=VERTEX_POINT('',#6476);
#1571=VERTEX_POINT('',#6477);
#1572=VERTEX_POINT('',#6479);
#1573=VERTEX_POINT('',#6681);
#1574=VERTEX_POINT('',#6910);
#1575=VERTEX_POINT('',#6911);
#1576=VERTEX_POINT('',#6913);
#1577=VERTEX_POINT('',#7144);
#1578=VERTEX_POINT('',#7379);
#1579=VERTEX_POINT('',#7380);
#1580=VERTEX_POINT('',#7382);
#1581=VERTEX_POINT('',#7613);
#1582=VERTEX_POINT('',#7845);
#1583=VERTEX_POINT('',#7846);
#1584=VERTEX_POINT('',#7848);
#1585=VERTEX_POINT('',#8082);
#1586=VERTEX_POINT('',#8317);
#1587=VERTEX_POINT('',#8318);
#1588=VERTEX_POINT('',#8320);
#1589=VERTEX_POINT('',#8548);
#1590=VERTEX_POINT('',#8780);
#1591=VERTEX_POINT('',#8781);
#1592=VERTEX_POINT('',#8783);
#1593=VERTEX_POINT('',#9017);
#1594=VERTEX_POINT('',#9246);
#1595=VERTEX_POINT('',#9247);
#1596=VERTEX_POINT('',#9249);
#1597=VERTEX_POINT('',#9284);
#1598=VERTEX_POINT('',#9292);
#1599=VERTEX_POINT('',#9294);
#1600=VERTEX_POINT('',#9487);
#1601=VERTEX_POINT('',#9488);
#1602=VERTEX_POINT('',#9490);
#1603=VERTEX_POINT('',#9495);
#1604=VERTEX_POINT('',#9647);
#1605=VERTEX_POINT('',#9649);
#1606=VERTEX_POINT('',#9863);
#1607=VERTEX_POINT('',#9864);
#1608=VERTEX_POINT('',#9866);
#1609=VERTEX_POINT('',#9881);
#1610=VERTEX_POINT('',#10098);
#1611=VERTEX_POINT('',#10099);
#1612=VERTEX_POINT('',#10101);
#1613=VERTEX_POINT('',#10317);
#1614=VERTEX_POINT('',#10534);
#1615=VERTEX_POINT('',#10535);
#1616=VERTEX_POINT('',#10709);
#1617=VERTEX_POINT('',#10926);
#1618=VERTEX_POINT('',#10927);
#1619=VERTEX_POINT('',#10929);
#1620=VERTEX_POINT('',#11106);
#1621=VERTEX_POINT('',#11323);
#1622=VERTEX_POINT('',#11324);
#1623=VERTEX_POINT('',#11486);
#1624=VERTEX_POINT('',#11703);
#1625=VERTEX_POINT('',#11704);
#1626=VERTEX_POINT('',#11706);
#1627=VERTEX_POINT('',#11877);
#1628=VERTEX_POINT('',#11893);
#1629=VERTEX_POINT('',#11895);
#1630=VERTEX_POINT('',#11897);
#1631=VERTEX_POINT('',#11899);
#1632=VERTEX_POINT('',#11942);
#1633=VERTEX_POINT('',#11944);
#1634=VERTEX_POINT('',#12131);
#1635=VERTEX_POINT('',#12345);
#1636=VERTEX_POINT('',#12576);
#1637=VERTEX_POINT('',#13630);
#1638=VERTEX_POINT('',#13632);
#1639=VERTEX_POINT('',#13636);
#1640=VERTEX_POINT('',#13639);
#1641=VERTEX_POINT('',#13646);
#1642=VERTEX_POINT('',#13647);
#1643=VERTEX_POINT('',#13649);
#1644=VERTEX_POINT('',#13760);
#1645=VERTEX_POINT('',#13845);
#1646=VERTEX_POINT('',#13846);
#1647=VERTEX_POINT('',#14167);
#1648=VERTEX_POINT('',#14168);
#1649=VERTEX_POINT('',#14489);
#1650=VERTEX_POINT('',#14490);
#1651=VERTEX_POINT('',#14815);
#1652=VERTEX_POINT('',#14816);
#1653=VERTEX_POINT('',#15135);
#1654=VERTEX_POINT('',#15136);
#1655=VERTEX_POINT('',#15457);
#1656=VERTEX_POINT('',#15458);
#1657=VERTEX_POINT('',#15465);
#1658=VERTEX_POINT('',#15467);
#1659=VERTEX_POINT('',#15473);
#1660=VERTEX_POINT('',#15688);
#1661=VERTEX_POINT('',#15903);
#1662=VERTEX_POINT('',#16115);
#1663=VERTEX_POINT('',#16126);
#1664=VERTEX_POINT('',#16338);
#1665=VERTEX_POINT('',#16553);
#1666=VERTEX_POINT('',#16603);
#1667=VERTEX_POINT('',#16605);
#1668=VERTEX_POINT('',#16610);
#1669=VERTEX_POINT('',#16828);
#1670=VERTEX_POINT('',#17040);
#1671=VERTEX_POINT('',#17255);
#1672=VERTEX_POINT('',#17470);
#1673=VERTEX_POINT('',#17900);
#1674=VERTEX_POINT('',#18037);
#1675=VERTEX_POINT('',#18190);
#1676=VERTEX_POINT('',#18191);
#1677=VERTEX_POINT('',#18206);
#1678=VERTEX_POINT('',#18216);
#1679=VERTEX_POINT('',#18233);
#1680=VERTEX_POINT('',#18235);
#1681=VERTEX_POINT('',#18239);
#1682=VERTEX_POINT('',#18240);
#1683=VERTEX_POINT('',#18290);
#1684=VERTEX_POINT('',#18299);
#1685=VERTEX_POINT('',#18306);
#1686=VERTEX_POINT('',#18357);
#1687=VERTEX_POINT('',#18410);
#1688=VERTEX_POINT('',#18425);
#1689=VERTEX_POINT('',#18713);
#1690=VERTEX_POINT('',#18993);
#1691=VERTEX_POINT('',#19193);
#1692=VERTEX_POINT('',#19194);
#1693=VERTEX_POINT('',#19196);
#1694=VERTEX_POINT('',#19275);
#1695=VERTEX_POINT('',#19336);
#1696=VERTEX_POINT('',#19337);
#1697=VERTEX_POINT('',#19507);
#1698=VERTEX_POINT('',#19564);
#1699=VERTEX_POINT('',#19565);
#1700=VERTEX_POINT('',#19567);
#1701=VERTEX_POINT('',#19734);
#1702=VERTEX_POINT('',#19865);
#1703=VERTEX_POINT('',#19866);
#1704=VERTEX_POINT('',#20211);
#1705=VERTEX_POINT('',#20212);
#1706=VERTEX_POINT('',#20214);
#1707=VERTEX_POINT('',#20387);
#1708=VERTEX_POINT('',#20563);
#1709=VERTEX_POINT('',#20564);
#1710=VERTEX_POINT('',#20895);
#1711=VERTEX_POINT('',#20896);
#1712=VERTEX_POINT('',#20898);
#1713=VERTEX_POINT('',#21067);
#1714=VERTEX_POINT('',#21272);
#1715=VERTEX_POINT('',#21273);
#1716=VERTEX_POINT('',#21437);
#1717=VERTEX_POINT('',#21618);
#1718=VERTEX_POINT('',#21619);
#1719=VERTEX_POINT('',#21657);
#1720=VERTEX_POINT('',#21659);
#1721=VERTEX_POINT('',#21661);
#1722=VERTEX_POINT('',#21672);
#1723=VERTEX_POINT('',#21899);
#1724=VERTEX_POINT('',#22126);
#1725=VERTEX_POINT('',#22353);
#1726=VERTEX_POINT('',#22580);
#1727=VERTEX_POINT('',#22807);
#1728=VERTEX_POINT('',#23034);
#1729=VERTEX_POINT('',#23045);
#1730=VERTEX_POINT('',#23052);
#1731=VERTEX_POINT('',#23054);
#1732=VERTEX_POINT('',#23064);
#1733=VERTEX_POINT('',#23291);
#1734=VERTEX_POINT('',#23518);
#1735=VERTEX_POINT('',#23745);
#1736=VERTEX_POINT('',#23972);
#1737=VERTEX_POINT('',#24199);
#1738=VERTEX_POINT('',#24656);
#1739=VERTEX_POINT('',#24785);
#1740=VERTEX_POINT('',#24787);
#1741=VERTEX_POINT('',#24946);
#1742=VERTEX_POINT('',#24947);
#1743=VERTEX_POINT('',#24962);
#1744=VERTEX_POINT('',#24972);
#1745=VERTEX_POINT('',#24989);
#1746=VERTEX_POINT('',#24991);
#1747=VERTEX_POINT('',#24995);
#1748=VERTEX_POINT('',#24996);
#1749=VERTEX_POINT('',#25046);
#1750=VERTEX_POINT('',#25054);
#1751=VERTEX_POINT('',#25062);
#1752=VERTEX_POINT('',#25113);
#1753=VERTEX_POINT('',#25166);
#1754=VERTEX_POINT('',#25181);
#1755=VERTEX_POINT('',#25524);
#1756=VERTEX_POINT('',#25850);
#1757=VERTEX_POINT('',#26044);
#1758=VERTEX_POINT('',#26045);
#1759=VERTEX_POINT('',#26047);
#1760=VERTEX_POINT('',#26052);
#1761=VERTEX_POINT('',#26110);
#1762=VERTEX_POINT('',#26111);
#1763=VERTEX_POINT('',#26113);
#1764=VERTEX_POINT('',#26269);
#1765=VERTEX_POINT('',#26501);
#1766=VERTEX_POINT('',#26502);
#1767=VERTEX_POINT('',#26504);
#1768=VERTEX_POINT('',#26735);
#1769=VERTEX_POINT('',#26967);
#1770=VERTEX_POINT('',#26968);
#1771=VERTEX_POINT('',#26970);
#1772=VERTEX_POINT('',#27204);
#1773=VERTEX_POINT('',#27433);
#1774=VERTEX_POINT('',#27434);
#1775=VERTEX_POINT('',#27436);
#1776=VERTEX_POINT('',#27524);
#1777=VERTEX_POINT('',#27753);
#1778=VERTEX_POINT('',#27754);
#1779=VERTEX_POINT('',#27756);
#1780=VERTEX_POINT('',#27911);
#1781=VERTEX_POINT('',#28143);
#1782=VERTEX_POINT('',#28144);
#1783=VERTEX_POINT('',#28146);
#1784=VERTEX_POINT('',#28380);
#1785=VERTEX_POINT('',#28609);
#1786=VERTEX_POINT('',#28610);
#1787=VERTEX_POINT('',#28612);
#1788=VERTEX_POINT('',#28840);
#1789=VERTEX_POINT('',#29075);
#1790=VERTEX_POINT('',#29076);
#1791=VERTEX_POINT('',#29078);
#1792=VERTEX_POINT('',#29161);
#1793=VERTEX_POINT('',#29167);
#1794=VERTEX_POINT('',#29169);
#1795=VERTEX_POINT('',#29320);
#1796=VERTEX_POINT('',#29321);
#1797=VERTEX_POINT('',#29323);
#1798=VERTEX_POINT('',#29364);
#1799=VERTEX_POINT('',#29375);
#1800=VERTEX_POINT('',#29720);
#1801=VERTEX_POINT('',#30073);
#1802=VERTEX_POINT('',#30422);
#1803=VERTEX_POINT('',#30634);
#1804=VERTEX_POINT('',#30765);
#1805=VERTEX_POINT('',#30767);
#1806=VERTEX_POINT('',#30958);
#1807=VERTEX_POINT('',#30970);
#1808=VERTEX_POINT('',#31313);
#1809=VERTEX_POINT('',#31662);
#1810=VERTEX_POINT('',#32201);
#1811=VERTEX_POINT('',#32432);
#1812=VERTEX_POINT('',#33525);
#1813=VERTEX_POINT('',#33526);
#1814=VERTEX_POINT('',#33530);
#1815=VERTEX_POINT('',#33532);
#1816=VERTEX_POINT('',#33534);
#1817=VERTEX_POINT('',#33543);
#1818=VERTEX_POINT('',#33554);
#1819=VERTEX_POINT('',#33569);
#1820=VERTEX_POINT('',#33629);
#1821=VERTEX_POINT('',#33664);
#1822=VERTEX_POINT('',#33666);
#1823=VERTEX_POINT('',#33675);
#1824=VERTEX_POINT('',#33686);
#1825=VERTEX_POINT('',#33701);
#1826=VERTEX_POINT('',#33721);
#1827=VERTEX_POINT('',#33723);
#1828=VERTEX_POINT('',#33725);
#1829=VERTEX_POINT('',#33727);
#1830=VERTEX_POINT('',#33731);
#1831=VERTEX_POINT('',#33735);
#1832=VERTEX_POINT('',#33737);
#1833=VERTEX_POINT('',#33739);
#1834=VERTEX_POINT('',#33741);
#1835=VERTEX_POINT('',#33745);
#1836=VERTEX_POINT('',#33749);
#1837=VERTEX_POINT('',#33751);
#1838=VERTEX_POINT('',#33755);
#1839=VERTEX_POINT('',#33756);
#1840=VERTEX_POINT('',#33761);
#1841=VERTEX_POINT('',#33762);
#1842=VERTEX_POINT('',#33767);
#1843=VERTEX_POINT('',#33768);
#1844=VERTEX_POINT('',#33773);
#1845=VERTEX_POINT('',#33774);
#1846=VERTEX_POINT('',#33779);
#1847=VERTEX_POINT('',#33780);
#1848=VERTEX_POINT('',#33785);
#1849=VERTEX_POINT('',#33786);
#1850=VERTEX_POINT('',#33791);
#1851=VERTEX_POINT('',#33792);
#1852=VERTEX_POINT('',#33797);
#1853=VERTEX_POINT('',#33798);
#1854=VERTEX_POINT('',#33803);
#1855=VERTEX_POINT('',#33804);
#1856=VERTEX_POINT('',#33809);
#1857=VERTEX_POINT('',#33810);
#1858=VERTEX_POINT('',#33815);
#1859=VERTEX_POINT('',#33816);
#1860=VERTEX_POINT('',#33821);
#1861=VERTEX_POINT('',#33822);
#1862=VERTEX_POINT('',#33827);
#1863=VERTEX_POINT('',#33832);
#1864=VERTEX_POINT('',#33836);
#1865=VERTEX_POINT('',#33837);
#1866=VERTEX_POINT('',#33842);
#1867=VERTEX_POINT('',#33843);
#1868=VERTEX_POINT('',#33848);
#1869=VERTEX_POINT('',#33849);
#1870=VERTEX_POINT('',#33854);
#1871=VERTEX_POINT('',#33855);
#1872=VERTEX_POINT('',#33860);
#1873=VERTEX_POINT('',#33861);
#1874=VERTEX_POINT('',#33866);
#1875=VERTEX_POINT('',#33867);
#1876=VERTEX_POINT('',#33872);
#1877=VERTEX_POINT('',#33873);
#1878=VERTEX_POINT('',#33878);
#1879=VERTEX_POINT('',#33879);
#1880=VERTEX_POINT('',#33884);
#1881=VERTEX_POINT('',#33885);
#1882=VERTEX_POINT('',#33890);
#1883=VERTEX_POINT('',#33891);
#1884=VERTEX_POINT('',#33896);
#1885=VERTEX_POINT('',#33897);
#1886=VERTEX_POINT('',#33902);
#1887=VERTEX_POINT('',#33903);
#1888=VERTEX_POINT('',#33908);
#1889=VERTEX_POINT('',#33909);
#1890=VERTEX_POINT('',#33914);
#1891=VERTEX_POINT('',#33915);
#1892=VERTEX_POINT('',#33920);
#1893=VERTEX_POINT('',#33921);
#1894=VERTEX_POINT('',#33926);
#1895=VERTEX_POINT('',#33933);
#1896=VERTEX_POINT('',#33935);
#1897=VERTEX_POINT('',#33939);
#1898=VERTEX_POINT('',#33943);
#1899=VERTEX_POINT('',#33947);
#1900=VERTEX_POINT('',#33951);
#1901=VERTEX_POINT('',#33955);
#1902=VERTEX_POINT('',#33959);
#1903=VERTEX_POINT('',#33963);
#1904=VERTEX_POINT('',#33967);
#1905=VERTEX_POINT('',#33971);
#1906=VERTEX_POINT('',#33975);
#1907=VERTEX_POINT('',#33979);
#1908=VERTEX_POINT('',#33983);
#1909=VERTEX_POINT('',#33987);
#1910=VERTEX_POINT('',#33993);
#1911=VERTEX_POINT('',#33995);
#1912=VERTEX_POINT('',#33997);
#1913=VERTEX_POINT('',#33999);
#1914=VERTEX_POINT('',#34001);
#1915=VERTEX_POINT('',#34003);
#1916=VERTEX_POINT('',#34005);
#1917=VERTEX_POINT('',#34007);
#1918=VERTEX_POINT('',#34009);
#1919=VERTEX_POINT('',#34012);
#1920=VERTEX_POINT('',#34013);
#1921=VERTEX_POINT('',#34015);
#1922=VERTEX_POINT('',#34017);
#1923=VERTEX_POINT('',#34021);
#1924=VERTEX_POINT('',#34026);
#1925=VERTEX_POINT('',#34030);
#1926=VERTEX_POINT('',#34034);
#1927=VERTEX_POINT('',#34038);
#1928=VERTEX_POINT('',#34042);
#1929=VERTEX_POINT('',#34046);
#1930=VERTEX_POINT('',#34050);
#1931=VERTEX_POINT('',#34054);
#1932=VERTEX_POINT('',#34058);
#1933=VERTEX_POINT('',#34062);
#1934=VERTEX_POINT('',#34066);
#1935=VERTEX_POINT('',#34070);
#1936=VERTEX_POINT('',#34074);
#1937=VERTEX_POINT('',#34078);
#1938=VERTEX_POINT('',#34082);
#1939=VERTEX_POINT('',#34086);
#1940=VERTEX_POINT('',#34090);
#1941=VERTEX_POINT('',#34095);
#1942=VERTEX_POINT('',#34099);
#1943=VERTEX_POINT('',#34103);
#1944=VERTEX_POINT('',#34104);
#1945=VERTEX_POINT('',#34109);
#1946=VERTEX_POINT('',#34110);
#1947=VERTEX_POINT('',#34115);
#1948=VERTEX_POINT('',#34116);
#1949=VERTEX_POINT('',#34121);
#1950=VERTEX_POINT('',#34122);
#1951=VERTEX_POINT('',#34127);
#1952=VERTEX_POINT('',#34128);
#1953=VERTEX_POINT('',#34133);
#1954=VERTEX_POINT('',#34134);
#1955=VERTEX_POINT('',#34139);
#1956=VERTEX_POINT('',#34140);
#1957=VERTEX_POINT('',#34145);
#1958=VERTEX_POINT('',#34146);
#1959=VERTEX_POINT('',#34151);
#1960=VERTEX_POINT('',#34152);
#1961=VERTEX_POINT('',#34157);
#1962=VERTEX_POINT('',#34158);
#1963=VERTEX_POINT('',#34193);
#1964=VERTEX_POINT('',#34195);
#1965=VERTEX_POINT('',#34197);
#1966=VERTEX_POINT('',#34199);
#1967=VERTEX_POINT('',#34201);
#1968=VERTEX_POINT('',#34203);
#1969=VERTEX_POINT('',#34205);
#1970=VERTEX_POINT('',#34207);
#1971=VERTEX_POINT('',#34209);
#1972=VERTEX_POINT('',#34212);
#1973=VERTEX_POINT('',#34214);
#1974=VERTEX_POINT('',#34218);
#1975=VERTEX_POINT('',#34220);
#1976=VERTEX_POINT('',#34244);
#1977=VERTEX_POINT('',#34245);
#1978=VERTEX_POINT('',#34247);
#1979=VERTEX_POINT('',#34249);
#1980=VERTEX_POINT('',#34251);
#1981=VERTEX_POINT('',#34253);
#1982=VERTEX_POINT('',#34257);
#1983=VERTEX_POINT('',#34258);
#1984=VERTEX_POINT('',#34260);
#1985=VERTEX_POINT('',#34262);
#1986=VERTEX_POINT('',#34264);
#1987=VERTEX_POINT('',#34284);
#1988=VERTEX_POINT('',#34288);
#1989=VERTEX_POINT('',#34289);
#1990=VERTEX_POINT('',#34312);
#1991=VERTEX_POINT('',#34315);
#1992=VERTEX_POINT('',#34323);
#1993=VERTEX_POINT('',#34325);
#1994=VERTEX_POINT('',#34329);
#1995=VERTEX_POINT('',#34333);
#1996=VERTEX_POINT('',#34337);
#1997=VERTEX_POINT('',#34343);
#1998=VERTEX_POINT('',#34351);
#1999=VERTEX_POINT('',#34352);
#2000=VERTEX_POINT('',#34354);
#2001=VERTEX_POINT('',#34356);
#2002=VERTEX_POINT('',#34360);
#2003=VERTEX_POINT('',#34362);
#2004=VERTEX_POINT('',#34366);
#2005=VERTEX_POINT('',#34368);
#2006=EDGE_CURVE('',#1540,#1541,#1288,.T.);
#2007=EDGE_CURVE('',#1541,#1540,#1289,.T.);
#2008=EDGE_CURVE('',#1541,#1542,#1014,.T.);
#2009=EDGE_CURVE('',#1543,#1542,#1290,.T.);
#2010=EDGE_CURVE('',#1542,#1543,#1291,.T.);
#2011=EDGE_CURVE('',#1544,#1545,#1292,.T.);
#2012=EDGE_CURVE('',#1545,#1544,#1293,.T.);
#2013=EDGE_CURVE('',#1545,#1546,#1015,.T.);
#2014=EDGE_CURVE('',#1547,#1546,#1294,.T.);
#2015=EDGE_CURVE('',#1546,#1547,#1295,.T.);
#2016=EDGE_CURVE('',#1548,#1548,#160,.T.);
#2017=EDGE_CURVE('',#1548,#1549,#161,.T.);
#2018=EDGE_CURVE('',#1549,#1550,#162,.T.);
#2019=EDGE_CURVE('',#1550,#1549,#163,.T.);
#2020=EDGE_CURVE('',#1551,#1551,#164,.T.);
#2021=EDGE_CURVE('',#1552,#1553,#165,.T.);
#2022=EDGE_CURVE('',#1553,#1552,#166,.T.);
#2023=EDGE_CURVE('',#1553,#1550,#1016,.T.);
#2024=EDGE_CURVE('',#1551,#1554,#167,.T.);
#2025=EDGE_CURVE('',#1554,#1555,#168,.T.);
#2026=EDGE_CURVE('',#1555,#1554,#169,.T.);
#2027=EDGE_CURVE('',#1555,#1556,#1017,.T.);
#2028=EDGE_CURVE('',#1557,#1556,#170,.T.);
#2029=EDGE_CURVE('',#1556,#1557,#171,.T.);
#2030=EDGE_CURVE('',#1558,#1558,#172,.T.);
#2031=EDGE_CURVE('',#1558,#1557,#173,.T.);
#2032=EDGE_CURVE('',#1559,#1559,#174,.T.);
#2033=EDGE_CURVE('',#1559,#1552,#175,.T.);
#2034=EDGE_CURVE('',#1560,#1560,#176,.T.);
#2035=EDGE_CURVE('',#1560,#1561,#1018,.T.);
#2036=EDGE_CURVE('',#1561,#1561,#177,.T.);
#2037=EDGE_CURVE('',#1562,#1562,#178,.T.);
#2038=EDGE_CURVE('',#1562,#1563,#1019,.T.);
#2039=EDGE_CURVE('',#1563,#1563,#179,.T.);
#2040=EDGE_CURVE('',#1564,#1564,#180,.F.);
#2041=EDGE_CURVE('',#1564,#1565,#1020,.T.);
#2042=EDGE_CURVE('',#1565,#1565,#181,.F.);
#2043=EDGE_CURVE('',#1566,#1567,#1021,.T.);
#2044=EDGE_CURVE('',#1567,#1568,#1296,.T.);
#2045=EDGE_CURVE('',#1569,#1568,#182,.T.);
#2046=EDGE_CURVE('',#1566,#1569,#1297,.T.);
#2047=EDGE_CURVE('',#1570,#1571,#1022,.T.);
#2048=EDGE_CURVE('',#1571,#1572,#1298,.T.);
#2049=EDGE_CURVE('',#1572,#1567,#1299,.T.);
#2050=EDGE_CURVE('',#1573,#1566,#1300,.T.);
#2051=EDGE_CURVE('',#1570,#1573,#1301,.T.);
#2052=EDGE_CURVE('',#1574,#1575,#1023,.T.);
#2053=EDGE_CURVE('',#1575,#1576,#1302,.T.);
#2054=EDGE_CURVE('',#1576,#1571,#1303,.T.);
#2055=EDGE_CURVE('',#1577,#1570,#1304,.T.);
#2056=EDGE_CURVE('',#1574,#1577,#1305,.T.);
#2057=EDGE_CURVE('',#1578,#1579,#1024,.T.);
#2058=EDGE_CURVE('',#1579,#1580,#1306,.T.);
#2059=EDGE_CURVE('',#1580,#1575,#1307,.T.);
#2060=EDGE_CURVE('',#1581,#1574,#1308,.T.);
#2061=EDGE_CURVE('',#1578,#1581,#1309,.T.);
#2062=EDGE_CURVE('',#1582,#1583,#1025,.T.);
#2063=EDGE_CURVE('',#1583,#1584,#1310,.T.);
#2064=EDGE_CURVE('',#1584,#1579,#1311,.T.);
#2065=EDGE_CURVE('',#1585,#1578,#1312,.T.);
#2066=EDGE_CURVE('',#1582,#1585,#1313,.T.);
#2067=EDGE_CURVE('',#1586,#1587,#1026,.T.);
#2068=EDGE_CURVE('',#1587,#1588,#1314,.T.);
#2069=EDGE_CURVE('',#1588,#1583,#1315,.T.);
#2070=EDGE_CURVE('',#1589,#1582,#1316,.T.);
#2071=EDGE_CURVE('',#1586,#1589,#1317,.T.);
#2072=EDGE_CURVE('',#1590,#1591,#1027,.T.);
#2073=EDGE_CURVE('',#1591,#1592,#1318,.T.);
#2074=EDGE_CURVE('',#1592,#1587,#1319,.T.);
#2075=EDGE_CURVE('',#1593,#1586,#1320,.T.);
#2076=EDGE_CURVE('',#1590,#1593,#1321,.T.);
#2077=EDGE_CURVE('',#1594,#1595,#1028,.T.);
#2078=EDGE_CURVE('',#1596,#1594,#1322,.T.);
#2079=EDGE_CURVE('',#1597,#1596,#1323,.T.);
#2080=EDGE_CURVE('',#1598,#1597,#183,.T.);
#2081=EDGE_CURVE('',#1598,#1599,#1324,.T.);
#2082=EDGE_CURVE('',#1599,#1595,#1325,.T.);
#2083=EDGE_CURVE('',#1600,#1601,#1029,.T.);
#2084=EDGE_CURVE('',#1601,#1602,#1326,.T.);
#2085=EDGE_CURVE('',#1602,#1603,#1327,.T.);
#2086=EDGE_CURVE('',#1604,#1603,#184,.F.);
#2087=EDGE_CURVE('',#1604,#1605,#1328,.T.);
#2088=EDGE_CURVE('',#1605,#1600,#1329,.T.);
#2089=EDGE_CURVE('',#1606,#1607,#1030,.T.);
#2090=EDGE_CURVE('',#1607,#1608,#1330,.T.);
#2091=EDGE_CURVE('',#1608,#1601,#1331,.T.);
#2092=EDGE_CURVE('',#1600,#1609,#1332,.T.);
#2093=EDGE_CURVE('',#1609,#1606,#1333,.T.);
#2094=EDGE_CURVE('',#1610,#1611,#1031,.T.);
#2095=EDGE_CURVE('',#1611,#1612,#1334,.T.);
#2096=EDGE_CURVE('',#1612,#1607,#1335,.T.);
#2097=EDGE_CURVE('',#1606,#1613,#1336,.T.);
#2098=EDGE_CURVE('',#1613,#1610,#1337,.T.);
#2099=EDGE_CURVE('',#1614,#1615,#1032,.T.);
#2100=EDGE_CURVE('',#1615,#1611,#1338,.T.);
#2101=EDGE_CURVE('',#1610,#1616,#1339,.T.);
#2102=EDGE_CURVE('',#1616,#1614,#1340,.T.);
#2103=EDGE_CURVE('',#1617,#1618,#1033,.T.);
#2104=EDGE_CURVE('',#1618,#1619,#1341,.T.);
#2105=EDGE_CURVE('',#1619,#1615,#1342,.T.);
#2106=EDGE_CURVE('',#1614,#1620,#1343,.T.);
#2107=EDGE_CURVE('',#1620,#1617,#1344,.T.);
#2108=EDGE_CURVE('',#1621,#1622,#1034,.T.);
#2109=EDGE_CURVE('',#1622,#1618,#1345,.T.);
#2110=EDGE_CURVE('',#1617,#1623,#1346,.T.);
#2111=EDGE_CURVE('',#1623,#1621,#1347,.T.);
#2112=EDGE_CURVE('',#1624,#1625,#1035,.T.);
#2113=EDGE_CURVE('',#1625,#1626,#1348,.T.);
#2114=EDGE_CURVE('',#1626,#1622,#1349,.T.);
#2115=EDGE_CURVE('',#1621,#1627,#1350,.T.);
#2116=EDGE_CURVE('',#1627,#1624,#1351,.T.);
#2117=EDGE_CURVE('',#1628,#1628,#185,.F.);
#2118=EDGE_CURVE('',#1628,#1629,#1036,.T.);
#2119=EDGE_CURVE('',#1629,#1630,#186,.T.);
#2120=EDGE_CURVE('',#1630,#1631,#1352,.T.);
#2121=EDGE_CURVE('',#1632,#1631,#1037,.T.);
#2122=EDGE_CURVE('',#1632,#1633,#1353,.T.);
#2123=EDGE_CURVE('',#1633,#1629,#187,.T.);
#2124=EDGE_CURVE('',#1631,#1625,#1354,.T.);
#2125=EDGE_CURVE('',#1624,#1634,#1355,.T.);
#2126=EDGE_CURVE('',#1634,#1632,#1356,.T.);
#2127=EDGE_CURVE('',#1595,#1635,#1357,.T.);
#2128=EDGE_CURVE('',#1635,#1591,#1358,.T.);
#2129=EDGE_CURVE('',#1636,#1590,#1359,.T.);
#2130=EDGE_CURVE('',#1594,#1636,#1360,.T.);
#2131=EDGE_CURVE('',#1568,#1604,#1361,.T.);
#2132=EDGE_CURVE('',#1633,#1598,#1362,.T.);
#2133=EDGE_CURVE('',#1597,#1630,#1363,.T.);
#2134=EDGE_CURVE('',#1603,#1569,#1364,.T.);
#2135=EDGE_CURVE('',#1637,#1637,#188,.T.);
#2136=EDGE_CURVE('',#1637,#1638,#1038,.T.);
#2137=EDGE_CURVE('',#1638,#1638,#189,.T.);
#2138=EDGE_CURVE('',#1639,#1639,#190,.T.);
#2139=EDGE_CURVE('',#1640,#1640,#191,.T.);
#2140=EDGE_CURVE('',#1639,#1640,#1039,.T.);
#2141=EDGE_CURVE('',#1641,#1642,#1040,.T.);
#2142=EDGE_CURVE('',#1643,#1641,#1365,.F.);
#2143=EDGE_CURVE('',#1644,#1643,#192,.T.);
#2144=EDGE_CURVE('',#1644,#1642,#1366,.T.);
#2145=EDGE_CURVE('',#1645,#1646,#1041,.T.);
#2146=EDGE_CURVE('',#1641,#1645,#1367,.F.);
#2147=EDGE_CURVE('',#1642,#1646,#1368,.T.);
#2148=EDGE_CURVE('',#1647,#1648,#1042,.T.);
#2149=EDGE_CURVE('',#1645,#1647,#1369,.F.);
#2150=EDGE_CURVE('',#1646,#1648,#1370,.T.);
#2151=EDGE_CURVE('',#1649,#1650,#1043,.T.);
#2152=EDGE_CURVE('',#1647,#1649,#1371,.F.);
#2153=EDGE_CURVE('',#1648,#1650,#1372,.T.);
#2154=EDGE_CURVE('',#1651,#1652,#1044,.T.);
#2155=EDGE_CURVE('',#1649,#1651,#1373,.F.);
#2156=EDGE_CURVE('',#1650,#1652,#1374,.T.);
#2157=EDGE_CURVE('',#1653,#1654,#1045,.T.);
#2158=EDGE_CURVE('',#1651,#1653,#1375,.F.);
#2159=EDGE_CURVE('',#1652,#1654,#1376,.T.);
#2160=EDGE_CURVE('',#1655,#1656,#1377,.T.);
#2161=EDGE_CURVE('',#1657,#1656,#193,.F.);
#2162=EDGE_CURVE('',#1657,#1658,#1378,.T.);
#2163=EDGE_CURVE('',#1658,#1659,#1379,.T.);
#2164=EDGE_CURVE('',#1659,#1660,#1380,.T.);
#2165=EDGE_CURVE('',#1660,#1661,#1381,.T.);
#2166=EDGE_CURVE('',#1661,#1662,#1382,.T.);
#2167=EDGE_CURVE('',#1662,#1663,#1383,.T.);
#2168=EDGE_CURVE('',#1663,#1664,#1384,.T.);
#2169=EDGE_CURVE('',#1664,#1665,#1385,.T.);
#2170=EDGE_CURVE('',#1666,#1665,#194,.T.);
#2171=EDGE_CURVE('',#1666,#1667,#1386,.T.);
#2172=EDGE_CURVE('',#1667,#1668,#1387,.T.);
#2173=EDGE_CURVE('',#1668,#1669,#1388,.T.);
#2174=EDGE_CURVE('',#1669,#1670,#1389,.T.);
#2175=EDGE_CURVE('',#1670,#1671,#1390,.T.);
#2176=EDGE_CURVE('',#1671,#1672,#1391,.T.);
#2177=EDGE_CURVE('',#1672,#1655,#1392,.T.);
#2178=EDGE_CURVE('',#1654,#1673,#1393,.T.);
#2179=EDGE_CURVE('',#1674,#1673,#195,.T.);
#2180=EDGE_CURVE('',#1653,#1674,#1394,.F.);
#2181=EDGE_CURVE('',#1675,#1676,#1395,.T.);
#2182=EDGE_CURVE('',#1676,#1677,#1396,.T.);
#2183=EDGE_CURVE('',#1677,#1678,#1397,.T.);
#2184=EDGE_CURVE('',#1678,#1675,#1046,.T.);
#2185=EDGE_CURVE('',#1679,#1677,#1047,.T.);
#2186=EDGE_CURVE('',#1680,#1679,#196,.T.);
#2187=EDGE_CURVE('',#1676,#1680,#1048,.T.);
#2188=EDGE_CURVE('',#1681,#1682,#1398,.T.);
#2189=EDGE_CURVE('',#1681,#1683,#1049,.T.);
#2190=EDGE_CURVE('',#1683,#1679,#1399,.T.);
#2191=EDGE_CURVE('',#1680,#1684,#1400,.T.);
#2192=EDGE_CURVE('',#1684,#1685,#1050,.T.);
#2193=EDGE_CURVE('',#1682,#1685,#1401,.T.);
#2194=EDGE_CURVE('',#1682,#1686,#1051,.T.);
#2195=EDGE_CURVE('',#1686,#1686,#197,.T.);
#2196=EDGE_CURVE('',#1687,#1681,#1402,.T.);
#2197=EDGE_CURVE('',#1685,#1688,#1403,.T.);
#2198=EDGE_CURVE('',#1688,#1687,#1052,.T.);
#2199=EDGE_CURVE('',#1683,#1684,#198,.T.);
#2200=EDGE_CURVE('',#1665,#1674,#1404,.T.);
#2201=EDGE_CURVE('',#1689,#1657,#1405,.T.);
#2202=EDGE_CURVE('',#1689,#1643,#1406,.T.);
#2203=EDGE_CURVE('',#1690,#1666,#1407,.T.);
#2204=EDGE_CURVE('',#1673,#1690,#1408,.T.);
#2205=EDGE_CURVE('',#1656,#1644,#1409,.T.);
#2206=EDGE_CURVE('',#1691,#1692,#1053,.T.);
#2207=EDGE_CURVE('',#1693,#1691,#1410,.F.);
#2208=EDGE_CURVE('',#1694,#1693,#199,.F.);
#2209=EDGE_CURVE('',#1694,#1692,#1411,.T.);
#2210=EDGE_CURVE('',#1695,#1696,#1054,.T.);
#2211=EDGE_CURVE('',#1691,#1695,#1412,.F.);
#2212=EDGE_CURVE('',#1692,#1697,#1413,.T.);
#2213=EDGE_CURVE('',#1697,#1696,#1414,.T.);
#2214=EDGE_CURVE('',#1698,#1699,#1055,.T.);
#2215=EDGE_CURVE('',#1700,#1698,#1415,.F.);
#2216=EDGE_CURVE('',#1695,#1700,#1416,.F.);
#2217=EDGE_CURVE('',#1696,#1701,#1417,.T.);
#2218=EDGE_CURVE('',#1701,#1699,#1418,.T.);
#2219=EDGE_CURVE('',#1702,#1703,#1056,.T.);
#2220=EDGE_CURVE('',#1698,#1702,#1419,.F.);
#2221=EDGE_CURVE('',#1699,#1703,#1420,.T.);
#2222=EDGE_CURVE('',#1704,#1705,#1057,.T.);
#2223=EDGE_CURVE('',#1706,#1704,#1421,.F.);
#2224=EDGE_CURVE('',#1702,#1706,#1422,.F.);
#2225=EDGE_CURVE('',#1703,#1707,#1423,.T.);
#2226=EDGE_CURVE('',#1707,#1705,#1424,.T.);
#2227=EDGE_CURVE('',#1708,#1709,#1058,.T.);
#2228=EDGE_CURVE('',#1704,#1708,#1425,.F.);
#2229=EDGE_CURVE('',#1705,#1709,#1426,.T.);
#2230=EDGE_CURVE('',#1710,#1711,#1059,.T.);
#2231=EDGE_CURVE('',#1712,#1710,#1427,.F.);
#2232=EDGE_CURVE('',#1708,#1712,#1428,.F.);
#2233=EDGE_CURVE('',#1709,#1713,#1429,.T.);
#2234=EDGE_CURVE('',#1713,#1711,#1430,.T.);
#2235=EDGE_CURVE('',#1714,#1715,#1060,.T.);
#2236=EDGE_CURVE('',#1710,#1714,#1431,.F.);
#2237=EDGE_CURVE('',#1711,#1716,#1432,.T.);
#2238=EDGE_CURVE('',#1716,#1715,#1433,.F.);
#2239=EDGE_CURVE('',#1717,#1718,#1434,.T.);
#2240=EDGE_CURVE('',#1719,#1718,#200,.T.);
#2241=EDGE_CURVE('',#1719,#1720,#201,.T.);
#2242=EDGE_CURVE('',#1720,#1721,#1435,.T.);
#2243=EDGE_CURVE('',#1721,#1722,#1436,.T.);
#2244=EDGE_CURVE('',#1722,#1723,#1437,.T.);
#2245=EDGE_CURVE('',#1723,#1724,#1438,.T.);
#2246=EDGE_CURVE('',#1724,#1725,#1439,.T.);
#2247=EDGE_CURVE('',#1725,#1726,#1440,.T.);
#2248=EDGE_CURVE('',#1726,#1727,#1441,.T.);
#2249=EDGE_CURVE('',#1727,#1728,#1442,.T.);
#2250=EDGE_CURVE('',#1728,#1729,#1443,.T.);
#2251=EDGE_CURVE('',#1730,#1729,#202,.F.);
#2252=EDGE_CURVE('',#1730,#1731,#1444,.T.);
#2253=EDGE_CURVE('',#1731,#1732,#1445,.T.);
#2254=EDGE_CURVE('',#1732,#1733,#1446,.T.);
#2255=EDGE_CURVE('',#1733,#1734,#1447,.T.);
#2256=EDGE_CURVE('',#1734,#1735,#1448,.T.);
#2257=EDGE_CURVE('',#1735,#1736,#1449,.T.);
#2258=EDGE_CURVE('',#1736,#1737,#1450,.T.);
#2259=EDGE_CURVE('',#1737,#1717,#1451,.T.);
#2260=EDGE_CURVE('',#1715,#1738,#1452,.F.);
#2261=EDGE_CURVE('',#1739,#1738,#203,.T.);
#2262=EDGE_CURVE('',#1740,#1739,#1453,.T.);
#2263=EDGE_CURVE('',#1714,#1740,#1454,.F.);
#2264=EDGE_CURVE('',#1741,#1742,#1455,.T.);
#2265=EDGE_CURVE('',#1742,#1743,#1456,.T.);
#2266=EDGE_CURVE('',#1743,#1744,#1457,.T.);
#2267=EDGE_CURVE('',#1744,#1741,#1061,.T.);
#2268=EDGE_CURVE('',#1745,#1743,#1062,.T.);
#2269=EDGE_CURVE('',#1746,#1745,#204,.T.);
#2270=EDGE_CURVE('',#1742,#1746,#1063,.T.);
#2271=EDGE_CURVE('',#1747,#1748,#1458,.T.);
#2272=EDGE_CURVE('',#1747,#1749,#1064,.T.);
#2273=EDGE_CURVE('',#1749,#1745,#1459,.T.);
#2274=EDGE_CURVE('',#1746,#1750,#1460,.T.);
#2275=EDGE_CURVE('',#1750,#1751,#1065,.T.);
#2276=EDGE_CURVE('',#1748,#1751,#1461,.T.);
#2277=EDGE_CURVE('',#1748,#1752,#1066,.T.);
#2278=EDGE_CURVE('',#1752,#1752,#205,.F.);
#2279=EDGE_CURVE('',#1753,#1747,#1462,.T.);
#2280=EDGE_CURVE('',#1751,#1754,#1463,.T.);
#2281=EDGE_CURVE('',#1754,#1753,#1067,.T.);
#2282=EDGE_CURVE('',#1749,#1750,#206,.T.);
#2283=EDGE_CURVE('',#1729,#1739,#1464,.T.);
#2284=EDGE_CURVE('',#1755,#1719,#1465,.F.);
#2285=EDGE_CURVE('',#1755,#1693,#1466,.T.);
#2286=EDGE_CURVE('',#1756,#1730,#1467,.T.);
#2287=EDGE_CURVE('',#1738,#1756,#1468,.T.);
#2288=EDGE_CURVE('',#1718,#1694,#1469,.F.);
#2289=EDGE_CURVE('',#1757,#1758,#1068,.T.);
#2290=EDGE_CURVE('',#1758,#1759,#1470,.T.);
#2291=EDGE_CURVE('',#1760,#1759,#207,.T.);
#2292=EDGE_CURVE('',#1757,#1760,#1471,.T.);
#2293=EDGE_CURVE('',#1761,#1762,#1069,.T.);
#2294=EDGE_CURVE('',#1762,#1763,#1472,.T.);
#2295=EDGE_CURVE('',#1763,#1758,#1473,.T.);
#2296=EDGE_CURVE('',#1764,#1757,#1474,.T.);
#2297=EDGE_CURVE('',#1761,#1764,#1475,.T.);
#2298=EDGE_CURVE('',#1765,#1766,#1070,.T.);
#2299=EDGE_CURVE('',#1766,#1767,#1476,.T.);
#2300=EDGE_CURVE('',#1767,#1762,#1477,.T.);
#2301=EDGE_CURVE('',#1768,#1761,#1478,.T.);
#2302=EDGE_CURVE('',#1765,#1768,#1479,.T.);
#2303=EDGE_CURVE('',#1769,#1770,#1071,.T.);
#2304=EDGE_CURVE('',#1770,#1771,#1480,.T.);
#2305=EDGE_CURVE('',#1771,#1766,#1481,.T.);
#2306=EDGE_CURVE('',#1772,#1765,#1482,.T.);
#2307=EDGE_CURVE('',#1769,#1772,#1483,.T.);
#2308=EDGE_CURVE('',#1773,#1774,#1072,.T.);
#2309=EDGE_CURVE('',#1774,#1775,#1484,.T.);
#2310=EDGE_CURVE('',#1775,#1770,#1485,.T.);
#2311=EDGE_CURVE('',#1776,#1769,#1486,.T.);
#2312=EDGE_CURVE('',#1773,#1776,#1487,.T.);
#2313=EDGE_CURVE('',#1777,#1778,#1073,.T.);
#2314=EDGE_CURVE('',#1778,#1779,#1488,.T.);
#2315=EDGE_CURVE('',#1779,#1774,#1489,.T.);
#2316=EDGE_CURVE('',#1780,#1773,#1490,.T.);
#2317=EDGE_CURVE('',#1777,#1780,#1491,.T.);
#2318=EDGE_CURVE('',#1781,#1782,#1074,.T.);
#2319=EDGE_CURVE('',#1782,#1783,#1492,.T.);
#2320=EDGE_CURVE('',#1783,#1778,#1493,.T.);
#2321=EDGE_CURVE('',#1784,#1777,#1494,.T.);
#2322=EDGE_CURVE('',#1781,#1784,#1495,.T.);
#2323=EDGE_CURVE('',#1785,#1786,#1075,.T.);
#2324=EDGE_CURVE('',#1786,#1787,#1496,.T.);
#2325=EDGE_CURVE('',#1787,#1782,#1497,.T.);
#2326=EDGE_CURVE('',#1788,#1781,#1498,.T.);
#2327=EDGE_CURVE('',#1785,#1788,#1499,.T.);
#2328=EDGE_CURVE('',#1789,#1790,#1076,.T.);
#2329=EDGE_CURVE('',#1791,#1789,#1500,.T.);
#2330=EDGE_CURVE('',#1792,#1791,#1501,.T.);
#2331=EDGE_CURVE('',#1793,#1792,#208,.T.);
#2332=EDGE_CURVE('',#1793,#1794,#1502,.T.);
#2333=EDGE_CURVE('',#1794,#1790,#1503,.T.);
#2334=EDGE_CURVE('',#1795,#1796,#209,.T.);
#2335=EDGE_CURVE('',#1795,#1797,#1504,.T.);
#2336=EDGE_CURVE('',#1797,#1798,#1505,.T.);
#2337=EDGE_CURVE('',#1798,#1799,#1506,.T.);
#2338=EDGE_CURVE('',#1799,#1800,#1507,.T.);
#2339=EDGE_CURVE('',#1800,#1801,#1508,.T.);
#2340=EDGE_CURVE('',#1801,#1802,#1509,.T.);
#2341=EDGE_CURVE('',#1802,#1803,#1510,.T.);
#2342=EDGE_CURVE('',#1803,#1804,#210,.T.);
#2343=EDGE_CURVE('',#1804,#1805,#1511,.T.);
#2344=EDGE_CURVE('',#1805,#1806,#1512,.T.);
#2345=EDGE_CURVE('',#1806,#1807,#1513,.T.);
#2346=EDGE_CURVE('',#1807,#1808,#1514,.T.);
#2347=EDGE_CURVE('',#1808,#1809,#1515,.T.);
#2348=EDGE_CURVE('',#1809,#1796,#1516,.T.);
#2349=EDGE_CURVE('',#1790,#1810,#1517,.T.);
#2350=EDGE_CURVE('',#1810,#1786,#1518,.T.);
#2351=EDGE_CURVE('',#1811,#1785,#1519,.T.);
#2352=EDGE_CURVE('',#1789,#1811,#1520,.T.);
#2353=EDGE_CURVE('',#1759,#1795,#1521,.T.);
#2354=EDGE_CURVE('',#1803,#1793,#1522,.T.);
#2355=EDGE_CURVE('',#1796,#1760,#1523,.T.);
#2356=EDGE_CURVE('',#1792,#1804,#1524,.T.);
#2357=EDGE_CURVE('',#1812,#1813,#211,.T.);
#2358=EDGE_CURVE('',#1813,#1812,#212,.T.);
#2359=EDGE_CURVE('',#1814,#1814,#213,.T.);
#2360=EDGE_CURVE('',#1814,#1815,#1077,.T.);
#2361=EDGE_CURVE('',#1816,#1815,#1525,.T.);
#2362=EDGE_CURVE('',#1817,#1816,#1526,.T.);
#2363=EDGE_CURVE('',#1818,#1817,#1527,.T.);
#2364=EDGE_CURVE('',#1819,#1818,#1528,.T.);
#2365=EDGE_CURVE('',#1815,#1819,#1529,.T.);
#2366=EDGE_CURVE('',#1813,#1812,#1530,.T.);
#2367=EDGE_CURVE('',#1812,#1813,#1531,.F.);
#2368=EDGE_CURVE('',#1820,#1820,#1532,.T.);
#2369=EDGE_CURVE('',#1820,#1821,#1078,.T.);
#2370=EDGE_CURVE('',#1822,#1821,#1533,.T.);
#2371=EDGE_CURVE('',#1823,#1822,#1534,.T.);
#2372=EDGE_CURVE('',#1824,#1823,#1535,.T.);
#2373=EDGE_CURVE('',#1825,#1824,#1536,.T.);
#2374=EDGE_CURVE('',#1821,#1825,#1537,.T.);
#2375=EDGE_CURVE('',#1825,#1826,#1079,.T.);
#2376=EDGE_CURVE('',#1827,#1826,#214,.T.);
#2377=EDGE_CURVE('',#1827,#1828,#1080,.T.);
#2378=EDGE_CURVE('',#1829,#1828,#215,.T.);
#2379=EDGE_CURVE('',#1829,#1822,#1081,.T.);
#2380=EDGE_CURVE('',#1830,#1824,#1082,.T.);
#2381=EDGE_CURVE('',#1826,#1830,#216,.T.);
#2382=EDGE_CURVE('',#1819,#1831,#1083,.T.);
#2383=EDGE_CURVE('',#1832,#1831,#217,.T.);
#2384=EDGE_CURVE('',#1832,#1833,#1084,.T.);
#2385=EDGE_CURVE('',#1834,#1833,#218,.T.);
#2386=EDGE_CURVE('',#1834,#1816,#1085,.T.);
#2387=EDGE_CURVE('',#1835,#1818,#1086,.T.);
#2388=EDGE_CURVE('',#1831,#1835,#219,.T.);
#2389=EDGE_CURVE('',#1826,#1836,#220,.T.);
#2390=EDGE_CURVE('',#1836,#1837,#221,.T.);
#2391=EDGE_CURVE('',#1837,#1827,#222,.T.);
#2392=EDGE_CURVE('',#1838,#1839,#223,.T.);
#2393=EDGE_CURVE('',#1839,#1827,#224,.T.);
#2394=EDGE_CURVE('',#1837,#1838,#225,.T.);
#2395=EDGE_CURVE('',#1840,#1841,#226,.T.);
#2396=EDGE_CURVE('',#1841,#1839,#227,.T.);
#2397=EDGE_CURVE('',#1838,#1840,#228,.T.);
#2398=EDGE_CURVE('',#1842,#1843,#229,.T.);
#2399=EDGE_CURVE('',#1843,#1841,#230,.T.);
#2400=EDGE_CURVE('',#1840,#1842,#231,.T.);
#2401=EDGE_CURVE('',#1844,#1845,#232,.T.);
#2402=EDGE_CURVE('',#1845,#1843,#233,.T.);
#2403=EDGE_CURVE('',#1842,#1844,#234,.T.);
#2404=EDGE_CURVE('',#1846,#1847,#235,.T.);
#2405=EDGE_CURVE('',#1847,#1845,#236,.T.);
#2406=EDGE_CURVE('',#1844,#1846,#237,.T.);
#2407=EDGE_CURVE('',#1848,#1849,#238,.T.);
#2408=EDGE_CURVE('',#1849,#1847,#239,.T.);
#2409=EDGE_CURVE('',#1846,#1848,#240,.T.);
#2410=EDGE_CURVE('',#1850,#1851,#241,.T.);
#2411=EDGE_CURVE('',#1851,#1849,#242,.T.);
#2412=EDGE_CURVE('',#1848,#1850,#243,.T.);
#2413=EDGE_CURVE('',#1852,#1853,#244,.T.);
#2414=EDGE_CURVE('',#1853,#1851,#245,.T.);
#2415=EDGE_CURVE('',#1850,#1852,#246,.T.);
#2416=EDGE_CURVE('',#1854,#1855,#247,.T.);
#2417=EDGE_CURVE('',#1855,#1853,#248,.T.);
#2418=EDGE_CURVE('',#1852,#1854,#249,.T.);
#2419=EDGE_CURVE('',#1856,#1857,#250,.T.);
#2420=EDGE_CURVE('',#1857,#1855,#251,.T.);
#2421=EDGE_CURVE('',#1854,#1856,#252,.T.);
#2422=EDGE_CURVE('',#1858,#1859,#253,.T.);
#2423=EDGE_CURVE('',#1859,#1857,#254,.T.);
#2424=EDGE_CURVE('',#1856,#1858,#255,.T.);
#2425=EDGE_CURVE('',#1860,#1861,#256,.T.);
#2426=EDGE_CURVE('',#1861,#1859,#257,.T.);
#2427=EDGE_CURVE('',#1858,#1860,#258,.T.);
#2428=EDGE_CURVE('',#1862,#1833,#259,.T.);
#2429=EDGE_CURVE('',#1833,#1861,#260,.T.);
#2430=EDGE_CURVE('',#1860,#1862,#261,.T.);
#2431=EDGE_CURVE('',#1863,#1834,#262,.T.);
#2432=EDGE_CURVE('',#1862,#1863,#263,.T.);
#2433=EDGE_CURVE('',#1864,#1865,#264,.T.);
#2434=EDGE_CURVE('',#1865,#1834,#265,.T.);
#2435=EDGE_CURVE('',#1863,#1864,#266,.T.);
#2436=EDGE_CURVE('',#1866,#1867,#267,.T.);
#2437=EDGE_CURVE('',#1867,#1865,#268,.T.);
#2438=EDGE_CURVE('',#1864,#1866,#269,.T.);
#2439=EDGE_CURVE('',#1868,#1869,#270,.T.);
#2440=EDGE_CURVE('',#1869,#1867,#271,.T.);
#2441=EDGE_CURVE('',#1866,#1868,#272,.T.);
#2442=EDGE_CURVE('',#1870,#1871,#273,.T.);
#2443=EDGE_CURVE('',#1871,#1869,#274,.T.);
#2444=EDGE_CURVE('',#1868,#1870,#275,.T.);
#2445=EDGE_CURVE('',#1872,#1873,#276,.T.);
#2446=EDGE_CURVE('',#1873,#1871,#277,.T.);
#2447=EDGE_CURVE('',#1870,#1872,#278,.T.);
#2448=EDGE_CURVE('',#1874,#1875,#279,.T.);
#2449=EDGE_CURVE('',#1875,#1873,#280,.T.);
#2450=EDGE_CURVE('',#1872,#1874,#281,.T.);
#2451=EDGE_CURVE('',#1876,#1877,#282,.T.);
#2452=EDGE_CURVE('',#1877,#1875,#283,.T.);
#2453=EDGE_CURVE('',#1874,#1876,#284,.T.);
#2454=EDGE_CURVE('',#1878,#1879,#285,.T.);
#2455=EDGE_CURVE('',#1879,#1877,#286,.T.);
#2456=EDGE_CURVE('',#1876,#1878,#287,.T.);
#2457=EDGE_CURVE('',#1880,#1881,#288,.T.);
#2458=EDGE_CURVE('',#1881,#1879,#289,.T.);
#2459=EDGE_CURVE('',#1878,#1880,#290,.T.);
#2460=EDGE_CURVE('',#1882,#1883,#291,.T.);
#2461=EDGE_CURVE('',#1883,#1881,#292,.T.);
#2462=EDGE_CURVE('',#1880,#1882,#293,.T.);
#2463=EDGE_CURVE('',#1884,#1885,#294,.T.);
#2464=EDGE_CURVE('',#1885,#1883,#295,.T.);
#2465=EDGE_CURVE('',#1882,#1884,#296,.T.);
#2466=EDGE_CURVE('',#1886,#1887,#297,.T.);
#2467=EDGE_CURVE('',#1887,#1885,#298,.T.);
#2468=EDGE_CURVE('',#1884,#1886,#299,.T.);
#2469=EDGE_CURVE('',#1888,#1889,#300,.T.);
#2470=EDGE_CURVE('',#1889,#1887,#301,.T.);
#2471=EDGE_CURVE('',#1886,#1888,#302,.T.);
#2472=EDGE_CURVE('',#1890,#1891,#303,.T.);
#2473=EDGE_CURVE('',#1891,#1889,#304,.T.);
#2474=EDGE_CURVE('',#1888,#1890,#305,.T.);
#2475=EDGE_CURVE('',#1892,#1893,#306,.T.);
#2476=EDGE_CURVE('',#1893,#1891,#307,.T.);
#2477=EDGE_CURVE('',#1890,#1892,#308,.T.);
#2478=EDGE_CURVE('',#1894,#1830,#309,.T.);
#2479=EDGE_CURVE('',#1830,#1893,#310,.T.);
#2480=EDGE_CURVE('',#1892,#1894,#311,.T.);
#2481=EDGE_CURVE('',#1894,#1836,#312,.T.);
#2482=EDGE_CURVE('',#1895,#1869,#1087,.T.);
#2483=EDGE_CURVE('',#1896,#1895,#313,.T.);
#2484=EDGE_CURVE('',#1867,#1896,#1088,.T.);
#2485=EDGE_CURVE('',#1871,#1897,#1089,.T.);
#2486=EDGE_CURVE('',#1895,#1897,#314,.T.);
#2487=EDGE_CURVE('',#1898,#1873,#1090,.T.);
#2488=EDGE_CURVE('',#1897,#1898,#315,.T.);
#2489=EDGE_CURVE('',#1875,#1899,#1091,.T.);
#2490=EDGE_CURVE('',#1898,#1899,#316,.T.);
#2491=EDGE_CURVE('',#1900,#1877,#1092,.T.);
#2492=EDGE_CURVE('',#1899,#1900,#317,.T.);
#2493=EDGE_CURVE('',#1879,#1901,#1093,.T.);
#2494=EDGE_CURVE('',#1900,#1901,#318,.T.);
#2495=EDGE_CURVE('',#1902,#1881,#1094,.T.);
#2496=EDGE_CURVE('',#1901,#1902,#319,.T.);
#2497=EDGE_CURVE('',#1883,#1903,#1095,.T.);
#2498=EDGE_CURVE('',#1902,#1903,#320,.T.);
#2499=EDGE_CURVE('',#1904,#1885,#1096,.T.);
#2500=EDGE_CURVE('',#1903,#1904,#321,.T.);
#2501=EDGE_CURVE('',#1887,#1905,#1097,.T.);
#2502=EDGE_CURVE('',#1904,#1905,#322,.T.);
#2503=EDGE_CURVE('',#1906,#1889,#1098,.T.);
#2504=EDGE_CURVE('',#1905,#1906,#323,.T.);
#2505=EDGE_CURVE('',#1891,#1907,#1099,.T.);
#2506=EDGE_CURVE('',#1906,#1907,#324,.T.);
#2507=EDGE_CURVE('',#1908,#1893,#1100,.T.);
#2508=EDGE_CURVE('',#1907,#1908,#325,.T.);
#2509=EDGE_CURVE('',#1823,#1909,#1101,.T.);
#2510=EDGE_CURVE('',#1908,#1909,#326,.T.);
#2511=EDGE_CURVE('',#1909,#1829,#327,.T.);
#2512=EDGE_CURVE('',#1910,#1910,#328,.T.);
#2513=EDGE_CURVE('',#1911,#1911,#329,.T.);
#2514=EDGE_CURVE('',#1912,#1912,#330,.T.);
#2515=EDGE_CURVE('',#1913,#1913,#331,.T.);
#2516=EDGE_CURVE('',#1914,#1914,#332,.T.);
#2517=EDGE_CURVE('',#1915,#1915,#333,.T.);
#2518=EDGE_CURVE('',#1916,#1916,#334,.T.);
#2519=EDGE_CURVE('',#1917,#1917,#335,.T.);
#2520=EDGE_CURVE('',#1918,#1918,#336,.T.);
#2521=EDGE_CURVE('',#1919,#1920,#337,.T.);
#2522=EDGE_CURVE('',#1920,#1921,#338,.T.);
#2523=EDGE_CURVE('',#1921,#1922,#339,.T.);
#2524=EDGE_CURVE('',#1922,#1919,#340,.T.);
#2525=EDGE_CURVE('',#1923,#1828,#341,.T.);
#2526=EDGE_CURVE('',#1828,#1922,#342,.T.);
#2527=EDGE_CURVE('',#1921,#1923,#343,.T.);
#2528=EDGE_CURVE('',#1924,#1829,#344,.T.);
#2529=EDGE_CURVE('',#1923,#1924,#345,.T.);
#2530=EDGE_CURVE('',#1925,#1909,#346,.T.);
#2531=EDGE_CURVE('',#1924,#1925,#347,.T.);
#2532=EDGE_CURVE('',#1926,#1908,#348,.T.);
#2533=EDGE_CURVE('',#1925,#1926,#349,.T.);
#2534=EDGE_CURVE('',#1927,#1907,#350,.T.);
#2535=EDGE_CURVE('',#1926,#1927,#351,.T.);
#2536=EDGE_CURVE('',#1928,#1906,#352,.T.);
#2537=EDGE_CURVE('',#1927,#1928,#353,.T.);
#2538=EDGE_CURVE('',#1929,#1905,#354,.T.);
#2539=EDGE_CURVE('',#1928,#1929,#355,.T.);
#2540=EDGE_CURVE('',#1930,#1904,#356,.T.);
#2541=EDGE_CURVE('',#1929,#1930,#357,.T.);
#2542=EDGE_CURVE('',#1931,#1903,#358,.T.);
#2543=EDGE_CURVE('',#1930,#1931,#359,.T.);
#2544=EDGE_CURVE('',#1932,#1902,#360,.T.);
#2545=EDGE_CURVE('',#1931,#1932,#361,.T.);
#2546=EDGE_CURVE('',#1933,#1901,#362,.T.);
#2547=EDGE_CURVE('',#1932,#1933,#363,.T.);
#2548=EDGE_CURVE('',#1934,#1900,#364,.T.);
#2549=EDGE_CURVE('',#1933,#1934,#365,.T.);
#2550=EDGE_CURVE('',#1935,#1899,#366,.T.);
#2551=EDGE_CURVE('',#1934,#1935,#367,.T.);
#2552=EDGE_CURVE('',#1936,#1898,#368,.T.);
#2553=EDGE_CURVE('',#1935,#1936,#369,.T.);
#2554=EDGE_CURVE('',#1937,#1897,#370,.T.);
#2555=EDGE_CURVE('',#1936,#1937,#371,.T.);
#2556=EDGE_CURVE('',#1938,#1895,#372,.T.);
#2557=EDGE_CURVE('',#1937,#1938,#373,.T.);
#2558=EDGE_CURVE('',#1939,#1896,#374,.T.);
#2559=EDGE_CURVE('',#1938,#1939,#375,.T.);
#2560=EDGE_CURVE('',#1940,#1835,#376,.T.);
#2561=EDGE_CURVE('',#1835,#1896,#377,.T.);
#2562=EDGE_CURVE('',#1939,#1940,#378,.T.);
#2563=EDGE_CURVE('',#1941,#1831,#379,.T.);
#2564=EDGE_CURVE('',#1940,#1941,#380,.T.);
#2565=EDGE_CURVE('',#1942,#1832,#381,.T.);
#2566=EDGE_CURVE('',#1941,#1942,#382,.T.);
#2567=EDGE_CURVE('',#1943,#1944,#383,.T.);
#2568=EDGE_CURVE('',#1944,#1832,#384,.T.);
#2569=EDGE_CURVE('',#1942,#1943,#385,.T.);
#2570=EDGE_CURVE('',#1945,#1946,#386,.T.);
#2571=EDGE_CURVE('',#1946,#1944,#387,.T.);
#2572=EDGE_CURVE('',#1943,#1945,#388,.T.);
#2573=EDGE_CURVE('',#1947,#1948,#389,.T.);
#2574=EDGE_CURVE('',#1948,#1946,#390,.T.);
#2575=EDGE_CURVE('',#1945,#1947,#391,.T.);
#2576=EDGE_CURVE('',#1949,#1950,#392,.T.);
#2577=EDGE_CURVE('',#1950,#1948,#393,.T.);
#2578=EDGE_CURVE('',#1947,#1949,#394,.T.);
#2579=EDGE_CURVE('',#1951,#1952,#395,.T.);
#2580=EDGE_CURVE('',#1952,#1950,#396,.T.);
#2581=EDGE_CURVE('',#1949,#1951,#397,.T.);
#2582=EDGE_CURVE('',#1953,#1954,#398,.T.);
#2583=EDGE_CURVE('',#1954,#1952,#399,.T.);
#2584=EDGE_CURVE('',#1951,#1953,#400,.T.);
#2585=EDGE_CURVE('',#1955,#1956,#401,.T.);
#2586=EDGE_CURVE('',#1956,#1954,#402,.T.);
#2587=EDGE_CURVE('',#1953,#1955,#403,.T.);
#2588=EDGE_CURVE('',#1957,#1958,#404,.T.);
#2589=EDGE_CURVE('',#1958,#1956,#405,.T.);
#2590=EDGE_CURVE('',#1955,#1957,#406,.T.);
#2591=EDGE_CURVE('',#1959,#1960,#407,.T.);
#2592=EDGE_CURVE('',#1960,#1958,#408,.T.);
#2593=EDGE_CURVE('',#1957,#1959,#409,.T.);
#2594=EDGE_CURVE('',#1961,#1962,#410,.T.);
#2595=EDGE_CURVE('',#1962,#1960,#411,.T.);
#2596=EDGE_CURVE('',#1959,#1961,#412,.T.);
#2597=EDGE_CURVE('',#1961,#1920,#413,.T.);
#2598=EDGE_CURVE('',#1919,#1962,#414,.T.);
#2599=EDGE_CURVE('',#1817,#1865,#1102,.T.);
#2600=EDGE_CURVE('',#1861,#1944,#1103,.T.);
#2601=EDGE_CURVE('',#1946,#1859,#1104,.T.);
#2602=EDGE_CURVE('',#1857,#1948,#1105,.T.);
#2603=EDGE_CURVE('',#1950,#1855,#1106,.T.);
#2604=EDGE_CURVE('',#1853,#1952,#1107,.T.);
#2605=EDGE_CURVE('',#1954,#1851,#1108,.T.);
#2606=EDGE_CURVE('',#1849,#1956,#1109,.T.);
#2607=EDGE_CURVE('',#1958,#1847,#1110,.T.);
#2608=EDGE_CURVE('',#1845,#1960,#1111,.T.);
#2609=EDGE_CURVE('',#1962,#1843,#1112,.T.);
#2610=EDGE_CURVE('',#1841,#1919,#1113,.T.);
#2611=EDGE_CURVE('',#1922,#1839,#1114,.T.);
#2612=EDGE_CURVE('',#1963,#1963,#415,.T.);
#2613=EDGE_CURVE('',#1964,#1964,#416,.T.);
#2614=EDGE_CURVE('',#1965,#1965,#417,.T.);
#2615=EDGE_CURVE('',#1966,#1966,#418,.T.);
#2616=EDGE_CURVE('',#1967,#1967,#419,.T.);
#2617=EDGE_CURVE('',#1968,#1968,#420,.T.);
#2618=EDGE_CURVE('',#1969,#1969,#421,.T.);
#2619=EDGE_CURVE('',#1970,#1970,#422,.T.);
#2620=EDGE_CURVE('',#1971,#1971,#423,.T.);
#2621=EDGE_CURVE('',#1910,#1972,#424,.T.);
#2622=EDGE_CURVE('',#1972,#1973,#425,.T.);
#2623=EDGE_CURVE('',#1973,#1972,#426,.T.);
#2624=EDGE_CURVE('',#1973,#1974,#1115,.T.);
#2625=EDGE_CURVE('',#1975,#1974,#427,.T.);
#2626=EDGE_CURVE('',#1974,#1975,#428,.T.);
#2627=EDGE_CURVE('',#1963,#1975,#429,.T.);
#2628=EDGE_CURVE('',#1964,#1911,#1116,.T.);
#2629=EDGE_CURVE('',#1971,#1918,#1117,.T.);
#2630=EDGE_CURVE('',#1970,#1912,#1118,.T.);
#2631=EDGE_CURVE('',#1969,#1917,#1119,.T.);
#2632=EDGE_CURVE('',#1968,#1913,#1120,.T.);
#2633=EDGE_CURVE('',#1967,#1916,#1121,.T.);
#2634=EDGE_CURVE('',#1966,#1914,#1122,.T.);
#2635=EDGE_CURVE('',#1965,#1915,#1123,.T.);
#2636=EDGE_CURVE('',#1976,#1977,#43,.T.);
#2637=EDGE_CURVE('',#1978,#1976,#1124,.T.);
#2638=EDGE_CURVE('',#1979,#1978,#44,.T.);
#2639=EDGE_CURVE('',#1980,#1979,#1125,.T.);
#2640=EDGE_CURVE('',#1980,#1981,#1126,.T.);
#2641=EDGE_CURVE('',#1977,#1981,#1127,.T.);
#2642=EDGE_CURVE('',#1982,#1983,#1128,.T.);
#2643=EDGE_CURVE('',#1984,#1982,#430,.T.);
#2644=EDGE_CURVE('',#1985,#1984,#431,.T.);
#2645=EDGE_CURVE('',#1986,#1985,#1538,.F.);
#2646=EDGE_CURVE('',#1987,#1986,#432,.T.);
#2647=EDGE_CURVE('',#1983,#1987,#433,.T.);
#2648=EDGE_CURVE('',#1988,#1989,#1539,.F.);
#2649=EDGE_CURVE('',#1989,#1986,#1129,.T.);
#2650=EDGE_CURVE('',#1985,#1988,#1130,.T.);
#2651=EDGE_CURVE('',#1990,#1988,#434,.T.);
#2652=EDGE_CURVE('',#1981,#1990,#435,.T.);
#2653=EDGE_CURVE('',#1991,#1980,#436,.T.);
#2654=EDGE_CURVE('',#1989,#1991,#437,.T.);
#2655=EDGE_CURVE('',#1987,#1991,#1131,.T.);
#2656=EDGE_CURVE('',#1990,#1984,#1132,.T.);
#2657=EDGE_CURVE('',#1982,#1992,#1133,.F.);
#2658=EDGE_CURVE('',#1993,#1992,#1134,.T.);
#2659=EDGE_CURVE('',#1984,#1993,#1135,.T.);
#2660=EDGE_CURVE('',#1994,#1983,#1136,.F.);
#2661=EDGE_CURVE('',#1992,#1994,#438,.F.);
#2662=EDGE_CURVE('',#1995,#1979,#1137,.T.);
#2663=EDGE_CURVE('',#1991,#1995,#1138,.T.);
#2664=EDGE_CURVE('',#1996,#1987,#1139,.T.);
#2665=EDGE_CURVE('',#1996,#1994,#1140,.T.);
#2666=EDGE_CURVE('',#1993,#1996,#439,.T.);
#2667=EDGE_CURVE('',#1997,#1990,#1141,.T.);
#2668=EDGE_CURVE('',#1997,#1977,#1142,.T.);
#2669=EDGE_CURVE('',#1995,#1997,#440,.T.);
#2670=EDGE_CURVE('',#1978,#1976,#441,.F.);
#2671=EDGE_CURVE('',#1998,#1999,#1143,.T.);
#2672=EDGE_CURVE('',#1999,#2000,#1144,.T.);
#2673=EDGE_CURVE('',#2001,#2000,#1145,.T.);
#2674=EDGE_CURVE('',#1998,#2001,#1146,.T.);
#2675=EDGE_CURVE('',#2002,#1998,#442,.T.);
#2676=EDGE_CURVE('',#2003,#2001,#443,.T.);
#2677=EDGE_CURVE('',#2002,#2003,#1147,.T.);
#2678=EDGE_CURVE('',#2004,#2002,#1148,.T.);
#2679=EDGE_CURVE('',#2005,#2003,#1149,.T.);
#2680=EDGE_CURVE('',#2004,#2005,#1150,.T.);
#2681=EDGE_CURVE('',#1999,#2004,#444,.T.);
#2682=EDGE_CURVE('',#2000,#2005,#445,.T.);
#2683=ORIENTED_EDGE('',*,*,#2006,.F.);
#2684=ORIENTED_EDGE('',*,*,#2007,.F.);
#2685=ORIENTED_EDGE('',*,*,#2008,.T.);
#2686=ORIENTED_EDGE('',*,*,#2009,.F.);
#2687=ORIENTED_EDGE('',*,*,#2010,.F.);
#2688=ORIENTED_EDGE('',*,*,#2008,.F.);
#2689=ORIENTED_EDGE('',*,*,#2011,.F.);
#2690=ORIENTED_EDGE('',*,*,#2012,.F.);
#2691=ORIENTED_EDGE('',*,*,#2013,.T.);
#2692=ORIENTED_EDGE('',*,*,#2014,.F.);
#2693=ORIENTED_EDGE('',*,*,#2015,.F.);
#2694=ORIENTED_EDGE('',*,*,#2013,.F.);
#2695=ORIENTED_EDGE('',*,*,#2016,.T.);
#2696=ORIENTED_EDGE('',*,*,#2017,.T.);
#2697=ORIENTED_EDGE('',*,*,#2018,.T.);
#2698=ORIENTED_EDGE('',*,*,#2019,.T.);
#2699=ORIENTED_EDGE('',*,*,#2017,.F.);
#2700=ORIENTED_EDGE('',*,*,#2020,.F.);
#2701=ORIENTED_EDGE('',*,*,#2016,.F.);
#2702=ORIENTED_EDGE('',*,*,#2021,.F.);
#2703=ORIENTED_EDGE('',*,*,#2022,.F.);
#2704=ORIENTED_EDGE('',*,*,#2023,.T.);
#2705=ORIENTED_EDGE('',*,*,#2018,.F.);
#2706=ORIENTED_EDGE('',*,*,#2019,.F.);
#2707=ORIENTED_EDGE('',*,*,#2023,.F.);
#2708=ORIENTED_EDGE('',*,*,#2011,.T.);
#2709=ORIENTED_EDGE('',*,*,#2012,.T.);
#2710=ORIENTED_EDGE('',*,*,#2009,.T.);
#2711=ORIENTED_EDGE('',*,*,#2010,.T.);
#2712=ORIENTED_EDGE('',*,*,#2020,.T.);
#2713=ORIENTED_EDGE('',*,*,#2024,.T.);
#2714=ORIENTED_EDGE('',*,*,#2025,.T.);
#2715=ORIENTED_EDGE('',*,*,#2026,.T.);
#2716=ORIENTED_EDGE('',*,*,#2024,.F.);
#2717=ORIENTED_EDGE('',*,*,#2026,.F.);
#2718=ORIENTED_EDGE('',*,*,#2027,.T.);
#2719=ORIENTED_EDGE('',*,*,#2028,.F.);
#2720=ORIENTED_EDGE('',*,*,#2029,.F.);
#2721=ORIENTED_EDGE('',*,*,#2027,.F.);
#2722=ORIENTED_EDGE('',*,*,#2025,.F.);
#2723=ORIENTED_EDGE('',*,*,#2014,.T.);
#2724=ORIENTED_EDGE('',*,*,#2015,.T.);
#2725=ORIENTED_EDGE('',*,*,#2006,.T.);
#2726=ORIENTED_EDGE('',*,*,#2007,.T.);
#2727=ORIENTED_EDGE('',*,*,#2030,.T.);
#2728=ORIENTED_EDGE('',*,*,#2031,.T.);
#2729=ORIENTED_EDGE('',*,*,#2028,.T.);
#2730=ORIENTED_EDGE('',*,*,#2029,.T.);
#2731=ORIENTED_EDGE('',*,*,#2031,.F.);
#2732=ORIENTED_EDGE('',*,*,#2030,.F.);
#2733=ORIENTED_EDGE('',*,*,#2032,.F.);
#2734=ORIENTED_EDGE('',*,*,#2032,.T.);
#2735=ORIENTED_EDGE('',*,*,#2033,.T.);
#2736=ORIENTED_EDGE('',*,*,#2021,.T.);
#2737=ORIENTED_EDGE('',*,*,#2022,.T.);
#2738=ORIENTED_EDGE('',*,*,#2033,.F.);
#2739=ORIENTED_EDGE('',*,*,#2034,.F.);
#2740=ORIENTED_EDGE('',*,*,#2035,.T.);
#2741=ORIENTED_EDGE('',*,*,#2036,.F.);
#2742=ORIENTED_EDGE('',*,*,#2035,.F.);
#2743=ORIENTED_EDGE('',*,*,#2036,.T.);
#2744=ORIENTED_EDGE('',*,*,#2034,.T.);
#2745=ORIENTED_EDGE('',*,*,#2037,.T.);
#2746=ORIENTED_EDGE('',*,*,#2038,.T.);
#2747=ORIENTED_EDGE('',*,*,#2039,.F.);
#2748=ORIENTED_EDGE('',*,*,#2038,.F.);
#2749=ORIENTED_EDGE('',*,*,#2040,.F.);
#2750=ORIENTED_EDGE('',*,*,#2041,.T.);
#2751=ORIENTED_EDGE('',*,*,#2042,.T.);
#2752=ORIENTED_EDGE('',*,*,#2041,.F.);
#2753=ORIENTED_EDGE('',*,*,#2040,.T.);
#2754=ORIENTED_EDGE('',*,*,#2039,.T.);
#2755=ORIENTED_EDGE('',*,*,#2042,.F.);
#2756=ORIENTED_EDGE('',*,*,#2037,.F.);
#2757=ORIENTED_EDGE('',*,*,#2043,.T.);
#2758=ORIENTED_EDGE('',*,*,#2044,.T.);
#2759=ORIENTED_EDGE('',*,*,#2045,.F.);
#2760=ORIENTED_EDGE('',*,*,#2046,.F.);
#2761=ORIENTED_EDGE('',*,*,#2047,.T.);
#2762=ORIENTED_EDGE('',*,*,#2048,.T.);
#2763=ORIENTED_EDGE('',*,*,#2049,.T.);
#2764=ORIENTED_EDGE('',*,*,#2043,.F.);
#2765=ORIENTED_EDGE('',*,*,#2050,.F.);
#2766=ORIENTED_EDGE('',*,*,#2051,.F.);
#2767=ORIENTED_EDGE('',*,*,#2052,.T.);
#2768=ORIENTED_EDGE('',*,*,#2053,.T.);
#2769=ORIENTED_EDGE('',*,*,#2054,.T.);
#2770=ORIENTED_EDGE('',*,*,#2047,.F.);
#2771=ORIENTED_EDGE('',*,*,#2055,.F.);
#2772=ORIENTED_EDGE('',*,*,#2056,.F.);
#2773=ORIENTED_EDGE('',*,*,#2057,.T.);
#2774=ORIENTED_EDGE('',*,*,#2058,.T.);
#2775=ORIENTED_EDGE('',*,*,#2059,.T.);
#2776=ORIENTED_EDGE('',*,*,#2052,.F.);
#2777=ORIENTED_EDGE('',*,*,#2060,.F.);
#2778=ORIENTED_EDGE('',*,*,#2061,.F.);
#2779=ORIENTED_EDGE('',*,*,#2062,.T.);
#2780=ORIENTED_EDGE('',*,*,#2063,.T.);
#2781=ORIENTED_EDGE('',*,*,#2064,.T.);
#2782=ORIENTED_EDGE('',*,*,#2057,.F.);
#2783=ORIENTED_EDGE('',*,*,#2065,.F.);
#2784=ORIENTED_EDGE('',*,*,#2066,.F.);
#2785=ORIENTED_EDGE('',*,*,#2067,.T.);
#2786=ORIENTED_EDGE('',*,*,#2068,.T.);
#2787=ORIENTED_EDGE('',*,*,#2069,.T.);
#2788=ORIENTED_EDGE('',*,*,#2062,.F.);
#2789=ORIENTED_EDGE('',*,*,#2070,.F.);
#2790=ORIENTED_EDGE('',*,*,#2071,.F.);
#2791=ORIENTED_EDGE('',*,*,#2072,.T.);
#2792=ORIENTED_EDGE('',*,*,#2073,.T.);
#2793=ORIENTED_EDGE('',*,*,#2074,.T.);
#2794=ORIENTED_EDGE('',*,*,#2067,.F.);
#2795=ORIENTED_EDGE('',*,*,#2075,.F.);
#2796=ORIENTED_EDGE('',*,*,#2076,.F.);
#2797=ORIENTED_EDGE('',*,*,#2077,.F.);
#2798=ORIENTED_EDGE('',*,*,#2078,.F.);
#2799=ORIENTED_EDGE('',*,*,#2079,.F.);
#2800=ORIENTED_EDGE('',*,*,#2080,.F.);
#2801=ORIENTED_EDGE('',*,*,#2081,.T.);
#2802=ORIENTED_EDGE('',*,*,#2082,.T.);
#2803=ORIENTED_EDGE('',*,*,#2083,.T.);
#2804=ORIENTED_EDGE('',*,*,#2084,.T.);
#2805=ORIENTED_EDGE('',*,*,#2085,.T.);
#2806=ORIENTED_EDGE('',*,*,#2086,.F.);
#2807=ORIENTED_EDGE('',*,*,#2087,.T.);
#2808=ORIENTED_EDGE('',*,*,#2088,.T.);
#2809=ORIENTED_EDGE('',*,*,#2089,.T.);
#2810=ORIENTED_EDGE('',*,*,#2090,.T.);
#2811=ORIENTED_EDGE('',*,*,#2091,.T.);
#2812=ORIENTED_EDGE('',*,*,#2083,.F.);
#2813=ORIENTED_EDGE('',*,*,#2092,.T.);
#2814=ORIENTED_EDGE('',*,*,#2093,.T.);
#2815=ORIENTED_EDGE('',*,*,#2094,.T.);
#2816=ORIENTED_EDGE('',*,*,#2095,.T.);
#2817=ORIENTED_EDGE('',*,*,#2096,.T.);
#2818=ORIENTED_EDGE('',*,*,#2089,.F.);
#2819=ORIENTED_EDGE('',*,*,#2097,.T.);
#2820=ORIENTED_EDGE('',*,*,#2098,.T.);
#2821=ORIENTED_EDGE('',*,*,#2099,.T.);
#2822=ORIENTED_EDGE('',*,*,#2100,.T.);
#2823=ORIENTED_EDGE('',*,*,#2094,.F.);
#2824=ORIENTED_EDGE('',*,*,#2101,.T.);
#2825=ORIENTED_EDGE('',*,*,#2102,.T.);
#2826=ORIENTED_EDGE('',*,*,#2103,.T.);
#2827=ORIENTED_EDGE('',*,*,#2104,.T.);
#2828=ORIENTED_EDGE('',*,*,#2105,.T.);
#2829=ORIENTED_EDGE('',*,*,#2099,.F.);
#2830=ORIENTED_EDGE('',*,*,#2106,.T.);
#2831=ORIENTED_EDGE('',*,*,#2107,.T.);
#2832=ORIENTED_EDGE('',*,*,#2108,.T.);
#2833=ORIENTED_EDGE('',*,*,#2109,.T.);
#2834=ORIENTED_EDGE('',*,*,#2103,.F.);
#2835=ORIENTED_EDGE('',*,*,#2110,.T.);
#2836=ORIENTED_EDGE('',*,*,#2111,.T.);
#2837=ORIENTED_EDGE('',*,*,#2112,.T.);
#2838=ORIENTED_EDGE('',*,*,#2113,.T.);
#2839=ORIENTED_EDGE('',*,*,#2114,.T.);
#2840=ORIENTED_EDGE('',*,*,#2108,.F.);
#2841=ORIENTED_EDGE('',*,*,#2115,.T.);
#2842=ORIENTED_EDGE('',*,*,#2116,.T.);
#2843=ORIENTED_EDGE('',*,*,#2117,.T.);
#2844=ORIENTED_EDGE('',*,*,#2118,.T.);
#2845=ORIENTED_EDGE('',*,*,#2119,.T.);
#2846=ORIENTED_EDGE('',*,*,#2120,.T.);
#2847=ORIENTED_EDGE('',*,*,#2121,.F.);
#2848=ORIENTED_EDGE('',*,*,#2122,.T.);
#2849=ORIENTED_EDGE('',*,*,#2123,.T.);
#2850=ORIENTED_EDGE('',*,*,#2118,.F.);
#2851=ORIENTED_EDGE('',*,*,#2121,.T.);
#2852=ORIENTED_EDGE('',*,*,#2124,.T.);
#2853=ORIENTED_EDGE('',*,*,#2112,.F.);
#2854=ORIENTED_EDGE('',*,*,#2125,.T.);
#2855=ORIENTED_EDGE('',*,*,#2126,.T.);
#2856=ORIENTED_EDGE('',*,*,#2077,.T.);
#2857=ORIENTED_EDGE('',*,*,#2127,.T.);
#2858=ORIENTED_EDGE('',*,*,#2128,.T.);
#2859=ORIENTED_EDGE('',*,*,#2072,.F.);
#2860=ORIENTED_EDGE('',*,*,#2129,.F.);
#2861=ORIENTED_EDGE('',*,*,#2130,.F.);
#2862=ORIENTED_EDGE('',*,*,#2131,.F.);
#2863=ORIENTED_EDGE('',*,*,#2044,.F.);
#2864=ORIENTED_EDGE('',*,*,#2049,.F.);
#2865=ORIENTED_EDGE('',*,*,#2048,.F.);
#2866=ORIENTED_EDGE('',*,*,#2054,.F.);
#2867=ORIENTED_EDGE('',*,*,#2053,.F.);
#2868=ORIENTED_EDGE('',*,*,#2059,.F.);
#2869=ORIENTED_EDGE('',*,*,#2058,.F.);
#2870=ORIENTED_EDGE('',*,*,#2064,.F.);
#2871=ORIENTED_EDGE('',*,*,#2063,.F.);
#2872=ORIENTED_EDGE('',*,*,#2069,.F.);
#2873=ORIENTED_EDGE('',*,*,#2068,.F.);
#2874=ORIENTED_EDGE('',*,*,#2074,.F.);
#2875=ORIENTED_EDGE('',*,*,#2073,.F.);
#2876=ORIENTED_EDGE('',*,*,#2128,.F.);
#2877=ORIENTED_EDGE('',*,*,#2127,.F.);
#2878=ORIENTED_EDGE('',*,*,#2082,.F.);
#2879=ORIENTED_EDGE('',*,*,#2081,.F.);
#2880=ORIENTED_EDGE('',*,*,#2132,.F.);
#2881=ORIENTED_EDGE('',*,*,#2122,.F.);
#2882=ORIENTED_EDGE('',*,*,#2126,.F.);
#2883=ORIENTED_EDGE('',*,*,#2125,.F.);
#2884=ORIENTED_EDGE('',*,*,#2116,.F.);
#2885=ORIENTED_EDGE('',*,*,#2115,.F.);
#2886=ORIENTED_EDGE('',*,*,#2111,.F.);
#2887=ORIENTED_EDGE('',*,*,#2110,.F.);
#2888=ORIENTED_EDGE('',*,*,#2107,.F.);
#2889=ORIENTED_EDGE('',*,*,#2106,.F.);
#2890=ORIENTED_EDGE('',*,*,#2102,.F.);
#2891=ORIENTED_EDGE('',*,*,#2101,.F.);
#2892=ORIENTED_EDGE('',*,*,#2098,.F.);
#2893=ORIENTED_EDGE('',*,*,#2097,.F.);
#2894=ORIENTED_EDGE('',*,*,#2093,.F.);
#2895=ORIENTED_EDGE('',*,*,#2092,.F.);
#2896=ORIENTED_EDGE('',*,*,#2088,.F.);
#2897=ORIENTED_EDGE('',*,*,#2087,.F.);
#2898=ORIENTED_EDGE('',*,*,#2080,.T.);
#2899=ORIENTED_EDGE('',*,*,#2133,.T.);
#2900=ORIENTED_EDGE('',*,*,#2119,.F.);
#2901=ORIENTED_EDGE('',*,*,#2123,.F.);
#2902=ORIENTED_EDGE('',*,*,#2132,.T.);
#2903=ORIENTED_EDGE('',*,*,#2134,.F.);
#2904=ORIENTED_EDGE('',*,*,#2085,.F.);
#2905=ORIENTED_EDGE('',*,*,#2084,.F.);
#2906=ORIENTED_EDGE('',*,*,#2091,.F.);
#2907=ORIENTED_EDGE('',*,*,#2090,.F.);
#2908=ORIENTED_EDGE('',*,*,#2096,.F.);
#2909=ORIENTED_EDGE('',*,*,#2095,.F.);
#2910=ORIENTED_EDGE('',*,*,#2100,.F.);
#2911=ORIENTED_EDGE('',*,*,#2105,.F.);
#2912=ORIENTED_EDGE('',*,*,#2104,.F.);
#2913=ORIENTED_EDGE('',*,*,#2109,.F.);
#2914=ORIENTED_EDGE('',*,*,#2114,.F.);
#2915=ORIENTED_EDGE('',*,*,#2113,.F.);
#2916=ORIENTED_EDGE('',*,*,#2124,.F.);
#2917=ORIENTED_EDGE('',*,*,#2120,.F.);
#2918=ORIENTED_EDGE('',*,*,#2133,.F.);
#2919=ORIENTED_EDGE('',*,*,#2079,.T.);
#2920=ORIENTED_EDGE('',*,*,#2078,.T.);
#2921=ORIENTED_EDGE('',*,*,#2130,.T.);
#2922=ORIENTED_EDGE('',*,*,#2129,.T.);
#2923=ORIENTED_EDGE('',*,*,#2076,.T.);
#2924=ORIENTED_EDGE('',*,*,#2075,.T.);
#2925=ORIENTED_EDGE('',*,*,#2071,.T.);
#2926=ORIENTED_EDGE('',*,*,#2070,.T.);
#2927=ORIENTED_EDGE('',*,*,#2066,.T.);
#2928=ORIENTED_EDGE('',*,*,#2065,.T.);
#2929=ORIENTED_EDGE('',*,*,#2061,.T.);
#2930=ORIENTED_EDGE('',*,*,#2060,.T.);
#2931=ORIENTED_EDGE('',*,*,#2056,.T.);
#2932=ORIENTED_EDGE('',*,*,#2055,.T.);
#2933=ORIENTED_EDGE('',*,*,#2051,.T.);
#2934=ORIENTED_EDGE('',*,*,#2050,.T.);
#2935=ORIENTED_EDGE('',*,*,#2046,.T.);
#2936=ORIENTED_EDGE('',*,*,#2135,.F.);
#2937=ORIENTED_EDGE('',*,*,#2136,.T.);
#2938=ORIENTED_EDGE('',*,*,#2137,.F.);
#2939=ORIENTED_EDGE('',*,*,#2136,.F.);
#2940=ORIENTED_EDGE('',*,*,#2135,.T.);
#2941=ORIENTED_EDGE('',*,*,#2138,.F.);
#2942=ORIENTED_EDGE('',*,*,#2139,.F.);
#2943=ORIENTED_EDGE('',*,*,#2117,.F.);
#2944=ORIENTED_EDGE('',*,*,#2138,.T.);
#2945=ORIENTED_EDGE('',*,*,#2140,.T.);
#2946=ORIENTED_EDGE('',*,*,#2139,.T.);
#2947=ORIENTED_EDGE('',*,*,#2140,.F.);
#2948=ORIENTED_EDGE('',*,*,#2137,.T.);
#2949=ORIENTED_EDGE('',*,*,#2131,.T.);
#2950=ORIENTED_EDGE('',*,*,#2086,.T.);
#2951=ORIENTED_EDGE('',*,*,#2134,.T.);
#2952=ORIENTED_EDGE('',*,*,#2045,.T.);
#2953=ORIENTED_EDGE('',*,*,#2141,.F.);
#2954=ORIENTED_EDGE('',*,*,#2142,.F.);
#2955=ORIENTED_EDGE('',*,*,#2143,.F.);
#2956=ORIENTED_EDGE('',*,*,#2144,.T.);
#2957=ORIENTED_EDGE('',*,*,#2145,.F.);
#2958=ORIENTED_EDGE('',*,*,#2146,.F.);
#2959=ORIENTED_EDGE('',*,*,#2141,.T.);
#2960=ORIENTED_EDGE('',*,*,#2147,.T.);
#2961=ORIENTED_EDGE('',*,*,#2148,.F.);
#2962=ORIENTED_EDGE('',*,*,#2149,.F.);
#2963=ORIENTED_EDGE('',*,*,#2145,.T.);
#2964=ORIENTED_EDGE('',*,*,#2150,.T.);
#2965=ORIENTED_EDGE('',*,*,#2151,.F.);
#2966=ORIENTED_EDGE('',*,*,#2152,.F.);
#2967=ORIENTED_EDGE('',*,*,#2148,.T.);
#2968=ORIENTED_EDGE('',*,*,#2153,.T.);
#2969=ORIENTED_EDGE('',*,*,#2154,.F.);
#2970=ORIENTED_EDGE('',*,*,#2155,.F.);
#2971=ORIENTED_EDGE('',*,*,#2151,.T.);
#2972=ORIENTED_EDGE('',*,*,#2156,.T.);
#2973=ORIENTED_EDGE('',*,*,#2157,.F.);
#2974=ORIENTED_EDGE('',*,*,#2158,.F.);
#2975=ORIENTED_EDGE('',*,*,#2154,.T.);
#2976=ORIENTED_EDGE('',*,*,#2159,.T.);
#2977=ORIENTED_EDGE('',*,*,#2160,.T.);
#2978=ORIENTED_EDGE('',*,*,#2161,.F.);
#2979=ORIENTED_EDGE('',*,*,#2162,.T.);
#2980=ORIENTED_EDGE('',*,*,#2163,.T.);
#2981=ORIENTED_EDGE('',*,*,#2164,.T.);
#2982=ORIENTED_EDGE('',*,*,#2165,.T.);
#2983=ORIENTED_EDGE('',*,*,#2166,.T.);
#2984=ORIENTED_EDGE('',*,*,#2167,.T.);
#2985=ORIENTED_EDGE('',*,*,#2168,.T.);
#2986=ORIENTED_EDGE('',*,*,#2169,.T.);
#2987=ORIENTED_EDGE('',*,*,#2170,.F.);
#2988=ORIENTED_EDGE('',*,*,#2171,.T.);
#2989=ORIENTED_EDGE('',*,*,#2172,.T.);
#2990=ORIENTED_EDGE('',*,*,#2173,.T.);
#2991=ORIENTED_EDGE('',*,*,#2174,.T.);
#2992=ORIENTED_EDGE('',*,*,#2175,.T.);
#2993=ORIENTED_EDGE('',*,*,#2176,.T.);
#2994=ORIENTED_EDGE('',*,*,#2177,.T.);
#2995=ORIENTED_EDGE('',*,*,#2157,.T.);
#2996=ORIENTED_EDGE('',*,*,#2178,.T.);
#2997=ORIENTED_EDGE('',*,*,#2179,.F.);
#2998=ORIENTED_EDGE('',*,*,#2180,.F.);
#2999=ORIENTED_EDGE('',*,*,#2181,.T.);
#3000=ORIENTED_EDGE('',*,*,#2182,.T.);
#3001=ORIENTED_EDGE('',*,*,#2183,.T.);
#3002=ORIENTED_EDGE('',*,*,#2184,.T.);
#3003=ORIENTED_EDGE('',*,*,#2183,.F.);
#3004=ORIENTED_EDGE('',*,*,#2185,.F.);
#3005=ORIENTED_EDGE('',*,*,#2186,.F.);
#3006=ORIENTED_EDGE('',*,*,#2187,.F.);
#3007=ORIENTED_EDGE('',*,*,#2181,.F.);
#3008=ORIENTED_EDGE('',*,*,#2184,.F.);
#3009=ORIENTED_EDGE('',*,*,#2188,.F.);
#3010=ORIENTED_EDGE('',*,*,#2189,.T.);
#3011=ORIENTED_EDGE('',*,*,#2190,.T.);
#3012=ORIENTED_EDGE('',*,*,#2185,.T.);
#3013=ORIENTED_EDGE('',*,*,#2182,.F.);
#3014=ORIENTED_EDGE('',*,*,#2187,.T.);
#3015=ORIENTED_EDGE('',*,*,#2191,.T.);
#3016=ORIENTED_EDGE('',*,*,#2192,.T.);
#3017=ORIENTED_EDGE('',*,*,#2193,.F.);
#3018=ORIENTED_EDGE('',*,*,#2194,.T.);
#3019=ORIENTED_EDGE('',*,*,#2195,.T.);
#3020=ORIENTED_EDGE('',*,*,#2194,.F.);
#3021=ORIENTED_EDGE('',*,*,#2196,.T.);
#3022=ORIENTED_EDGE('',*,*,#2188,.T.);
#3023=ORIENTED_EDGE('',*,*,#2193,.T.);
#3024=ORIENTED_EDGE('',*,*,#2197,.T.);
#3025=ORIENTED_EDGE('',*,*,#2198,.T.);
#3026=ORIENTED_EDGE('',*,*,#2197,.F.);
#3027=ORIENTED_EDGE('',*,*,#2192,.F.);
#3028=ORIENTED_EDGE('',*,*,#2199,.F.);
#3029=ORIENTED_EDGE('',*,*,#2189,.F.);
#3030=ORIENTED_EDGE('',*,*,#2196,.F.);
#3031=ORIENTED_EDGE('',*,*,#2198,.F.);
#3032=ORIENTED_EDGE('',*,*,#2191,.F.);
#3033=ORIENTED_EDGE('',*,*,#2186,.T.);
#3034=ORIENTED_EDGE('',*,*,#2190,.F.);
#3035=ORIENTED_EDGE('',*,*,#2199,.T.);
#3036=ORIENTED_EDGE('',*,*,#2200,.F.);
#3037=ORIENTED_EDGE('',*,*,#2169,.F.);
#3038=ORIENTED_EDGE('',*,*,#2168,.F.);
#3039=ORIENTED_EDGE('',*,*,#2167,.F.);
#3040=ORIENTED_EDGE('',*,*,#2166,.F.);
#3041=ORIENTED_EDGE('',*,*,#2165,.F.);
#3042=ORIENTED_EDGE('',*,*,#2164,.F.);
#3043=ORIENTED_EDGE('',*,*,#2163,.F.);
#3044=ORIENTED_EDGE('',*,*,#2162,.F.);
#3045=ORIENTED_EDGE('',*,*,#2201,.F.);
#3046=ORIENTED_EDGE('',*,*,#2202,.T.);
#3047=ORIENTED_EDGE('',*,*,#2142,.T.);
#3048=ORIENTED_EDGE('',*,*,#2146,.T.);
#3049=ORIENTED_EDGE('',*,*,#2149,.T.);
#3050=ORIENTED_EDGE('',*,*,#2152,.T.);
#3051=ORIENTED_EDGE('',*,*,#2155,.T.);
#3052=ORIENTED_EDGE('',*,*,#2158,.T.);
#3053=ORIENTED_EDGE('',*,*,#2180,.T.);
#3054=ORIENTED_EDGE('',*,*,#2203,.F.);
#3055=ORIENTED_EDGE('',*,*,#2204,.F.);
#3056=ORIENTED_EDGE('',*,*,#2178,.F.);
#3057=ORIENTED_EDGE('',*,*,#2159,.F.);
#3058=ORIENTED_EDGE('',*,*,#2156,.F.);
#3059=ORIENTED_EDGE('',*,*,#2153,.F.);
#3060=ORIENTED_EDGE('',*,*,#2150,.F.);
#3061=ORIENTED_EDGE('',*,*,#2147,.F.);
#3062=ORIENTED_EDGE('',*,*,#2144,.F.);
#3063=ORIENTED_EDGE('',*,*,#2205,.F.);
#3064=ORIENTED_EDGE('',*,*,#2160,.F.);
#3065=ORIENTED_EDGE('',*,*,#2177,.F.);
#3066=ORIENTED_EDGE('',*,*,#2176,.F.);
#3067=ORIENTED_EDGE('',*,*,#2175,.F.);
#3068=ORIENTED_EDGE('',*,*,#2174,.F.);
#3069=ORIENTED_EDGE('',*,*,#2173,.F.);
#3070=ORIENTED_EDGE('',*,*,#2172,.F.);
#3071=ORIENTED_EDGE('',*,*,#2171,.F.);
#3072=ORIENTED_EDGE('',*,*,#2200,.T.);
#3073=ORIENTED_EDGE('',*,*,#2179,.T.);
#3074=ORIENTED_EDGE('',*,*,#2204,.T.);
#3075=ORIENTED_EDGE('',*,*,#2203,.T.);
#3076=ORIENTED_EDGE('',*,*,#2170,.T.);
#3077=ORIENTED_EDGE('',*,*,#2195,.F.);
#3078=ORIENTED_EDGE('',*,*,#2201,.T.);
#3079=ORIENTED_EDGE('',*,*,#2161,.T.);
#3080=ORIENTED_EDGE('',*,*,#2205,.T.);
#3081=ORIENTED_EDGE('',*,*,#2143,.T.);
#3082=ORIENTED_EDGE('',*,*,#2202,.F.);
#3083=ORIENTED_EDGE('',*,*,#2206,.F.);
#3084=ORIENTED_EDGE('',*,*,#2207,.F.);
#3085=ORIENTED_EDGE('',*,*,#2208,.F.);
#3086=ORIENTED_EDGE('',*,*,#2209,.T.);
#3087=ORIENTED_EDGE('',*,*,#2210,.F.);
#3088=ORIENTED_EDGE('',*,*,#2211,.F.);
#3089=ORIENTED_EDGE('',*,*,#2206,.T.);
#3090=ORIENTED_EDGE('',*,*,#2212,.T.);
#3091=ORIENTED_EDGE('',*,*,#2213,.T.);
#3092=ORIENTED_EDGE('',*,*,#2214,.F.);
#3093=ORIENTED_EDGE('',*,*,#2215,.F.);
#3094=ORIENTED_EDGE('',*,*,#2216,.F.);
#3095=ORIENTED_EDGE('',*,*,#2210,.T.);
#3096=ORIENTED_EDGE('',*,*,#2217,.T.);
#3097=ORIENTED_EDGE('',*,*,#2218,.T.);
#3098=ORIENTED_EDGE('',*,*,#2219,.F.);
#3099=ORIENTED_EDGE('',*,*,#2220,.F.);
#3100=ORIENTED_EDGE('',*,*,#2214,.T.);
#3101=ORIENTED_EDGE('',*,*,#2221,.T.);
#3102=ORIENTED_EDGE('',*,*,#2222,.F.);
#3103=ORIENTED_EDGE('',*,*,#2223,.F.);
#3104=ORIENTED_EDGE('',*,*,#2224,.F.);
#3105=ORIENTED_EDGE('',*,*,#2219,.T.);
#3106=ORIENTED_EDGE('',*,*,#2225,.T.);
#3107=ORIENTED_EDGE('',*,*,#2226,.T.);
#3108=ORIENTED_EDGE('',*,*,#2227,.F.);
#3109=ORIENTED_EDGE('',*,*,#2228,.F.);
#3110=ORIENTED_EDGE('',*,*,#2222,.T.);
#3111=ORIENTED_EDGE('',*,*,#2229,.T.);
#3112=ORIENTED_EDGE('',*,*,#2230,.F.);
#3113=ORIENTED_EDGE('',*,*,#2231,.F.);
#3114=ORIENTED_EDGE('',*,*,#2232,.F.);
#3115=ORIENTED_EDGE('',*,*,#2227,.T.);
#3116=ORIENTED_EDGE('',*,*,#2233,.T.);
#3117=ORIENTED_EDGE('',*,*,#2234,.T.);
#3118=ORIENTED_EDGE('',*,*,#2235,.F.);
#3119=ORIENTED_EDGE('',*,*,#2236,.F.);
#3120=ORIENTED_EDGE('',*,*,#2230,.T.);
#3121=ORIENTED_EDGE('',*,*,#2237,.T.);
#3122=ORIENTED_EDGE('',*,*,#2238,.T.);
#3123=ORIENTED_EDGE('',*,*,#2239,.T.);
#3124=ORIENTED_EDGE('',*,*,#2240,.F.);
#3125=ORIENTED_EDGE('',*,*,#2241,.T.);
#3126=ORIENTED_EDGE('',*,*,#2242,.T.);
#3127=ORIENTED_EDGE('',*,*,#2243,.T.);
#3128=ORIENTED_EDGE('',*,*,#2244,.T.);
#3129=ORIENTED_EDGE('',*,*,#2245,.T.);
#3130=ORIENTED_EDGE('',*,*,#2246,.T.);
#3131=ORIENTED_EDGE('',*,*,#2247,.T.);
#3132=ORIENTED_EDGE('',*,*,#2248,.T.);
#3133=ORIENTED_EDGE('',*,*,#2249,.T.);
#3134=ORIENTED_EDGE('',*,*,#2250,.T.);
#3135=ORIENTED_EDGE('',*,*,#2251,.F.);
#3136=ORIENTED_EDGE('',*,*,#2252,.T.);
#3137=ORIENTED_EDGE('',*,*,#2253,.T.);
#3138=ORIENTED_EDGE('',*,*,#2254,.T.);
#3139=ORIENTED_EDGE('',*,*,#2255,.T.);
#3140=ORIENTED_EDGE('',*,*,#2256,.T.);
#3141=ORIENTED_EDGE('',*,*,#2257,.T.);
#3142=ORIENTED_EDGE('',*,*,#2258,.T.);
#3143=ORIENTED_EDGE('',*,*,#2259,.T.);
#3144=ORIENTED_EDGE('',*,*,#2235,.T.);
#3145=ORIENTED_EDGE('',*,*,#2260,.T.);
#3146=ORIENTED_EDGE('',*,*,#2261,.F.);
#3147=ORIENTED_EDGE('',*,*,#2262,.F.);
#3148=ORIENTED_EDGE('',*,*,#2263,.F.);
#3149=ORIENTED_EDGE('',*,*,#2264,.T.);
#3150=ORIENTED_EDGE('',*,*,#2265,.T.);
#3151=ORIENTED_EDGE('',*,*,#2266,.T.);
#3152=ORIENTED_EDGE('',*,*,#2267,.T.);
#3153=ORIENTED_EDGE('',*,*,#2266,.F.);
#3154=ORIENTED_EDGE('',*,*,#2268,.F.);
#3155=ORIENTED_EDGE('',*,*,#2269,.F.);
#3156=ORIENTED_EDGE('',*,*,#2270,.F.);
#3157=ORIENTED_EDGE('',*,*,#2264,.F.);
#3158=ORIENTED_EDGE('',*,*,#2267,.F.);
#3159=ORIENTED_EDGE('',*,*,#2271,.F.);
#3160=ORIENTED_EDGE('',*,*,#2272,.T.);
#3161=ORIENTED_EDGE('',*,*,#2273,.T.);
#3162=ORIENTED_EDGE('',*,*,#2268,.T.);
#3163=ORIENTED_EDGE('',*,*,#2265,.F.);
#3164=ORIENTED_EDGE('',*,*,#2270,.T.);
#3165=ORIENTED_EDGE('',*,*,#2274,.T.);
#3166=ORIENTED_EDGE('',*,*,#2275,.T.);
#3167=ORIENTED_EDGE('',*,*,#2276,.F.);
#3168=ORIENTED_EDGE('',*,*,#2277,.T.);
#3169=ORIENTED_EDGE('',*,*,#2278,.T.);
#3170=ORIENTED_EDGE('',*,*,#2277,.F.);
#3171=ORIENTED_EDGE('',*,*,#2279,.T.);
#3172=ORIENTED_EDGE('',*,*,#2271,.T.);
#3173=ORIENTED_EDGE('',*,*,#2276,.T.);
#3174=ORIENTED_EDGE('',*,*,#2280,.T.);
#3175=ORIENTED_EDGE('',*,*,#2281,.T.);
#3176=ORIENTED_EDGE('',*,*,#2273,.F.);
#3177=ORIENTED_EDGE('',*,*,#2282,.T.);
#3178=ORIENTED_EDGE('',*,*,#2274,.F.);
#3179=ORIENTED_EDGE('',*,*,#2269,.T.);
#3180=ORIENTED_EDGE('',*,*,#2280,.F.);
#3181=ORIENTED_EDGE('',*,*,#2275,.F.);
#3182=ORIENTED_EDGE('',*,*,#2282,.F.);
#3183=ORIENTED_EDGE('',*,*,#2272,.F.);
#3184=ORIENTED_EDGE('',*,*,#2279,.F.);
#3185=ORIENTED_EDGE('',*,*,#2281,.F.);
#3186=ORIENTED_EDGE('',*,*,#2283,.F.);
#3187=ORIENTED_EDGE('',*,*,#2250,.F.);
#3188=ORIENTED_EDGE('',*,*,#2249,.F.);
#3189=ORIENTED_EDGE('',*,*,#2248,.F.);
#3190=ORIENTED_EDGE('',*,*,#2247,.F.);
#3191=ORIENTED_EDGE('',*,*,#2246,.F.);
#3192=ORIENTED_EDGE('',*,*,#2245,.F.);
#3193=ORIENTED_EDGE('',*,*,#2244,.F.);
#3194=ORIENTED_EDGE('',*,*,#2243,.F.);
#3195=ORIENTED_EDGE('',*,*,#2242,.F.);
#3196=ORIENTED_EDGE('',*,*,#2241,.F.);
#3197=ORIENTED_EDGE('',*,*,#2284,.F.);
#3198=ORIENTED_EDGE('',*,*,#2285,.T.);
#3199=ORIENTED_EDGE('',*,*,#2207,.T.);
#3200=ORIENTED_EDGE('',*,*,#2211,.T.);
#3201=ORIENTED_EDGE('',*,*,#2216,.T.);
#3202=ORIENTED_EDGE('',*,*,#2215,.T.);
#3203=ORIENTED_EDGE('',*,*,#2220,.T.);
#3204=ORIENTED_EDGE('',*,*,#2224,.T.);
#3205=ORIENTED_EDGE('',*,*,#2223,.T.);
#3206=ORIENTED_EDGE('',*,*,#2228,.T.);
#3207=ORIENTED_EDGE('',*,*,#2232,.T.);
#3208=ORIENTED_EDGE('',*,*,#2231,.T.);
#3209=ORIENTED_EDGE('',*,*,#2236,.T.);
#3210=ORIENTED_EDGE('',*,*,#2263,.T.);
#3211=ORIENTED_EDGE('',*,*,#2262,.T.);
#3212=ORIENTED_EDGE('',*,*,#2286,.F.);
#3213=ORIENTED_EDGE('',*,*,#2287,.F.);
#3214=ORIENTED_EDGE('',*,*,#2260,.F.);
#3215=ORIENTED_EDGE('',*,*,#2238,.F.);
#3216=ORIENTED_EDGE('',*,*,#2237,.F.);
#3217=ORIENTED_EDGE('',*,*,#2234,.F.);
#3218=ORIENTED_EDGE('',*,*,#2233,.F.);
#3219=ORIENTED_EDGE('',*,*,#2229,.F.);
#3220=ORIENTED_EDGE('',*,*,#2226,.F.);
#3221=ORIENTED_EDGE('',*,*,#2225,.F.);
#3222=ORIENTED_EDGE('',*,*,#2221,.F.);
#3223=ORIENTED_EDGE('',*,*,#2218,.F.);
#3224=ORIENTED_EDGE('',*,*,#2217,.F.);
#3225=ORIENTED_EDGE('',*,*,#2213,.F.);
#3226=ORIENTED_EDGE('',*,*,#2212,.F.);
#3227=ORIENTED_EDGE('',*,*,#2209,.F.);
#3228=ORIENTED_EDGE('',*,*,#2288,.F.);
#3229=ORIENTED_EDGE('',*,*,#2239,.F.);
#3230=ORIENTED_EDGE('',*,*,#2259,.F.);
#3231=ORIENTED_EDGE('',*,*,#2258,.F.);
#3232=ORIENTED_EDGE('',*,*,#2257,.F.);
#3233=ORIENTED_EDGE('',*,*,#2256,.F.);
#3234=ORIENTED_EDGE('',*,*,#2255,.F.);
#3235=ORIENTED_EDGE('',*,*,#2254,.F.);
#3236=ORIENTED_EDGE('',*,*,#2253,.F.);
#3237=ORIENTED_EDGE('',*,*,#2252,.F.);
#3238=ORIENTED_EDGE('',*,*,#2283,.T.);
#3239=ORIENTED_EDGE('',*,*,#2261,.T.);
#3240=ORIENTED_EDGE('',*,*,#2287,.T.);
#3241=ORIENTED_EDGE('',*,*,#2286,.T.);
#3242=ORIENTED_EDGE('',*,*,#2251,.T.);
#3243=ORIENTED_EDGE('',*,*,#2278,.F.);
#3244=ORIENTED_EDGE('',*,*,#2284,.T.);
#3245=ORIENTED_EDGE('',*,*,#2240,.T.);
#3246=ORIENTED_EDGE('',*,*,#2288,.T.);
#3247=ORIENTED_EDGE('',*,*,#2208,.T.);
#3248=ORIENTED_EDGE('',*,*,#2285,.F.);
#3249=ORIENTED_EDGE('',*,*,#2289,.T.);
#3250=ORIENTED_EDGE('',*,*,#2290,.T.);
#3251=ORIENTED_EDGE('',*,*,#2291,.F.);
#3252=ORIENTED_EDGE('',*,*,#2292,.F.);
#3253=ORIENTED_EDGE('',*,*,#2293,.T.);
#3254=ORIENTED_EDGE('',*,*,#2294,.T.);
#3255=ORIENTED_EDGE('',*,*,#2295,.T.);
#3256=ORIENTED_EDGE('',*,*,#2289,.F.);
#3257=ORIENTED_EDGE('',*,*,#2296,.F.);
#3258=ORIENTED_EDGE('',*,*,#2297,.F.);
#3259=ORIENTED_EDGE('',*,*,#2298,.T.);
#3260=ORIENTED_EDGE('',*,*,#2299,.T.);
#3261=ORIENTED_EDGE('',*,*,#2300,.T.);
#3262=ORIENTED_EDGE('',*,*,#2293,.F.);
#3263=ORIENTED_EDGE('',*,*,#2301,.F.);
#3264=ORIENTED_EDGE('',*,*,#2302,.F.);
#3265=ORIENTED_EDGE('',*,*,#2303,.T.);
#3266=ORIENTED_EDGE('',*,*,#2304,.T.);
#3267=ORIENTED_EDGE('',*,*,#2305,.T.);
#3268=ORIENTED_EDGE('',*,*,#2298,.F.);
#3269=ORIENTED_EDGE('',*,*,#2306,.F.);
#3270=ORIENTED_EDGE('',*,*,#2307,.F.);
#3271=ORIENTED_EDGE('',*,*,#2308,.T.);
#3272=ORIENTED_EDGE('',*,*,#2309,.T.);
#3273=ORIENTED_EDGE('',*,*,#2310,.T.);
#3274=ORIENTED_EDGE('',*,*,#2303,.F.);
#3275=ORIENTED_EDGE('',*,*,#2311,.F.);
#3276=ORIENTED_EDGE('',*,*,#2312,.F.);
#3277=ORIENTED_EDGE('',*,*,#2313,.T.);
#3278=ORIENTED_EDGE('',*,*,#2314,.T.);
#3279=ORIENTED_EDGE('',*,*,#2315,.T.);
#3280=ORIENTED_EDGE('',*,*,#2308,.F.);
#3281=ORIENTED_EDGE('',*,*,#2316,.F.);
#3282=ORIENTED_EDGE('',*,*,#2317,.F.);
#3283=ORIENTED_EDGE('',*,*,#2318,.T.);
#3284=ORIENTED_EDGE('',*,*,#2319,.T.);
#3285=ORIENTED_EDGE('',*,*,#2320,.T.);
#3286=ORIENTED_EDGE('',*,*,#2313,.F.);
#3287=ORIENTED_EDGE('',*,*,#2321,.F.);
#3288=ORIENTED_EDGE('',*,*,#2322,.F.);
#3289=ORIENTED_EDGE('',*,*,#2323,.T.);
#3290=ORIENTED_EDGE('',*,*,#2324,.T.);
#3291=ORIENTED_EDGE('',*,*,#2325,.T.);
#3292=ORIENTED_EDGE('',*,*,#2318,.F.);
#3293=ORIENTED_EDGE('',*,*,#2326,.F.);
#3294=ORIENTED_EDGE('',*,*,#2327,.F.);
#3295=ORIENTED_EDGE('',*,*,#2328,.F.);
#3296=ORIENTED_EDGE('',*,*,#2329,.F.);
#3297=ORIENTED_EDGE('',*,*,#2330,.F.);
#3298=ORIENTED_EDGE('',*,*,#2331,.F.);
#3299=ORIENTED_EDGE('',*,*,#2332,.T.);
#3300=ORIENTED_EDGE('',*,*,#2333,.T.);
#3301=ORIENTED_EDGE('',*,*,#2334,.F.);
#3302=ORIENTED_EDGE('',*,*,#2335,.T.);
#3303=ORIENTED_EDGE('',*,*,#2336,.T.);
#3304=ORIENTED_EDGE('',*,*,#2337,.T.);
#3305=ORIENTED_EDGE('',*,*,#2338,.T.);
#3306=ORIENTED_EDGE('',*,*,#2339,.T.);
#3307=ORIENTED_EDGE('',*,*,#2340,.T.);
#3308=ORIENTED_EDGE('',*,*,#2341,.T.);
#3309=ORIENTED_EDGE('',*,*,#2342,.T.);
#3310=ORIENTED_EDGE('',*,*,#2343,.T.);
#3311=ORIENTED_EDGE('',*,*,#2344,.T.);
#3312=ORIENTED_EDGE('',*,*,#2345,.T.);
#3313=ORIENTED_EDGE('',*,*,#2346,.T.);
#3314=ORIENTED_EDGE('',*,*,#2347,.T.);
#3315=ORIENTED_EDGE('',*,*,#2348,.T.);
#3316=ORIENTED_EDGE('',*,*,#2328,.T.);
#3317=ORIENTED_EDGE('',*,*,#2349,.T.);
#3318=ORIENTED_EDGE('',*,*,#2350,.T.);
#3319=ORIENTED_EDGE('',*,*,#2323,.F.);
#3320=ORIENTED_EDGE('',*,*,#2351,.F.);
#3321=ORIENTED_EDGE('',*,*,#2352,.F.);
#3322=ORIENTED_EDGE('',*,*,#2353,.F.);
#3323=ORIENTED_EDGE('',*,*,#2290,.F.);
#3324=ORIENTED_EDGE('',*,*,#2295,.F.);
#3325=ORIENTED_EDGE('',*,*,#2294,.F.);
#3326=ORIENTED_EDGE('',*,*,#2300,.F.);
#3327=ORIENTED_EDGE('',*,*,#2299,.F.);
#3328=ORIENTED_EDGE('',*,*,#2305,.F.);
#3329=ORIENTED_EDGE('',*,*,#2304,.F.);
#3330=ORIENTED_EDGE('',*,*,#2310,.F.);
#3331=ORIENTED_EDGE('',*,*,#2309,.F.);
#3332=ORIENTED_EDGE('',*,*,#2315,.F.);
#3333=ORIENTED_EDGE('',*,*,#2314,.F.);
#3334=ORIENTED_EDGE('',*,*,#2320,.F.);
#3335=ORIENTED_EDGE('',*,*,#2319,.F.);
#3336=ORIENTED_EDGE('',*,*,#2325,.F.);
#3337=ORIENTED_EDGE('',*,*,#2324,.F.);
#3338=ORIENTED_EDGE('',*,*,#2350,.F.);
#3339=ORIENTED_EDGE('',*,*,#2349,.F.);
#3340=ORIENTED_EDGE('',*,*,#2333,.F.);
#3341=ORIENTED_EDGE('',*,*,#2332,.F.);
#3342=ORIENTED_EDGE('',*,*,#2354,.F.);
#3343=ORIENTED_EDGE('',*,*,#2341,.F.);
#3344=ORIENTED_EDGE('',*,*,#2340,.F.);
#3345=ORIENTED_EDGE('',*,*,#2339,.F.);
#3346=ORIENTED_EDGE('',*,*,#2338,.F.);
#3347=ORIENTED_EDGE('',*,*,#2337,.F.);
#3348=ORIENTED_EDGE('',*,*,#2336,.F.);
#3349=ORIENTED_EDGE('',*,*,#2335,.F.);
#3350=ORIENTED_EDGE('',*,*,#2355,.F.);
#3351=ORIENTED_EDGE('',*,*,#2348,.F.);
#3352=ORIENTED_EDGE('',*,*,#2347,.F.);
#3353=ORIENTED_EDGE('',*,*,#2346,.F.);
#3354=ORIENTED_EDGE('',*,*,#2345,.F.);
#3355=ORIENTED_EDGE('',*,*,#2344,.F.);
#3356=ORIENTED_EDGE('',*,*,#2343,.F.);
#3357=ORIENTED_EDGE('',*,*,#2356,.F.);
#3358=ORIENTED_EDGE('',*,*,#2330,.T.);
#3359=ORIENTED_EDGE('',*,*,#2329,.T.);
#3360=ORIENTED_EDGE('',*,*,#2352,.T.);
#3361=ORIENTED_EDGE('',*,*,#2351,.T.);
#3362=ORIENTED_EDGE('',*,*,#2327,.T.);
#3363=ORIENTED_EDGE('',*,*,#2326,.T.);
#3364=ORIENTED_EDGE('',*,*,#2322,.T.);
#3365=ORIENTED_EDGE('',*,*,#2321,.T.);
#3366=ORIENTED_EDGE('',*,*,#2317,.T.);
#3367=ORIENTED_EDGE('',*,*,#2316,.T.);
#3368=ORIENTED_EDGE('',*,*,#2312,.T.);
#3369=ORIENTED_EDGE('',*,*,#2311,.T.);
#3370=ORIENTED_EDGE('',*,*,#2307,.T.);
#3371=ORIENTED_EDGE('',*,*,#2306,.T.);
#3372=ORIENTED_EDGE('',*,*,#2302,.T.);
#3373=ORIENTED_EDGE('',*,*,#2301,.T.);
#3374=ORIENTED_EDGE('',*,*,#2297,.T.);
#3375=ORIENTED_EDGE('',*,*,#2296,.T.);
#3376=ORIENTED_EDGE('',*,*,#2292,.T.);
#3377=ORIENTED_EDGE('',*,*,#2357,.F.);
#3378=ORIENTED_EDGE('',*,*,#2358,.F.);
#3379=ORIENTED_EDGE('',*,*,#2354,.T.);
#3380=ORIENTED_EDGE('',*,*,#2331,.T.);
#3381=ORIENTED_EDGE('',*,*,#2356,.T.);
#3382=ORIENTED_EDGE('',*,*,#2342,.F.);
#3383=ORIENTED_EDGE('',*,*,#2359,.F.);
#3384=ORIENTED_EDGE('',*,*,#2360,.T.);
#3385=ORIENTED_EDGE('',*,*,#2361,.F.);
#3386=ORIENTED_EDGE('',*,*,#2362,.F.);
#3387=ORIENTED_EDGE('',*,*,#2363,.F.);
#3388=ORIENTED_EDGE('',*,*,#2364,.F.);
#3389=ORIENTED_EDGE('',*,*,#2365,.F.);
#3390=ORIENTED_EDGE('',*,*,#2360,.F.);
#3391=ORIENTED_EDGE('',*,*,#2359,.T.);
#3392=ORIENTED_EDGE('',*,*,#2353,.T.);
#3393=ORIENTED_EDGE('',*,*,#2334,.T.);
#3394=ORIENTED_EDGE('',*,*,#2355,.T.);
#3395=ORIENTED_EDGE('',*,*,#2291,.T.);
#3396=ORIENTED_EDGE('',*,*,#2358,.T.);
#3397=ORIENTED_EDGE('',*,*,#2366,.F.);
#3398=ORIENTED_EDGE('',*,*,#2357,.T.);
#3399=ORIENTED_EDGE('',*,*,#2367,.F.);
#3400=ORIENTED_EDGE('',*,*,#2368,.F.);
#3401=ORIENTED_EDGE('',*,*,#2369,.T.);
#3402=ORIENTED_EDGE('',*,*,#2370,.F.);
#3403=ORIENTED_EDGE('',*,*,#2371,.F.);
#3404=ORIENTED_EDGE('',*,*,#2372,.F.);
#3405=ORIENTED_EDGE('',*,*,#2373,.F.);
#3406=ORIENTED_EDGE('',*,*,#2374,.F.);
#3407=ORIENTED_EDGE('',*,*,#2369,.F.);
#3408=ORIENTED_EDGE('',*,*,#2370,.T.);
#3409=ORIENTED_EDGE('',*,*,#2374,.T.);
#3410=ORIENTED_EDGE('',*,*,#2375,.T.);
#3411=ORIENTED_EDGE('',*,*,#2376,.F.);
#3412=ORIENTED_EDGE('',*,*,#2377,.T.);
#3413=ORIENTED_EDGE('',*,*,#2378,.F.);
#3414=ORIENTED_EDGE('',*,*,#2379,.T.);
#3415=ORIENTED_EDGE('',*,*,#2373,.T.);
#3416=ORIENTED_EDGE('',*,*,#2380,.F.);
#3417=ORIENTED_EDGE('',*,*,#2381,.F.);
#3418=ORIENTED_EDGE('',*,*,#2375,.F.);
#3419=ORIENTED_EDGE('',*,*,#2361,.T.);
#3420=ORIENTED_EDGE('',*,*,#2365,.T.);
#3421=ORIENTED_EDGE('',*,*,#2382,.T.);
#3422=ORIENTED_EDGE('',*,*,#2383,.F.);
#3423=ORIENTED_EDGE('',*,*,#2384,.T.);
#3424=ORIENTED_EDGE('',*,*,#2385,.F.);
#3425=ORIENTED_EDGE('',*,*,#2386,.T.);
#3426=ORIENTED_EDGE('',*,*,#2364,.T.);
#3427=ORIENTED_EDGE('',*,*,#2387,.F.);
#3428=ORIENTED_EDGE('',*,*,#2388,.F.);
#3429=ORIENTED_EDGE('',*,*,#2382,.F.);
#3430=ORIENTED_EDGE('',*,*,#2389,.T.);
#3431=ORIENTED_EDGE('',*,*,#2390,.T.);
#3432=ORIENTED_EDGE('',*,*,#2391,.T.);
#3433=ORIENTED_EDGE('',*,*,#2376,.T.);
#3434=ORIENTED_EDGE('',*,*,#2392,.T.);
#3435=ORIENTED_EDGE('',*,*,#2393,.T.);
#3436=ORIENTED_EDGE('',*,*,#2391,.F.);
#3437=ORIENTED_EDGE('',*,*,#2394,.T.);
#3438=ORIENTED_EDGE('',*,*,#2395,.T.);
#3439=ORIENTED_EDGE('',*,*,#2396,.T.);
#3440=ORIENTED_EDGE('',*,*,#2392,.F.);
#3441=ORIENTED_EDGE('',*,*,#2397,.T.);
#3442=ORIENTED_EDGE('',*,*,#2398,.T.);
#3443=ORIENTED_EDGE('',*,*,#2399,.T.);
#3444=ORIENTED_EDGE('',*,*,#2395,.F.);
#3445=ORIENTED_EDGE('',*,*,#2400,.T.);
#3446=ORIENTED_EDGE('',*,*,#2401,.T.);
#3447=ORIENTED_EDGE('',*,*,#2402,.T.);
#3448=ORIENTED_EDGE('',*,*,#2398,.F.);
#3449=ORIENTED_EDGE('',*,*,#2403,.T.);
#3450=ORIENTED_EDGE('',*,*,#2404,.T.);
#3451=ORIENTED_EDGE('',*,*,#2405,.T.);
#3452=ORIENTED_EDGE('',*,*,#2401,.F.);
#3453=ORIENTED_EDGE('',*,*,#2406,.T.);
#3454=ORIENTED_EDGE('',*,*,#2407,.T.);
#3455=ORIENTED_EDGE('',*,*,#2408,.T.);
#3456=ORIENTED_EDGE('',*,*,#2404,.F.);
#3457=ORIENTED_EDGE('',*,*,#2409,.T.);
#3458=ORIENTED_EDGE('',*,*,#2410,.T.);
#3459=ORIENTED_EDGE('',*,*,#2411,.T.);
#3460=ORIENTED_EDGE('',*,*,#2407,.F.);
#3461=ORIENTED_EDGE('',*,*,#2412,.T.);
#3462=ORIENTED_EDGE('',*,*,#2413,.T.);
#3463=ORIENTED_EDGE('',*,*,#2414,.T.);
#3464=ORIENTED_EDGE('',*,*,#2410,.F.);
#3465=ORIENTED_EDGE('',*,*,#2415,.T.);
#3466=ORIENTED_EDGE('',*,*,#2416,.T.);
#3467=ORIENTED_EDGE('',*,*,#2417,.T.);
#3468=ORIENTED_EDGE('',*,*,#2413,.F.);
#3469=ORIENTED_EDGE('',*,*,#2418,.T.);
#3470=ORIENTED_EDGE('',*,*,#2419,.T.);
#3471=ORIENTED_EDGE('',*,*,#2420,.T.);
#3472=ORIENTED_EDGE('',*,*,#2416,.F.);
#3473=ORIENTED_EDGE('',*,*,#2421,.T.);
#3474=ORIENTED_EDGE('',*,*,#2422,.T.);
#3475=ORIENTED_EDGE('',*,*,#2423,.T.);
#3476=ORIENTED_EDGE('',*,*,#2419,.F.);
#3477=ORIENTED_EDGE('',*,*,#2424,.T.);
#3478=ORIENTED_EDGE('',*,*,#2425,.T.);
#3479=ORIENTED_EDGE('',*,*,#2426,.T.);
#3480=ORIENTED_EDGE('',*,*,#2422,.F.);
#3481=ORIENTED_EDGE('',*,*,#2427,.T.);
#3482=ORIENTED_EDGE('',*,*,#2428,.T.);
#3483=ORIENTED_EDGE('',*,*,#2429,.T.);
#3484=ORIENTED_EDGE('',*,*,#2425,.F.);
#3485=ORIENTED_EDGE('',*,*,#2430,.T.);
#3486=ORIENTED_EDGE('',*,*,#2431,.T.);
#3487=ORIENTED_EDGE('',*,*,#2385,.T.);
#3488=ORIENTED_EDGE('',*,*,#2428,.F.);
#3489=ORIENTED_EDGE('',*,*,#2432,.T.);
#3490=ORIENTED_EDGE('',*,*,#2433,.T.);
#3491=ORIENTED_EDGE('',*,*,#2434,.T.);
#3492=ORIENTED_EDGE('',*,*,#2431,.F.);
#3493=ORIENTED_EDGE('',*,*,#2435,.T.);
#3494=ORIENTED_EDGE('',*,*,#2436,.T.);
#3495=ORIENTED_EDGE('',*,*,#2437,.T.);
#3496=ORIENTED_EDGE('',*,*,#2433,.F.);
#3497=ORIENTED_EDGE('',*,*,#2438,.T.);
#3498=ORIENTED_EDGE('',*,*,#2439,.T.);
#3499=ORIENTED_EDGE('',*,*,#2440,.T.);
#3500=ORIENTED_EDGE('',*,*,#2436,.F.);
#3501=ORIENTED_EDGE('',*,*,#2441,.T.);
#3502=ORIENTED_EDGE('',*,*,#2442,.T.);
#3503=ORIENTED_EDGE('',*,*,#2443,.T.);
#3504=ORIENTED_EDGE('',*,*,#2439,.F.);
#3505=ORIENTED_EDGE('',*,*,#2444,.T.);
#3506=ORIENTED_EDGE('',*,*,#2445,.T.);
#3507=ORIENTED_EDGE('',*,*,#2446,.T.);
#3508=ORIENTED_EDGE('',*,*,#2442,.F.);
#3509=ORIENTED_EDGE('',*,*,#2447,.T.);
#3510=ORIENTED_EDGE('',*,*,#2448,.T.);
#3511=ORIENTED_EDGE('',*,*,#2449,.T.);
#3512=ORIENTED_EDGE('',*,*,#2445,.F.);
#3513=ORIENTED_EDGE('',*,*,#2450,.T.);
#3514=ORIENTED_EDGE('',*,*,#2451,.T.);
#3515=ORIENTED_EDGE('',*,*,#2452,.T.);
#3516=ORIENTED_EDGE('',*,*,#2448,.F.);
#3517=ORIENTED_EDGE('',*,*,#2453,.T.);
#3518=ORIENTED_EDGE('',*,*,#2454,.T.);
#3519=ORIENTED_EDGE('',*,*,#2455,.T.);
#3520=ORIENTED_EDGE('',*,*,#2451,.F.);
#3521=ORIENTED_EDGE('',*,*,#2456,.T.);
#3522=ORIENTED_EDGE('',*,*,#2457,.T.);
#3523=ORIENTED_EDGE('',*,*,#2458,.T.);
#3524=ORIENTED_EDGE('',*,*,#2454,.F.);
#3525=ORIENTED_EDGE('',*,*,#2459,.T.);
#3526=ORIENTED_EDGE('',*,*,#2460,.T.);
#3527=ORIENTED_EDGE('',*,*,#2461,.T.);
#3528=ORIENTED_EDGE('',*,*,#2457,.F.);
#3529=ORIENTED_EDGE('',*,*,#2462,.T.);
#3530=ORIENTED_EDGE('',*,*,#2463,.T.);
#3531=ORIENTED_EDGE('',*,*,#2464,.T.);
#3532=ORIENTED_EDGE('',*,*,#2460,.F.);
#3533=ORIENTED_EDGE('',*,*,#2465,.T.);
#3534=ORIENTED_EDGE('',*,*,#2466,.T.);
#3535=ORIENTED_EDGE('',*,*,#2467,.T.);
#3536=ORIENTED_EDGE('',*,*,#2463,.F.);
#3537=ORIENTED_EDGE('',*,*,#2468,.T.);
#3538=ORIENTED_EDGE('',*,*,#2469,.T.);
#3539=ORIENTED_EDGE('',*,*,#2470,.T.);
#3540=ORIENTED_EDGE('',*,*,#2466,.F.);
#3541=ORIENTED_EDGE('',*,*,#2471,.T.);
#3542=ORIENTED_EDGE('',*,*,#2472,.T.);
#3543=ORIENTED_EDGE('',*,*,#2473,.T.);
#3544=ORIENTED_EDGE('',*,*,#2469,.F.);
#3545=ORIENTED_EDGE('',*,*,#2474,.T.);
#3546=ORIENTED_EDGE('',*,*,#2475,.T.);
#3547=ORIENTED_EDGE('',*,*,#2476,.T.);
#3548=ORIENTED_EDGE('',*,*,#2472,.F.);
#3549=ORIENTED_EDGE('',*,*,#2477,.T.);
#3550=ORIENTED_EDGE('',*,*,#2478,.T.);
#3551=ORIENTED_EDGE('',*,*,#2479,.T.);
#3552=ORIENTED_EDGE('',*,*,#2475,.F.);
#3553=ORIENTED_EDGE('',*,*,#2480,.T.);
#3554=ORIENTED_EDGE('',*,*,#2478,.F.);
#3555=ORIENTED_EDGE('',*,*,#2481,.T.);
#3556=ORIENTED_EDGE('',*,*,#2389,.F.);
#3557=ORIENTED_EDGE('',*,*,#2381,.T.);
#3558=ORIENTED_EDGE('',*,*,#2440,.F.);
#3559=ORIENTED_EDGE('',*,*,#2482,.F.);
#3560=ORIENTED_EDGE('',*,*,#2483,.F.);
#3561=ORIENTED_EDGE('',*,*,#2484,.F.);
#3562=ORIENTED_EDGE('',*,*,#2443,.F.);
#3563=ORIENTED_EDGE('',*,*,#2485,.T.);
#3564=ORIENTED_EDGE('',*,*,#2486,.F.);
#3565=ORIENTED_EDGE('',*,*,#2482,.T.);
#3566=ORIENTED_EDGE('',*,*,#2446,.F.);
#3567=ORIENTED_EDGE('',*,*,#2487,.F.);
#3568=ORIENTED_EDGE('',*,*,#2488,.F.);
#3569=ORIENTED_EDGE('',*,*,#2485,.F.);
#3570=ORIENTED_EDGE('',*,*,#2449,.F.);
#3571=ORIENTED_EDGE('',*,*,#2489,.T.);
#3572=ORIENTED_EDGE('',*,*,#2490,.F.);
#3573=ORIENTED_EDGE('',*,*,#2487,.T.);
#3574=ORIENTED_EDGE('',*,*,#2452,.F.);
#3575=ORIENTED_EDGE('',*,*,#2491,.F.);
#3576=ORIENTED_EDGE('',*,*,#2492,.F.);
#3577=ORIENTED_EDGE('',*,*,#2489,.F.);
#3578=ORIENTED_EDGE('',*,*,#2455,.F.);
#3579=ORIENTED_EDGE('',*,*,#2493,.T.);
#3580=ORIENTED_EDGE('',*,*,#2494,.F.);
#3581=ORIENTED_EDGE('',*,*,#2491,.T.);
#3582=ORIENTED_EDGE('',*,*,#2458,.F.);
#3583=ORIENTED_EDGE('',*,*,#2495,.F.);
#3584=ORIENTED_EDGE('',*,*,#2496,.F.);
#3585=ORIENTED_EDGE('',*,*,#2493,.F.);
#3586=ORIENTED_EDGE('',*,*,#2461,.F.);
#3587=ORIENTED_EDGE('',*,*,#2497,.T.);
#3588=ORIENTED_EDGE('',*,*,#2498,.F.);
#3589=ORIENTED_EDGE('',*,*,#2495,.T.);
#3590=ORIENTED_EDGE('',*,*,#2464,.F.);
#3591=ORIENTED_EDGE('',*,*,#2499,.F.);
#3592=ORIENTED_EDGE('',*,*,#2500,.F.);
#3593=ORIENTED_EDGE('',*,*,#2497,.F.);
#3594=ORIENTED_EDGE('',*,*,#2467,.F.);
#3595=ORIENTED_EDGE('',*,*,#2501,.T.);
#3596=ORIENTED_EDGE('',*,*,#2502,.F.);
#3597=ORIENTED_EDGE('',*,*,#2499,.T.);
#3598=ORIENTED_EDGE('',*,*,#2470,.F.);
#3599=ORIENTED_EDGE('',*,*,#2503,.F.);
#3600=ORIENTED_EDGE('',*,*,#2504,.F.);
#3601=ORIENTED_EDGE('',*,*,#2501,.F.);
#3602=ORIENTED_EDGE('',*,*,#2473,.F.);
#3603=ORIENTED_EDGE('',*,*,#2505,.T.);
#3604=ORIENTED_EDGE('',*,*,#2506,.F.);
#3605=ORIENTED_EDGE('',*,*,#2503,.T.);
#3606=ORIENTED_EDGE('',*,*,#2476,.F.);
#3607=ORIENTED_EDGE('',*,*,#2507,.F.);
#3608=ORIENTED_EDGE('',*,*,#2508,.F.);
#3609=ORIENTED_EDGE('',*,*,#2505,.F.);
#3610=ORIENTED_EDGE('',*,*,#2372,.T.);
#3611=ORIENTED_EDGE('',*,*,#2509,.T.);
#3612=ORIENTED_EDGE('',*,*,#2510,.F.);
#3613=ORIENTED_EDGE('',*,*,#2507,.T.);
#3614=ORIENTED_EDGE('',*,*,#2479,.F.);
#3615=ORIENTED_EDGE('',*,*,#2380,.T.);
#3616=ORIENTED_EDGE('',*,*,#2371,.T.);
#3617=ORIENTED_EDGE('',*,*,#2379,.F.);
#3618=ORIENTED_EDGE('',*,*,#2511,.F.);
#3619=ORIENTED_EDGE('',*,*,#2509,.F.);
#3620=ORIENTED_EDGE('',*,*,#2390,.F.);
#3621=ORIENTED_EDGE('',*,*,#2481,.F.);
#3622=ORIENTED_EDGE('',*,*,#2480,.F.);
#3623=ORIENTED_EDGE('',*,*,#2477,.F.);
#3624=ORIENTED_EDGE('',*,*,#2474,.F.);
#3625=ORIENTED_EDGE('',*,*,#2471,.F.);
#3626=ORIENTED_EDGE('',*,*,#2468,.F.);
#3627=ORIENTED_EDGE('',*,*,#2465,.F.);
#3628=ORIENTED_EDGE('',*,*,#2462,.F.);
#3629=ORIENTED_EDGE('',*,*,#2459,.F.);
#3630=ORIENTED_EDGE('',*,*,#2456,.F.);
#3631=ORIENTED_EDGE('',*,*,#2453,.F.);
#3632=ORIENTED_EDGE('',*,*,#2450,.F.);
#3633=ORIENTED_EDGE('',*,*,#2447,.F.);
#3634=ORIENTED_EDGE('',*,*,#2444,.F.);
#3635=ORIENTED_EDGE('',*,*,#2441,.F.);
#3636=ORIENTED_EDGE('',*,*,#2438,.F.);
#3637=ORIENTED_EDGE('',*,*,#2435,.F.);
#3638=ORIENTED_EDGE('',*,*,#2432,.F.);
#3639=ORIENTED_EDGE('',*,*,#2430,.F.);
#3640=ORIENTED_EDGE('',*,*,#2427,.F.);
#3641=ORIENTED_EDGE('',*,*,#2424,.F.);
#3642=ORIENTED_EDGE('',*,*,#2421,.F.);
#3643=ORIENTED_EDGE('',*,*,#2418,.F.);
#3644=ORIENTED_EDGE('',*,*,#2415,.F.);
#3645=ORIENTED_EDGE('',*,*,#2412,.F.);
#3646=ORIENTED_EDGE('',*,*,#2409,.F.);
#3647=ORIENTED_EDGE('',*,*,#2406,.F.);
#3648=ORIENTED_EDGE('',*,*,#2403,.F.);
#3649=ORIENTED_EDGE('',*,*,#2400,.F.);
#3650=ORIENTED_EDGE('',*,*,#2397,.F.);
#3651=ORIENTED_EDGE('',*,*,#2394,.F.);
#3652=ORIENTED_EDGE('',*,*,#2512,.F.);
#3653=ORIENTED_EDGE('',*,*,#2513,.T.);
#3654=ORIENTED_EDGE('',*,*,#2514,.T.);
#3655=ORIENTED_EDGE('',*,*,#2515,.T.);
#3656=ORIENTED_EDGE('',*,*,#2516,.T.);
#3657=ORIENTED_EDGE('',*,*,#2517,.T.);
#3658=ORIENTED_EDGE('',*,*,#2518,.T.);
#3659=ORIENTED_EDGE('',*,*,#2519,.T.);
#3660=ORIENTED_EDGE('',*,*,#2520,.T.);
#3661=ORIENTED_EDGE('',*,*,#2521,.T.);
#3662=ORIENTED_EDGE('',*,*,#2522,.T.);
#3663=ORIENTED_EDGE('',*,*,#2523,.T.);
#3664=ORIENTED_EDGE('',*,*,#2524,.T.);
#3665=ORIENTED_EDGE('',*,*,#2525,.T.);
#3666=ORIENTED_EDGE('',*,*,#2526,.T.);
#3667=ORIENTED_EDGE('',*,*,#2523,.F.);
#3668=ORIENTED_EDGE('',*,*,#2527,.T.);
#3669=ORIENTED_EDGE('',*,*,#2528,.T.);
#3670=ORIENTED_EDGE('',*,*,#2378,.T.);
#3671=ORIENTED_EDGE('',*,*,#2525,.F.);
#3672=ORIENTED_EDGE('',*,*,#2529,.T.);
#3673=ORIENTED_EDGE('',*,*,#2530,.T.);
#3674=ORIENTED_EDGE('',*,*,#2511,.T.);
#3675=ORIENTED_EDGE('',*,*,#2528,.F.);
#3676=ORIENTED_EDGE('',*,*,#2531,.T.);
#3677=ORIENTED_EDGE('',*,*,#2532,.T.);
#3678=ORIENTED_EDGE('',*,*,#2510,.T.);
#3679=ORIENTED_EDGE('',*,*,#2530,.F.);
#3680=ORIENTED_EDGE('',*,*,#2533,.T.);
#3681=ORIENTED_EDGE('',*,*,#2534,.T.);
#3682=ORIENTED_EDGE('',*,*,#2508,.T.);
#3683=ORIENTED_EDGE('',*,*,#2532,.F.);
#3684=ORIENTED_EDGE('',*,*,#2535,.T.);
#3685=ORIENTED_EDGE('',*,*,#2536,.T.);
#3686=ORIENTED_EDGE('',*,*,#2506,.T.);
#3687=ORIENTED_EDGE('',*,*,#2534,.F.);
#3688=ORIENTED_EDGE('',*,*,#2537,.T.);
#3689=ORIENTED_EDGE('',*,*,#2538,.T.);
#3690=ORIENTED_EDGE('',*,*,#2504,.T.);
#3691=ORIENTED_EDGE('',*,*,#2536,.F.);
#3692=ORIENTED_EDGE('',*,*,#2539,.T.);
#3693=ORIENTED_EDGE('',*,*,#2540,.T.);
#3694=ORIENTED_EDGE('',*,*,#2502,.T.);
#3695=ORIENTED_EDGE('',*,*,#2538,.F.);
#3696=ORIENTED_EDGE('',*,*,#2541,.T.);
#3697=ORIENTED_EDGE('',*,*,#2542,.T.);
#3698=ORIENTED_EDGE('',*,*,#2500,.T.);
#3699=ORIENTED_EDGE('',*,*,#2540,.F.);
#3700=ORIENTED_EDGE('',*,*,#2543,.T.);
#3701=ORIENTED_EDGE('',*,*,#2544,.T.);
#3702=ORIENTED_EDGE('',*,*,#2498,.T.);
#3703=ORIENTED_EDGE('',*,*,#2542,.F.);
#3704=ORIENTED_EDGE('',*,*,#2545,.T.);
#3705=ORIENTED_EDGE('',*,*,#2546,.T.);
#3706=ORIENTED_EDGE('',*,*,#2496,.T.);
#3707=ORIENTED_EDGE('',*,*,#2544,.F.);
#3708=ORIENTED_EDGE('',*,*,#2547,.T.);
#3709=ORIENTED_EDGE('',*,*,#2548,.T.);
#3710=ORIENTED_EDGE('',*,*,#2494,.T.);
#3711=ORIENTED_EDGE('',*,*,#2546,.F.);
#3712=ORIENTED_EDGE('',*,*,#2549,.T.);
#3713=ORIENTED_EDGE('',*,*,#2550,.T.);
#3714=ORIENTED_EDGE('',*,*,#2492,.T.);
#3715=ORIENTED_EDGE('',*,*,#2548,.F.);
#3716=ORIENTED_EDGE('',*,*,#2551,.T.);
#3717=ORIENTED_EDGE('',*,*,#2552,.T.);
#3718=ORIENTED_EDGE('',*,*,#2490,.T.);
#3719=ORIENTED_EDGE('',*,*,#2550,.F.);
#3720=ORIENTED_EDGE('',*,*,#2553,.T.);
#3721=ORIENTED_EDGE('',*,*,#2554,.T.);
#3722=ORIENTED_EDGE('',*,*,#2488,.T.);
#3723=ORIENTED_EDGE('',*,*,#2552,.F.);
#3724=ORIENTED_EDGE('',*,*,#2555,.T.);
#3725=ORIENTED_EDGE('',*,*,#2556,.T.);
#3726=ORIENTED_EDGE('',*,*,#2486,.T.);
#3727=ORIENTED_EDGE('',*,*,#2554,.F.);
#3728=ORIENTED_EDGE('',*,*,#2557,.T.);
#3729=ORIENTED_EDGE('',*,*,#2558,.T.);
#3730=ORIENTED_EDGE('',*,*,#2483,.T.);
#3731=ORIENTED_EDGE('',*,*,#2556,.F.);
#3732=ORIENTED_EDGE('',*,*,#2559,.T.);
#3733=ORIENTED_EDGE('',*,*,#2560,.T.);
#3734=ORIENTED_EDGE('',*,*,#2561,.T.);
#3735=ORIENTED_EDGE('',*,*,#2558,.F.);
#3736=ORIENTED_EDGE('',*,*,#2562,.T.);
#3737=ORIENTED_EDGE('',*,*,#2563,.T.);
#3738=ORIENTED_EDGE('',*,*,#2388,.T.);
#3739=ORIENTED_EDGE('',*,*,#2560,.F.);
#3740=ORIENTED_EDGE('',*,*,#2564,.T.);
#3741=ORIENTED_EDGE('',*,*,#2565,.T.);
#3742=ORIENTED_EDGE('',*,*,#2383,.T.);
#3743=ORIENTED_EDGE('',*,*,#2563,.F.);
#3744=ORIENTED_EDGE('',*,*,#2566,.T.);
#3745=ORIENTED_EDGE('',*,*,#2567,.T.);
#3746=ORIENTED_EDGE('',*,*,#2568,.T.);
#3747=ORIENTED_EDGE('',*,*,#2565,.F.);
#3748=ORIENTED_EDGE('',*,*,#2569,.T.);
#3749=ORIENTED_EDGE('',*,*,#2570,.T.);
#3750=ORIENTED_EDGE('',*,*,#2571,.T.);
#3751=ORIENTED_EDGE('',*,*,#2567,.F.);
#3752=ORIENTED_EDGE('',*,*,#2572,.T.);
#3753=ORIENTED_EDGE('',*,*,#2573,.T.);
#3754=ORIENTED_EDGE('',*,*,#2574,.T.);
#3755=ORIENTED_EDGE('',*,*,#2570,.F.);
#3756=ORIENTED_EDGE('',*,*,#2575,.T.);
#3757=ORIENTED_EDGE('',*,*,#2576,.T.);
#3758=ORIENTED_EDGE('',*,*,#2577,.T.);
#3759=ORIENTED_EDGE('',*,*,#2573,.F.);
#3760=ORIENTED_EDGE('',*,*,#2578,.T.);
#3761=ORIENTED_EDGE('',*,*,#2579,.T.);
#3762=ORIENTED_EDGE('',*,*,#2580,.T.);
#3763=ORIENTED_EDGE('',*,*,#2576,.F.);
#3764=ORIENTED_EDGE('',*,*,#2581,.T.);
#3765=ORIENTED_EDGE('',*,*,#2582,.T.);
#3766=ORIENTED_EDGE('',*,*,#2583,.T.);
#3767=ORIENTED_EDGE('',*,*,#2579,.F.);
#3768=ORIENTED_EDGE('',*,*,#2584,.T.);
#3769=ORIENTED_EDGE('',*,*,#2585,.T.);
#3770=ORIENTED_EDGE('',*,*,#2586,.T.);
#3771=ORIENTED_EDGE('',*,*,#2582,.F.);
#3772=ORIENTED_EDGE('',*,*,#2587,.T.);
#3773=ORIENTED_EDGE('',*,*,#2588,.T.);
#3774=ORIENTED_EDGE('',*,*,#2589,.T.);
#3775=ORIENTED_EDGE('',*,*,#2585,.F.);
#3776=ORIENTED_EDGE('',*,*,#2590,.T.);
#3777=ORIENTED_EDGE('',*,*,#2591,.T.);
#3778=ORIENTED_EDGE('',*,*,#2592,.T.);
#3779=ORIENTED_EDGE('',*,*,#2588,.F.);
#3780=ORIENTED_EDGE('',*,*,#2593,.T.);
#3781=ORIENTED_EDGE('',*,*,#2594,.T.);
#3782=ORIENTED_EDGE('',*,*,#2595,.T.);
#3783=ORIENTED_EDGE('',*,*,#2591,.F.);
#3784=ORIENTED_EDGE('',*,*,#2596,.T.);
#3785=ORIENTED_EDGE('',*,*,#2594,.F.);
#3786=ORIENTED_EDGE('',*,*,#2597,.T.);
#3787=ORIENTED_EDGE('',*,*,#2521,.F.);
#3788=ORIENTED_EDGE('',*,*,#2598,.T.);
#3789=ORIENTED_EDGE('',*,*,#2363,.T.);
#3790=ORIENTED_EDGE('',*,*,#2599,.T.);
#3791=ORIENTED_EDGE('',*,*,#2437,.F.);
#3792=ORIENTED_EDGE('',*,*,#2484,.T.);
#3793=ORIENTED_EDGE('',*,*,#2561,.F.);
#3794=ORIENTED_EDGE('',*,*,#2387,.T.);
#3795=ORIENTED_EDGE('',*,*,#2362,.T.);
#3796=ORIENTED_EDGE('',*,*,#2386,.F.);
#3797=ORIENTED_EDGE('',*,*,#2434,.F.);
#3798=ORIENTED_EDGE('',*,*,#2599,.F.);
#3799=ORIENTED_EDGE('',*,*,#2429,.F.);
#3800=ORIENTED_EDGE('',*,*,#2384,.F.);
#3801=ORIENTED_EDGE('',*,*,#2568,.F.);
#3802=ORIENTED_EDGE('',*,*,#2600,.F.);
#3803=ORIENTED_EDGE('',*,*,#2426,.F.);
#3804=ORIENTED_EDGE('',*,*,#2600,.T.);
#3805=ORIENTED_EDGE('',*,*,#2571,.F.);
#3806=ORIENTED_EDGE('',*,*,#2601,.T.);
#3807=ORIENTED_EDGE('',*,*,#2423,.F.);
#3808=ORIENTED_EDGE('',*,*,#2601,.F.);
#3809=ORIENTED_EDGE('',*,*,#2574,.F.);
#3810=ORIENTED_EDGE('',*,*,#2602,.F.);
#3811=ORIENTED_EDGE('',*,*,#2420,.F.);
#3812=ORIENTED_EDGE('',*,*,#2602,.T.);
#3813=ORIENTED_EDGE('',*,*,#2577,.F.);
#3814=ORIENTED_EDGE('',*,*,#2603,.T.);
#3815=ORIENTED_EDGE('',*,*,#2417,.F.);
#3816=ORIENTED_EDGE('',*,*,#2603,.F.);
#3817=ORIENTED_EDGE('',*,*,#2580,.F.);
#3818=ORIENTED_EDGE('',*,*,#2604,.F.);
#3819=ORIENTED_EDGE('',*,*,#2414,.F.);
#3820=ORIENTED_EDGE('',*,*,#2604,.T.);
#3821=ORIENTED_EDGE('',*,*,#2583,.F.);
#3822=ORIENTED_EDGE('',*,*,#2605,.T.);
#3823=ORIENTED_EDGE('',*,*,#2411,.F.);
#3824=ORIENTED_EDGE('',*,*,#2605,.F.);
#3825=ORIENTED_EDGE('',*,*,#2586,.F.);
#3826=ORIENTED_EDGE('',*,*,#2606,.F.);
#3827=ORIENTED_EDGE('',*,*,#2408,.F.);
#3828=ORIENTED_EDGE('',*,*,#2606,.T.);
#3829=ORIENTED_EDGE('',*,*,#2589,.F.);
#3830=ORIENTED_EDGE('',*,*,#2607,.T.);
#3831=ORIENTED_EDGE('',*,*,#2405,.F.);
#3832=ORIENTED_EDGE('',*,*,#2607,.F.);
#3833=ORIENTED_EDGE('',*,*,#2592,.F.);
#3834=ORIENTED_EDGE('',*,*,#2608,.F.);
#3835=ORIENTED_EDGE('',*,*,#2402,.F.);
#3836=ORIENTED_EDGE('',*,*,#2608,.T.);
#3837=ORIENTED_EDGE('',*,*,#2595,.F.);
#3838=ORIENTED_EDGE('',*,*,#2609,.T.);
#3839=ORIENTED_EDGE('',*,*,#2399,.F.);
#3840=ORIENTED_EDGE('',*,*,#2609,.F.);
#3841=ORIENTED_EDGE('',*,*,#2598,.F.);
#3842=ORIENTED_EDGE('',*,*,#2610,.F.);
#3843=ORIENTED_EDGE('',*,*,#2396,.F.);
#3844=ORIENTED_EDGE('',*,*,#2610,.T.);
#3845=ORIENTED_EDGE('',*,*,#2524,.F.);
#3846=ORIENTED_EDGE('',*,*,#2611,.T.);
#3847=ORIENTED_EDGE('',*,*,#2522,.F.);
#3848=ORIENTED_EDGE('',*,*,#2597,.F.);
#3849=ORIENTED_EDGE('',*,*,#2596,.F.);
#3850=ORIENTED_EDGE('',*,*,#2593,.F.);
#3851=ORIENTED_EDGE('',*,*,#2590,.F.);
#3852=ORIENTED_EDGE('',*,*,#2587,.F.);
#3853=ORIENTED_EDGE('',*,*,#2584,.F.);
#3854=ORIENTED_EDGE('',*,*,#2581,.F.);
#3855=ORIENTED_EDGE('',*,*,#2578,.F.);
#3856=ORIENTED_EDGE('',*,*,#2575,.F.);
#3857=ORIENTED_EDGE('',*,*,#2572,.F.);
#3858=ORIENTED_EDGE('',*,*,#2569,.F.);
#3859=ORIENTED_EDGE('',*,*,#2566,.F.);
#3860=ORIENTED_EDGE('',*,*,#2564,.F.);
#3861=ORIENTED_EDGE('',*,*,#2562,.F.);
#3862=ORIENTED_EDGE('',*,*,#2559,.F.);
#3863=ORIENTED_EDGE('',*,*,#2557,.F.);
#3864=ORIENTED_EDGE('',*,*,#2555,.F.);
#3865=ORIENTED_EDGE('',*,*,#2553,.F.);
#3866=ORIENTED_EDGE('',*,*,#2551,.F.);
#3867=ORIENTED_EDGE('',*,*,#2549,.F.);
#3868=ORIENTED_EDGE('',*,*,#2547,.F.);
#3869=ORIENTED_EDGE('',*,*,#2545,.F.);
#3870=ORIENTED_EDGE('',*,*,#2543,.F.);
#3871=ORIENTED_EDGE('',*,*,#2541,.F.);
#3872=ORIENTED_EDGE('',*,*,#2539,.F.);
#3873=ORIENTED_EDGE('',*,*,#2537,.F.);
#3874=ORIENTED_EDGE('',*,*,#2535,.F.);
#3875=ORIENTED_EDGE('',*,*,#2533,.F.);
#3876=ORIENTED_EDGE('',*,*,#2531,.F.);
#3877=ORIENTED_EDGE('',*,*,#2529,.F.);
#3878=ORIENTED_EDGE('',*,*,#2527,.F.);
#3879=ORIENTED_EDGE('',*,*,#2612,.F.);
#3880=ORIENTED_EDGE('',*,*,#2613,.T.);
#3881=ORIENTED_EDGE('',*,*,#2614,.T.);
#3882=ORIENTED_EDGE('',*,*,#2615,.T.);
#3883=ORIENTED_EDGE('',*,*,#2616,.T.);
#3884=ORIENTED_EDGE('',*,*,#2617,.T.);
#3885=ORIENTED_EDGE('',*,*,#2618,.T.);
#3886=ORIENTED_EDGE('',*,*,#2619,.T.);
#3887=ORIENTED_EDGE('',*,*,#2620,.T.);
#3888=ORIENTED_EDGE('',*,*,#2512,.T.);
#3889=ORIENTED_EDGE('',*,*,#2621,.T.);
#3890=ORIENTED_EDGE('',*,*,#2622,.T.);
#3891=ORIENTED_EDGE('',*,*,#2623,.T.);
#3892=ORIENTED_EDGE('',*,*,#2621,.F.);
#3893=ORIENTED_EDGE('',*,*,#2623,.F.);
#3894=ORIENTED_EDGE('',*,*,#2624,.T.);
#3895=ORIENTED_EDGE('',*,*,#2625,.F.);
#3896=ORIENTED_EDGE('',*,*,#2626,.F.);
#3897=ORIENTED_EDGE('',*,*,#2624,.F.);
#3898=ORIENTED_EDGE('',*,*,#2622,.F.);
#3899=ORIENTED_EDGE('',*,*,#2368,.T.);
#3900=ORIENTED_EDGE('',*,*,#2367,.T.);
#3901=ORIENTED_EDGE('',*,*,#2366,.T.);
#3902=ORIENTED_EDGE('',*,*,#2612,.T.);
#3903=ORIENTED_EDGE('',*,*,#2627,.T.);
#3904=ORIENTED_EDGE('',*,*,#2625,.T.);
#3905=ORIENTED_EDGE('',*,*,#2626,.T.);
#3906=ORIENTED_EDGE('',*,*,#2627,.F.);
#3907=ORIENTED_EDGE('',*,*,#2393,.F.);
#3908=ORIENTED_EDGE('',*,*,#2611,.F.);
#3909=ORIENTED_EDGE('',*,*,#2526,.F.);
#3910=ORIENTED_EDGE('',*,*,#2377,.F.);
#3911=ORIENTED_EDGE('',*,*,#2613,.F.);
#3912=ORIENTED_EDGE('',*,*,#2628,.T.);
#3913=ORIENTED_EDGE('',*,*,#2513,.F.);
#3914=ORIENTED_EDGE('',*,*,#2628,.F.);
#3915=ORIENTED_EDGE('',*,*,#2620,.F.);
#3916=ORIENTED_EDGE('',*,*,#2629,.T.);
#3917=ORIENTED_EDGE('',*,*,#2520,.F.);
#3918=ORIENTED_EDGE('',*,*,#2629,.F.);
#3919=ORIENTED_EDGE('',*,*,#2619,.F.);
#3920=ORIENTED_EDGE('',*,*,#2630,.T.);
#3921=ORIENTED_EDGE('',*,*,#2514,.F.);
#3922=ORIENTED_EDGE('',*,*,#2630,.F.);
#3923=ORIENTED_EDGE('',*,*,#2618,.F.);
#3924=ORIENTED_EDGE('',*,*,#2631,.T.);
#3925=ORIENTED_EDGE('',*,*,#2519,.F.);
#3926=ORIENTED_EDGE('',*,*,#2631,.F.);
#3927=ORIENTED_EDGE('',*,*,#2617,.F.);
#3928=ORIENTED_EDGE('',*,*,#2632,.T.);
#3929=ORIENTED_EDGE('',*,*,#2515,.F.);
#3930=ORIENTED_EDGE('',*,*,#2632,.F.);
#3931=ORIENTED_EDGE('',*,*,#2616,.F.);
#3932=ORIENTED_EDGE('',*,*,#2633,.T.);
#3933=ORIENTED_EDGE('',*,*,#2518,.F.);
#3934=ORIENTED_EDGE('',*,*,#2633,.F.);
#3935=ORIENTED_EDGE('',*,*,#2615,.F.);
#3936=ORIENTED_EDGE('',*,*,#2634,.T.);
#3937=ORIENTED_EDGE('',*,*,#2516,.F.);
#3938=ORIENTED_EDGE('',*,*,#2634,.F.);
#3939=ORIENTED_EDGE('',*,*,#2614,.F.);
#3940=ORIENTED_EDGE('',*,*,#2635,.T.);
#3941=ORIENTED_EDGE('',*,*,#2517,.F.);
#3942=ORIENTED_EDGE('',*,*,#2635,.F.);
#3943=ORIENTED_EDGE('',*,*,#2636,.F.);
#3944=ORIENTED_EDGE('',*,*,#2637,.F.);
#3945=ORIENTED_EDGE('',*,*,#2638,.F.);
#3946=ORIENTED_EDGE('',*,*,#2639,.F.);
#3947=ORIENTED_EDGE('',*,*,#2640,.T.);
#3948=ORIENTED_EDGE('',*,*,#2641,.F.);
#3949=ORIENTED_EDGE('',*,*,#2642,.F.);
#3950=ORIENTED_EDGE('',*,*,#2643,.F.);
#3951=ORIENTED_EDGE('',*,*,#2644,.F.);
#3952=ORIENTED_EDGE('',*,*,#2645,.F.);
#3953=ORIENTED_EDGE('',*,*,#2646,.F.);
#3954=ORIENTED_EDGE('',*,*,#2647,.F.);
#3955=ORIENTED_EDGE('',*,*,#2648,.T.);
#3956=ORIENTED_EDGE('',*,*,#2649,.T.);
#3957=ORIENTED_EDGE('',*,*,#2645,.T.);
#3958=ORIENTED_EDGE('',*,*,#2650,.T.);
#3959=ORIENTED_EDGE('',*,*,#2648,.F.);
#3960=ORIENTED_EDGE('',*,*,#2651,.F.);
#3961=ORIENTED_EDGE('',*,*,#2652,.F.);
#3962=ORIENTED_EDGE('',*,*,#2640,.F.);
#3963=ORIENTED_EDGE('',*,*,#2653,.F.);
#3964=ORIENTED_EDGE('',*,*,#2654,.F.);
#3965=ORIENTED_EDGE('',*,*,#2655,.F.);
#3966=ORIENTED_EDGE('',*,*,#2646,.T.);
#3967=ORIENTED_EDGE('',*,*,#2649,.F.);
#3968=ORIENTED_EDGE('',*,*,#2654,.T.);
#3969=ORIENTED_EDGE('',*,*,#2656,.F.);
#3970=ORIENTED_EDGE('',*,*,#2651,.T.);
#3971=ORIENTED_EDGE('',*,*,#2650,.F.);
#3972=ORIENTED_EDGE('',*,*,#2644,.T.);
#3973=ORIENTED_EDGE('',*,*,#2643,.T.);
#3974=ORIENTED_EDGE('',*,*,#2657,.T.);
#3975=ORIENTED_EDGE('',*,*,#2658,.F.);
#3976=ORIENTED_EDGE('',*,*,#2659,.F.);
#3977=ORIENTED_EDGE('',*,*,#2642,.T.);
#3978=ORIENTED_EDGE('',*,*,#2660,.F.);
#3979=ORIENTED_EDGE('',*,*,#2661,.F.);
#3980=ORIENTED_EDGE('',*,*,#2657,.F.);
#3981=ORIENTED_EDGE('',*,*,#2653,.T.);
#3982=ORIENTED_EDGE('',*,*,#2639,.T.);
#3983=ORIENTED_EDGE('',*,*,#2662,.F.);
#3984=ORIENTED_EDGE('',*,*,#2663,.F.);
#3985=ORIENTED_EDGE('',*,*,#2647,.T.);
#3986=ORIENTED_EDGE('',*,*,#2664,.F.);
#3987=ORIENTED_EDGE('',*,*,#2665,.T.);
#3988=ORIENTED_EDGE('',*,*,#2660,.T.);
#3989=ORIENTED_EDGE('',*,*,#2666,.F.);
#3990=ORIENTED_EDGE('',*,*,#2658,.T.);
#3991=ORIENTED_EDGE('',*,*,#2661,.T.);
#3992=ORIENTED_EDGE('',*,*,#2665,.F.);
#3993=ORIENTED_EDGE('',*,*,#2652,.T.);
#3994=ORIENTED_EDGE('',*,*,#2667,.F.);
#3995=ORIENTED_EDGE('',*,*,#2668,.T.);
#3996=ORIENTED_EDGE('',*,*,#2641,.T.);
#3997=ORIENTED_EDGE('',*,*,#2636,.T.);
#3998=ORIENTED_EDGE('',*,*,#2668,.F.);
#3999=ORIENTED_EDGE('',*,*,#2669,.F.);
#4000=ORIENTED_EDGE('',*,*,#2662,.T.);
#4001=ORIENTED_EDGE('',*,*,#2638,.T.);
#4002=ORIENTED_EDGE('',*,*,#2670,.T.);
#4003=ORIENTED_EDGE('',*,*,#2637,.T.);
#4004=ORIENTED_EDGE('',*,*,#2670,.F.);
#4005=ORIENTED_EDGE('',*,*,#2671,.T.);
#4006=ORIENTED_EDGE('',*,*,#2672,.T.);
#4007=ORIENTED_EDGE('',*,*,#2673,.F.);
#4008=ORIENTED_EDGE('',*,*,#2674,.F.);
#4009=ORIENTED_EDGE('',*,*,#2675,.T.);
#4010=ORIENTED_EDGE('',*,*,#2674,.T.);
#4011=ORIENTED_EDGE('',*,*,#2676,.F.);
#4012=ORIENTED_EDGE('',*,*,#2677,.F.);
#4013=ORIENTED_EDGE('',*,*,#2678,.T.);
#4014=ORIENTED_EDGE('',*,*,#2677,.T.);
#4015=ORIENTED_EDGE('',*,*,#2679,.F.);
#4016=ORIENTED_EDGE('',*,*,#2680,.F.);
#4017=ORIENTED_EDGE('',*,*,#2681,.T.);
#4018=ORIENTED_EDGE('',*,*,#2680,.T.);
#4019=ORIENTED_EDGE('',*,*,#2682,.F.);
#4020=ORIENTED_EDGE('',*,*,#2672,.F.);
#4021=ORIENTED_EDGE('',*,*,#2682,.T.);
#4022=ORIENTED_EDGE('',*,*,#2679,.T.);
#4023=ORIENTED_EDGE('',*,*,#2676,.T.);
#4024=ORIENTED_EDGE('',*,*,#2673,.T.);
#4025=ORIENTED_EDGE('',*,*,#2681,.F.);
#4026=ORIENTED_EDGE('',*,*,#2671,.F.);
#4027=ORIENTED_EDGE('',*,*,#2675,.F.);
#4028=ORIENTED_EDGE('',*,*,#2678,.F.);
#4029=ORIENTED_EDGE('',*,*,#2664,.T.);
#4030=ORIENTED_EDGE('',*,*,#2655,.T.);
#4031=ORIENTED_EDGE('',*,*,#2663,.T.);
#4032=ORIENTED_EDGE('',*,*,#2669,.T.);
#4033=ORIENTED_EDGE('',*,*,#2667,.T.);
#4034=ORIENTED_EDGE('',*,*,#2656,.T.);
#4035=ORIENTED_EDGE('',*,*,#2659,.T.);
#4036=ORIENTED_EDGE('',*,*,#2666,.T.);
#4037=CYLINDRICAL_SURFACE('',#4481,5.);
#4038=CYLINDRICAL_SURFACE('',#4482,5.);
#4039=CYLINDRICAL_SURFACE('',#4490,25.);
#4040=CYLINDRICAL_SURFACE('',#4497,28.);
#4041=CYLINDRICAL_SURFACE('',#4508,24.5);
#4042=CYLINDRICAL_SURFACE('',#4514,4.);
#4043=CYLINDRICAL_SURFACE('',#4517,10.);
#4044=CYLINDRICAL_SURFACE('',#4523,4.085);
#4045=CYLINDRICAL_SURFACE('',#4525,4.085);
#4046=CYLINDRICAL_SURFACE('',#4526,4.085);
#4047=CYLINDRICAL_SURFACE('',#4527,4.085);
#4048=CYLINDRICAL_SURFACE('',#4528,4.085);
#4049=CYLINDRICAL_SURFACE('',#4529,4.085);
#4050=CYLINDRICAL_SURFACE('',#4530,4.085);
#4051=CYLINDRICAL_SURFACE('',#4531,4.085);
#4052=CYLINDRICAL_SURFACE('',#4533,3.38975);
#4053=CYLINDRICAL_SURFACE('',#4535,3.38975);
#4054=CYLINDRICAL_SURFACE('',#4536,3.38975);
#4055=CYLINDRICAL_SURFACE('',#4537,3.38975);
#4056=CYLINDRICAL_SURFACE('',#4538,3.38975);
#4057=CYLINDRICAL_SURFACE('',#4539,3.38975);
#4058=CYLINDRICAL_SURFACE('',#4540,3.38975);
#4059=CYLINDRICAL_SURFACE('',#4541,3.38975);
#4060=CYLINDRICAL_SURFACE('',#4545,3.38975);
#4061=CYLINDRICAL_SURFACE('',#4546,4.085);
#4062=CYLINDRICAL_SURFACE('',#4548,8.);
#4063=CYLINDRICAL_SURFACE('',#4555,5.);
#4064=CYLINDRICAL_SURFACE('',#4558,3.22275);
#4065=CYLINDRICAL_SURFACE('',#4560,3.22275);
#4066=CYLINDRICAL_SURFACE('',#4561,3.22275);
#4067=CYLINDRICAL_SURFACE('',#4562,3.22275);
#4068=CYLINDRICAL_SURFACE('',#4563,3.22275);
#4069=CYLINDRICAL_SURFACE('',#4564,3.22275);
#4070=CYLINDRICAL_SURFACE('',#4565,3.933);
#4071=CYLINDRICAL_SURFACE('',#4568,3.22275);
#4072=CYLINDRICAL_SURFACE('',#4572,3.);
#4073=CYLINDRICAL_SURFACE('',#4576,24.5);
#4074=CYLINDRICAL_SURFACE('',#4580,3.22275);
#4075=CYLINDRICAL_SURFACE('',#4582,3.22275);
#4076=CYLINDRICAL_SURFACE('',#4583,3.22275);
#4077=CYLINDRICAL_SURFACE('',#4584,3.22275);
#4078=CYLINDRICAL_SURFACE('',#4585,3.22275);
#4079=CYLINDRICAL_SURFACE('',#4586,3.22275);
#4080=CYLINDRICAL_SURFACE('',#4587,3.22275);
#4081=CYLINDRICAL_SURFACE('',#4588,3.22275);
#4082=CYLINDRICAL_SURFACE('',#4589,3.933);
#4083=CYLINDRICAL_SURFACE('',#4593,3.22275);
#4084=CYLINDRICAL_SURFACE('',#4597,3.);
#4085=CYLINDRICAL_SURFACE('',#4599,24.5);
#4086=CYLINDRICAL_SURFACE('',#4605,4.085);
#4087=CYLINDRICAL_SURFACE('',#4607,4.085);
#4088=CYLINDRICAL_SURFACE('',#4608,4.085);
#4089=CYLINDRICAL_SURFACE('',#4609,4.085);
#4090=CYLINDRICAL_SURFACE('',#4610,4.085);
#4091=CYLINDRICAL_SURFACE('',#4611,4.085);
#4092=CYLINDRICAL_SURFACE('',#4612,4.085);
#4093=CYLINDRICAL_SURFACE('',#4613,4.085);
#4094=CYLINDRICAL_SURFACE('',#4614,4.085);
#4095=CYLINDRICAL_SURFACE('',#4616,3.38975);
#4096=CYLINDRICAL_SURFACE('',#4619,4.085);
#4097=CYLINDRICAL_SURFACE('',#4623,5.);
#4098=CYLINDRICAL_SURFACE('',#4626,5.);
#4099=CYLINDRICAL_SURFACE('',#4627,5.);
#4100=CYLINDRICAL_SURFACE('',#4628,5.);
#4101=CYLINDRICAL_SURFACE('',#4629,4.);
#4102=CYLINDRICAL_SURFACE('',#4632,31.);
#4103=CYLINDRICAL_SURFACE('',#4634,4.);
#4104=CYLINDRICAL_SURFACE('',#4637,31.);
#4105=CYLINDRICAL_SURFACE('',#4764,6.5);
#4106=CYLINDRICAL_SURFACE('',#4766,4.);
#4107=CYLINDRICAL_SURFACE('',#4768,31.);
#4108=CYLINDRICAL_SURFACE('',#4770,4.);
#4109=CYLINDRICAL_SURFACE('',#4772,6.5);
#4110=CYLINDRICAL_SURFACE('',#4774,4.);
#4111=CYLINDRICAL_SURFACE('',#4776,31.);
#4112=CYLINDRICAL_SURFACE('',#4778,4.);
#4113=CYLINDRICAL_SURFACE('',#4780,6.5);
#4114=CYLINDRICAL_SURFACE('',#4782,4.);
#4115=CYLINDRICAL_SURFACE('',#4784,31.);
#4116=CYLINDRICAL_SURFACE('',#4786,4.);
#4117=CYLINDRICAL_SURFACE('',#4788,6.5);
#4118=CYLINDRICAL_SURFACE('',#4790,4.);
#4119=CYLINDRICAL_SURFACE('',#4792,31.);
#4120=CYLINDRICAL_SURFACE('',#4914,4.);
#4121=CYLINDRICAL_SURFACE('',#4915,31.);
#4122=CYLINDRICAL_SURFACE('',#4916,6.5);
#4123=CYLINDRICAL_SURFACE('',#4917,4.);
#4124=CYLINDRICAL_SURFACE('',#4918,31.);
#4125=CYLINDRICAL_SURFACE('',#4919,4.);
#4126=CYLINDRICAL_SURFACE('',#4920,6.5);
#4127=CYLINDRICAL_SURFACE('',#4921,4.);
#4128=CYLINDRICAL_SURFACE('',#4922,31.);
#4129=CYLINDRICAL_SURFACE('',#4923,4.);
#4130=CYLINDRICAL_SURFACE('',#4924,6.5);
#4131=CYLINDRICAL_SURFACE('',#4925,4.);
#4132=CYLINDRICAL_SURFACE('',#4926,31.);
#4133=CYLINDRICAL_SURFACE('',#4927,4.);
#4134=CYLINDRICAL_SURFACE('',#4942,28.);
#4135=CYLINDRICAL_SURFACE('',#4947,6.5);
#4136=CYLINDRICAL_SURFACE('',#4948,1.5);
#4137=CYLINDRICAL_SURFACE('',#4949,1.5);
#4138=CYLINDRICAL_SURFACE('',#4950,1.5);
#4139=CYLINDRICAL_SURFACE('',#4951,1.5);
#4140=CYLINDRICAL_SURFACE('',#4952,1.5);
#4141=CYLINDRICAL_SURFACE('',#4953,1.5);
#4142=CYLINDRICAL_SURFACE('',#4954,1.5);
#4143=CYLINDRICAL_SURFACE('',#4955,1.5);
#4144=CYLINDRICAL_SURFACE('',#4960,241.305156942645);
#4145=CYLINDRICAL_SURFACE('',#4965,5.);
#4146=CYLINDRICAL_SURFACE('',#4966,238.305156942645);
#4147=CYLINDRICAL_SURFACE('',#4978,5.);
#4148=CYLINDRICAL_SURFACE('',#4981,5.);
#4149=CYLINDRICAL_SURFACE('',#4986,6.);
#4150=CYLINDRICAL_SURFACE('',#4990,6.);
#4151=ADVANCED_FACE('',(#516),#4037,.F.);
#4152=ADVANCED_FACE('',(#517),#4038,.F.);
#4153=ADVANCED_FACE('',(#518),#446,.T.);
#4154=ADVANCED_FACE('',(#519,#89),#125,.T.);
#4155=ADVANCED_FACE('',(#520,#90,#91),#4039,.F.);
#4156=ADVANCED_FACE('',(#521),#447,.T.);
#4157=ADVANCED_FACE('',(#522,#92,#93),#4040,.T.);
#4158=ADVANCED_FACE('',(#523),#448,.T.);
#4159=ADVANCED_FACE('',(#524,#94),#126,.F.);
#4160=ADVANCED_FACE('',(#525),#449,.T.);
#4161=ADVANCED_FACE('',(#526),#4041,.T.);
#4162=ADVANCED_FACE('',(#527),#127,.T.);
#4163=ADVANCED_FACE('',(#528),#128,.F.);
#4164=ADVANCED_FACE('',(#529),#4042,.F.);
#4165=ADVANCED_FACE('',(#530),#4043,.T.);
#4166=ADVANCED_FACE('',(#531,#95),#129,.T.);
#4167=ADVANCED_FACE('',(#532,#96),#130,.F.);
#4168=ADVANCED_FACE('',(#533),#4044,.F.);
#4169=ADVANCED_FACE('',(#534),#4045,.F.);
#4170=ADVANCED_FACE('',(#535),#4046,.F.);
#4171=ADVANCED_FACE('',(#536),#4047,.F.);
#4172=ADVANCED_FACE('',(#537),#4048,.F.);
#4173=ADVANCED_FACE('',(#538),#4049,.F.);
#4174=ADVANCED_FACE('',(#539),#4050,.F.);
#4175=ADVANCED_FACE('',(#540),#4051,.F.);
#4176=ADVANCED_FACE('',(#541),#4052,.F.);
#4177=ADVANCED_FACE('',(#542),#4053,.F.);
#4178=ADVANCED_FACE('',(#543),#4054,.F.);
#4179=ADVANCED_FACE('',(#544),#4055,.F.);
#4180=ADVANCED_FACE('',(#545),#4056,.F.);
#4181=ADVANCED_FACE('',(#546),#4057,.F.);
#4182=ADVANCED_FACE('',(#547),#4058,.F.);
#4183=ADVANCED_FACE('',(#548),#4059,.F.);
#4184=ADVANCED_FACE('',(#549),#4060,.F.);
#4185=ADVANCED_FACE('',(#550),#4061,.F.);
#4186=ADVANCED_FACE('',(#551),#45,.F.);
#4187=ADVANCED_FACE('',(#552),#131,.T.);
#4188=ADVANCED_FACE('',(#553),#46,.F.);
#4189=ADVANCED_FACE('',(#554),#4062,.T.);
#4190=ADVANCED_FACE('',(#555,#97),#132,.F.);
#4191=ADVANCED_FACE('',(#556,#98),#133,.F.);
#4192=ADVANCED_FACE('',(#557),#4063,.T.);
#4193=ADVANCED_FACE('',(#558,#99),#134,.T.);
#4194=ADVANCED_FACE('',(#559),#4064,.T.);
#4195=ADVANCED_FACE('',(#560),#4065,.T.);
#4196=ADVANCED_FACE('',(#561),#4066,.T.);
#4197=ADVANCED_FACE('',(#562),#4067,.T.);
#4198=ADVANCED_FACE('',(#563),#4068,.T.);
#4199=ADVANCED_FACE('',(#564),#4069,.T.);
#4200=ADVANCED_FACE('',(#565),#4070,.T.);
#4201=ADVANCED_FACE('',(#566),#4071,.T.);
#4202=ADVANCED_FACE('',(#567),#47,.F.);
#4203=ADVANCED_FACE('',(#568),#135,.F.);
#4204=ADVANCED_FACE('',(#569),#4072,.T.);
#4205=ADVANCED_FACE('',(#570),#48,.F.);
#4206=ADVANCED_FACE('',(#571),#136,.T.);
#4207=ADVANCED_FACE('',(#572),#4073,.F.);
#4208=ADVANCED_FACE('',(#573),#49,.F.);
#4209=ADVANCED_FACE('',(#574),#50,.F.);
#4210=ADVANCED_FACE('',(#575,#100),#137,.F.);
#4211=ADVANCED_FACE('',(#576),#138,.T.);
#4212=ADVANCED_FACE('',(#577),#4074,.T.);
#4213=ADVANCED_FACE('',(#578),#4075,.T.);
#4214=ADVANCED_FACE('',(#579),#4076,.T.);
#4215=ADVANCED_FACE('',(#580),#4077,.T.);
#4216=ADVANCED_FACE('',(#581),#4078,.T.);
#4217=ADVANCED_FACE('',(#582),#4079,.T.);
#4218=ADVANCED_FACE('',(#583),#4080,.T.);
#4219=ADVANCED_FACE('',(#584),#4081,.T.);
#4220=ADVANCED_FACE('',(#585),#4082,.T.);
#4221=ADVANCED_FACE('',(#586),#4083,.T.);
#4222=ADVANCED_FACE('',(#587),#51,.F.);
#4223=ADVANCED_FACE('',(#588),#139,.T.);
#4224=ADVANCED_FACE('',(#589),#4084,.T.);
#4225=ADVANCED_FACE('',(#590),#52,.F.);
#4226=ADVANCED_FACE('',(#591),#4085,.F.);
#4227=ADVANCED_FACE('',(#592),#140,.F.);
#4228=ADVANCED_FACE('',(#593),#53,.F.);
#4229=ADVANCED_FACE('',(#594),#54,.F.);
#4230=ADVANCED_FACE('',(#595,#101),#141,.F.);
#4231=ADVANCED_FACE('',(#596),#142,.T.);
#4232=ADVANCED_FACE('',(#597),#4086,.F.);
#4233=ADVANCED_FACE('',(#598),#4087,.F.);
#4234=ADVANCED_FACE('',(#599),#4088,.F.);
#4235=ADVANCED_FACE('',(#600),#4089,.F.);
#4236=ADVANCED_FACE('',(#601),#4090,.F.);
#4237=ADVANCED_FACE('',(#602),#4091,.F.);
#4238=ADVANCED_FACE('',(#603),#4092,.F.);
#4239=ADVANCED_FACE('',(#604),#4093,.F.);
#4240=ADVANCED_FACE('',(#605),#4094,.F.);
#4241=ADVANCED_FACE('',(#606),#4095,.F.);
#4242=ADVANCED_FACE('',(#607),#4096,.F.);
#4243=ADVANCED_FACE('',(#608),#55,.F.);
#4244=ADVANCED_FACE('',(#609),#56,.F.);
#4245=ADVANCED_FACE('',(#610,#102),#143,.T.);
#4246=ADVANCED_FACE('',(#611),#4097,.T.);
#4247=ADVANCED_FACE('',(#612,#103),#144,.F.);
#4248=ADVANCED_FACE('',(#613),#4098,.F.);
#4249=ADVANCED_FACE('',(#614),#4099,.F.);
#4250=ADVANCED_FACE('',(#615),#4100,.F.);
#4251=ADVANCED_FACE('',(#616),#4101,.F.);
#4252=ADVANCED_FACE('',(#617),#4102,.T.);
#4253=ADVANCED_FACE('',(#618),#4103,.F.);
#4254=ADVANCED_FACE('',(#619),#4104,.T.);
#4255=ADVANCED_FACE('',(#620),#450,.T.);
#4256=ADVANCED_FACE('',(#621),#451,.T.);
#4257=ADVANCED_FACE('',(#622),#452,.T.);
#4258=ADVANCED_FACE('',(#623),#453,.T.);
#4259=ADVANCED_FACE('',(#624),#454,.T.);
#4260=ADVANCED_FACE('',(#625),#455,.T.);
#4261=ADVANCED_FACE('',(#626),#456,.T.);
#4262=ADVANCED_FACE('',(#627),#457,.T.);
#4263=ADVANCED_FACE('',(#628),#458,.T.);
#4264=ADVANCED_FACE('',(#629),#459,.T.);
#4265=ADVANCED_FACE('',(#630),#460,.T.);
#4266=ADVANCED_FACE('',(#631),#461,.T.);
#4267=ADVANCED_FACE('',(#632),#462,.T.);
#4268=ADVANCED_FACE('',(#633),#463,.T.);
#4269=ADVANCED_FACE('',(#634),#464,.T.);
#4270=ADVANCED_FACE('',(#635),#465,.T.);
#4271=ADVANCED_FACE('',(#636),#466,.T.);
#4272=ADVANCED_FACE('',(#637),#467,.T.);
#4273=ADVANCED_FACE('',(#638),#468,.T.);
#4274=ADVANCED_FACE('',(#639),#469,.T.);
#4275=ADVANCED_FACE('',(#640),#470,.T.);
#4276=ADVANCED_FACE('',(#641),#471,.T.);
#4277=ADVANCED_FACE('',(#642),#472,.T.);
#4278=ADVANCED_FACE('',(#643),#473,.T.);
#4279=ADVANCED_FACE('',(#644),#474,.T.);
#4280=ADVANCED_FACE('',(#645),#475,.T.);
#4281=ADVANCED_FACE('',(#646),#476,.T.);
#4282=ADVANCED_FACE('',(#647),#477,.T.);
#4283=ADVANCED_FACE('',(#648),#478,.T.);
#4284=ADVANCED_FACE('',(#649),#479,.T.);
#4285=ADVANCED_FACE('',(#650),#480,.T.);
#4286=ADVANCED_FACE('',(#651),#481,.T.);
#4287=ADVANCED_FACE('',(#652),#4105,.T.);
#4288=ADVANCED_FACE('',(#653),#4106,.F.);
#4289=ADVANCED_FACE('',(#654),#4107,.T.);
#4290=ADVANCED_FACE('',(#655),#4108,.F.);
#4291=ADVANCED_FACE('',(#656),#4109,.T.);
#4292=ADVANCED_FACE('',(#657),#4110,.F.);
#4293=ADVANCED_FACE('',(#658),#4111,.T.);
#4294=ADVANCED_FACE('',(#659),#4112,.F.);
#4295=ADVANCED_FACE('',(#660),#4113,.T.);
#4296=ADVANCED_FACE('',(#661),#4114,.F.);
#4297=ADVANCED_FACE('',(#662),#4115,.T.);
#4298=ADVANCED_FACE('',(#663),#4116,.F.);
#4299=ADVANCED_FACE('',(#664),#4117,.T.);
#4300=ADVANCED_FACE('',(#665),#4118,.F.);
#4301=ADVANCED_FACE('',(#666),#4119,.T.);
#4302=ADVANCED_FACE('',(#667,#104,#105,#106,#107,#108,#109,#110,#111,#112),
#145,.T.);
#4303=ADVANCED_FACE('',(#668),#482,.T.);
#4304=ADVANCED_FACE('',(#669),#483,.T.);
#4305=ADVANCED_FACE('',(#670),#484,.T.);
#4306=ADVANCED_FACE('',(#671),#485,.T.);
#4307=ADVANCED_FACE('',(#672),#486,.T.);
#4308=ADVANCED_FACE('',(#673),#487,.T.);
#4309=ADVANCED_FACE('',(#674),#488,.T.);
#4310=ADVANCED_FACE('',(#675),#489,.T.);
#4311=ADVANCED_FACE('',(#676),#490,.T.);
#4312=ADVANCED_FACE('',(#677),#491,.T.);
#4313=ADVANCED_FACE('',(#678),#492,.T.);
#4314=ADVANCED_FACE('',(#679),#493,.T.);
#4315=ADVANCED_FACE('',(#680),#494,.T.);
#4316=ADVANCED_FACE('',(#681),#495,.T.);
#4317=ADVANCED_FACE('',(#682),#496,.T.);
#4318=ADVANCED_FACE('',(#683),#497,.T.);
#4319=ADVANCED_FACE('',(#684),#498,.T.);
#4320=ADVANCED_FACE('',(#685),#499,.T.);
#4321=ADVANCED_FACE('',(#686),#500,.T.);
#4322=ADVANCED_FACE('',(#687),#501,.T.);
#4323=ADVANCED_FACE('',(#688),#502,.T.);
#4324=ADVANCED_FACE('',(#689),#503,.T.);
#4325=ADVANCED_FACE('',(#690),#504,.T.);
#4326=ADVANCED_FACE('',(#691),#505,.T.);
#4327=ADVANCED_FACE('',(#692),#506,.T.);
#4328=ADVANCED_FACE('',(#693),#507,.T.);
#4329=ADVANCED_FACE('',(#694),#508,.T.);
#4330=ADVANCED_FACE('',(#695),#509,.T.);
#4331=ADVANCED_FACE('',(#696),#510,.T.);
#4332=ADVANCED_FACE('',(#697),#511,.T.);
#4333=ADVANCED_FACE('',(#698),#512,.T.);
#4334=ADVANCED_FACE('',(#699),#513,.T.);
#4335=ADVANCED_FACE('',(#700),#4120,.F.);
#4336=ADVANCED_FACE('',(#701),#4121,.T.);
#4337=ADVANCED_FACE('',(#702),#4122,.T.);
#4338=ADVANCED_FACE('',(#703),#4123,.F.);
#4339=ADVANCED_FACE('',(#704),#4124,.T.);
#4340=ADVANCED_FACE('',(#705),#4125,.F.);
#4341=ADVANCED_FACE('',(#706),#4126,.T.);
#4342=ADVANCED_FACE('',(#707),#4127,.F.);
#4343=ADVANCED_FACE('',(#708),#4128,.T.);
#4344=ADVANCED_FACE('',(#709),#4129,.F.);
#4345=ADVANCED_FACE('',(#710),#4130,.T.);
#4346=ADVANCED_FACE('',(#711),#4131,.F.);
#4347=ADVANCED_FACE('',(#712),#4132,.T.);
#4348=ADVANCED_FACE('',(#713),#4133,.F.);
#4349=ADVANCED_FACE('',(#714,#113,#114,#115,#116,#117,#118,#119,#120,#121),
#146,.F.);
#4350=ADVANCED_FACE('',(#715),#514,.T.);
#4351=ADVANCED_FACE('',(#716,#122,#123),#4134,.F.);
#4352=ADVANCED_FACE('',(#717),#515,.T.);
#4353=ADVANCED_FACE('',(#718),#4135,.T.);
#4354=ADVANCED_FACE('',(#719),#4136,.F.);
#4355=ADVANCED_FACE('',(#720),#4137,.F.);
#4356=ADVANCED_FACE('',(#721),#4138,.F.);
#4357=ADVANCED_FACE('',(#722),#4139,.F.);
#4358=ADVANCED_FACE('',(#723),#4140,.F.);
#4359=ADVANCED_FACE('',(#724),#4141,.F.);
#4360=ADVANCED_FACE('',(#725),#4142,.F.);
#4361=ADVANCED_FACE('',(#726),#4143,.F.);
#4362=ADVANCED_FACE('',(#727),#147,.T.);
#4363=ADVANCED_FACE('',(#728),#4144,.T.);
#4364=ADVANCED_FACE('',(#729),#4145,.T.);
#4365=ADVANCED_FACE('',(#730),#4146,.F.);
#4366=ADVANCED_FACE('',(#731),#148,.F.);
#4367=ADVANCED_FACE('',(#732),#149,.T.);
#4368=ADVANCED_FACE('',(#733),#150,.F.);
#4369=ADVANCED_FACE('',(#734),#151,.F.);
#4370=ADVANCED_FACE('',(#735),#152,.F.);
#4371=ADVANCED_FACE('',(#736),#153,.F.);
#4372=ADVANCED_FACE('',(#737),#4147,.F.);
#4373=ADVANCED_FACE('',(#738),#154,.F.);
#4374=ADVANCED_FACE('',(#739),#4148,.F.);
#4375=ADVANCED_FACE('',(#740),#155,.F.);
#4376=ADVANCED_FACE('',(#741),#156,.T.);
#4377=ADVANCED_FACE('',(#742),#4149,.T.);
#4378=ADVANCED_FACE('',(#743),#157,.T.);
#4379=ADVANCED_FACE('',(#744),#4150,.T.);
#4380=ADVANCED_FACE('',(#745),#158,.T.);
#4381=ADVANCED_FACE('',(#746,#124),#159,.F.);
#4382=CLOSED_SHELL('',(#4151,#4152,#4153,#4154,#4155,#4156,#4157,#4158,
#4159,#4160));
#4383=CLOSED_SHELL('',(#4161,#4162,#4163));
#4384=CLOSED_SHELL('',(#4164,#4165,#4166,#4167));
#4385=CLOSED_SHELL('',(#4168,#4169,#4170,#4171,#4172,#4173,#4174,#4175,
#4176,#4177,#4178,#4179,#4180,#4181,#4182,#4183,#4184,#4185,#4186,#4187,
#4188,#4189,#4190,#4191,#4192,#4193));
#4386=CLOSED_SHELL('',(#4194,#4195,#4196,#4197,#4198,#4199,#4200,#4201,
#4202,#4203,#4204,#4205,#4206,#4207,#4208,#4209,#4210,#4211));
#4387=CLOSED_SHELL('',(#4212,#4213,#4214,#4215,#4216,#4217,#4218,#4219,
#4220,#4221,#4222,#4223,#4224,#4225,#4226,#4227,#4228,#4229,#4230,#4231));
#4388=CLOSED_SHELL('',(#4232,#4233,#4234,#4235,#4236,#4237,#4238,#4239,
#4240,#4241,#4242,#4243,#4244,#4245,#4246,#4247,#4248,#4249,#4250,#4251,
#4252,#4253,#4254,#4255,#4256,#4257,#4258,#4259,#4260,#4261,#4262,#4263,
#4264,#4265,#4266,#4267,#4268,#4269,#4270,#4271,#4272,#4273,#4274,#4275,
#4276,#4277,#4278,#4279,#4280,#4281,#4282,#4283,#4284,#4285,#4286,#4287,
#4288,#4289,#4290,#4291,#4292,#4293,#4294,#4295,#4296,#4297,#4298,#4299,
#4300,#4301,#4302,#4303,#4304,#4305,#4306,#4307,#4308,#4309,#4310,#4311,
#4312,#4313,#4314,#4315,#4316,#4317,#4318,#4319,#4320,#4321,#4322,#4323,
#4324,#4325,#4326,#4327,#4328,#4329,#4330,#4331,#4332,#4333,#4334,#4335,
#4336,#4337,#4338,#4339,#4340,#4341,#4342,#4343,#4344,#4345,#4346,#4347,
#4348,#4349,#4350,#4351,#4352,#4353,#4354,#4355,#4356,#4357,#4358,#4359,
#4360,#4361));
#4389=CLOSED_SHELL('',(#4362,#4363,#4364,#4365,#4366,#4367,#4368,#4369,
#4370,#4371,#4372,#4373,#4374,#4375,#4376,#4377,#4378,#4379,#4380,#4381));
#4390=DERIVED_UNIT_ELEMENT(#4406,1.);
#4391=DERIVED_UNIT_ELEMENT(#34405,-3.);
#4392=DERIVED_UNIT_ELEMENT(#4406,1.);
#4393=DERIVED_UNIT_ELEMENT(#34405,-3.);
#4394=DERIVED_UNIT_ELEMENT(#4406,1.);
#4395=DERIVED_UNIT_ELEMENT(#34405,-3.);
#4396=DERIVED_UNIT_ELEMENT(#4406,1.);
#4397=DERIVED_UNIT_ELEMENT(#34405,-3.);
#4398=DERIVED_UNIT_ELEMENT(#4406,1.);
#4399=DERIVED_UNIT_ELEMENT(#34405,-3.);
#4400=DERIVED_UNIT_ELEMENT(#4406,1.);
#4401=DERIVED_UNIT_ELEMENT(#34405,-3.);
#4402=DERIVED_UNIT_ELEMENT(#4406,1.);
#4403=DERIVED_UNIT_ELEMENT(#34405,-3.);
#4404=DERIVED_UNIT_ELEMENT(#4406,1.);
#4405=DERIVED_UNIT_ELEMENT(#34405,-3.);
#4406=(
MASS_UNIT()
NAMED_UNIT(*)
SI_UNIT(.KILO.,.GRAM.)
);
#4407=DERIVED_UNIT((#4390,#4391));
#4408=DERIVED_UNIT((#4392,#4393));
#4409=DERIVED_UNIT((#4394,#4395));
#4410=DERIVED_UNIT((#4396,#4397));
#4411=DERIVED_UNIT((#4398,#4399));
#4412=DERIVED_UNIT((#4400,#4401));
#4413=DERIVED_UNIT((#4402,#4403));
#4414=DERIVED_UNIT((#4404,#4405));
#4415=MEASURE_REPRESENTATION_ITEM('density measure',
POSITIVE_RATIO_MEASURE(7850.),#4407);
#4416=MEASURE_REPRESENTATION_ITEM('density measure',
POSITIVE_RATIO_MEASURE(7850.),#4408);
#4417=MEASURE_REPRESENTATION_ITEM('density measure',
POSITIVE_RATIO_MEASURE(7850.),#4409);
#4418=MEASURE_REPRESENTATION_ITEM('density measure',
POSITIVE_RATIO_MEASURE(7850.),#4410);
#4419=MEASURE_REPRESENTATION_ITEM('density measure',
POSITIVE_RATIO_MEASURE(7850.),#4411);
#4420=MEASURE_REPRESENTATION_ITEM('density measure',
POSITIVE_RATIO_MEASURE(7850.),#4412);
#4421=MEASURE_REPRESENTATION_ITEM('density measure',
POSITIVE_RATIO_MEASURE(7850.),#4413);
#4422=MEASURE_REPRESENTATION_ITEM('density measure',
POSITIVE_RATIO_MEASURE(7850.),#4414);
#4423=PROPERTY_DEFINITION_REPRESENTATION(#4463,#4439);
#4424=PROPERTY_DEFINITION_REPRESENTATION(#4464,#4440);
#4425=PROPERTY_DEFINITION_REPRESENTATION(#4465,#4441);
#4426=PROPERTY_DEFINITION_REPRESENTATION(#4466,#4442);
#4427=PROPERTY_DEFINITION_REPRESENTATION(#4467,#4443);
#4428=PROPERTY_DEFINITION_REPRESENTATION(#4468,#4444);
#4429=PROPERTY_DEFINITION_REPRESENTATION(#4469,#4445);
#4430=PROPERTY_DEFINITION_REPRESENTATION(#4470,#4446);
#4431=PROPERTY_DEFINITION_REPRESENTATION(#4471,#4447);
#4432=PROPERTY_DEFINITION_REPRESENTATION(#4472,#4448);
#4433=PROPERTY_DEFINITION_REPRESENTATION(#4473,#4449);
#4434=PROPERTY_DEFINITION_REPRESENTATION(#4474,#4450);
#4435=PROPERTY_DEFINITION_REPRESENTATION(#4475,#4451);
#4436=PROPERTY_DEFINITION_REPRESENTATION(#4476,#4452);
#4437=PROPERTY_DEFINITION_REPRESENTATION(#4477,#4453);
#4438=PROPERTY_DEFINITION_REPRESENTATION(#4478,#4454);
#4439=REPRESENTATION('material name',(#4455),#34395);
#4440=REPRESENTATION('density',(#4415),#34395);
#4441=REPRESENTATION('material name',(#4456),#34396);
#4442=REPRESENTATION('density',(#4416),#34396);
#4443=REPRESENTATION('material name',(#4457),#34397);
#4444=REPRESENTATION('density',(#4417),#34397);
#4445=REPRESENTATION('material name',(#4458),#34398);
#4446=REPRESENTATION('density',(#4418),#34398);
#4447=REPRESENTATION('material name',(#4459),#34399);
#4448=REPRESENTATION('density',(#4419),#34399);
#4449=REPRESENTATION('material name',(#4460),#34400);
#4450=REPRESENTATION('density',(#4420),#34400);
#4451=REPRESENTATION('material name',(#4461),#34401);
#4452=REPRESENTATION('density',(#4421),#34401);
#4453=REPRESENTATION('material name',(#4462),#34402);
#4454=REPRESENTATION('density',(#4422),#34402);
#4455=DESCRIPTIVE_REPRESENTATION_ITEM('Steel','Steel');
#4456=DESCRIPTIVE_REPRESENTATION_ITEM('Steel','Steel');
#4457=DESCRIPTIVE_REPRESENTATION_ITEM('Steel','Steel');
#4458=DESCRIPTIVE_REPRESENTATION_ITEM('Steel','Steel');
#4459=DESCRIPTIVE_REPRESENTATION_ITEM('Steel','Steel');
#4460=DESCRIPTIVE_REPRESENTATION_ITEM('Steel','Steel');
#4461=DESCRIPTIVE_REPRESENTATION_ITEM('Steel','Steel');
#4462=DESCRIPTIVE_REPRESENTATION_ITEM('Steel','Steel');
#4463=PROPERTY_DEFINITION('material property','material name',#34445);
#4464=PROPERTY_DEFINITION('material property','density of part',#34445);
#4465=PROPERTY_DEFINITION('material property','material name',#34446);
#4466=PROPERTY_DEFINITION('material property','density of part',#34446);
#4467=PROPERTY_DEFINITION('material property','material name',#34447);
#4468=PROPERTY_DEFINITION('material property','density of part',#34447);
#4469=PROPERTY_DEFINITION('material property','material name',#34448);
#4470=PROPERTY_DEFINITION('material property','density of part',#34448);
#4471=PROPERTY_DEFINITION('material property','material name',#34449);
#4472=PROPERTY_DEFINITION('material property','density of part',#34449);
#4473=PROPERTY_DEFINITION('material property','material name',#34450);
#4474=PROPERTY_DEFINITION('material property','density of part',#34450);
#4475=PROPERTY_DEFINITION('material property','material name',#34451);
#4476=PROPERTY_DEFINITION('material property','density of part',#34451);
#4477=PROPERTY_DEFINITION('material property','material name',#34452);
#4478=PROPERTY_DEFINITION('material property','density of part',#34452);
#4479=AXIS2_PLACEMENT_3D('',#6188,#5003,#5004);
#4480=AXIS2_PLACEMENT_3D('',#6189,#5005,#5006);
#4481=AXIS2_PLACEMENT_3D('',#6190,#5007,#5008);
#4482=AXIS2_PLACEMENT_3D('',#6268,#5010,#5011);
#4483=AXIS2_PLACEMENT_3D('',#6346,#5013,#5014);
#4484=AXIS2_PLACEMENT_3D('',#6348,#5015,#5016);
#4485=AXIS2_PLACEMENT_3D('',#6350,#5017,#5018);
#4486=AXIS2_PLACEMENT_3D('',#6352,#5019,#5020);
#4487=AXIS2_PLACEMENT_3D('',#6353,#5021,#5022);
#4488=AXIS2_PLACEMENT_3D('',#6354,#5023,#5024);
#4489=AXIS2_PLACEMENT_3D('',#6356,#5025,#5026);
#4490=AXIS2_PLACEMENT_3D('',#6357,#5027,#5028);
#4491=AXIS2_PLACEMENT_3D('',#6360,#5029,#5030);
#4492=AXIS2_PLACEMENT_3D('',#6361,#5031,#5032);
#4493=AXIS2_PLACEMENT_3D('',#6363,#5034,#5035);
#4494=AXIS2_PLACEMENT_3D('',#6365,#5036,#5037);
#4495=AXIS2_PLACEMENT_3D('',#6367,#5038,#5039);
#4496=AXIS2_PLACEMENT_3D('',#6368,#5040,#5041);
#4497=AXIS2_PLACEMENT_3D('',#6369,#5042,#5043);
#4498=AXIS2_PLACEMENT_3D('',#6373,#5045,#5046);
#4499=AXIS2_PLACEMENT_3D('',#6374,#5047,#5048);
#4500=AXIS2_PLACEMENT_3D('',#6375,#5049,#5050);
#4501=AXIS2_PLACEMENT_3D('',#6377,#5051,#5052);
#4502=AXIS2_PLACEMENT_3D('',#6378,#5053,#5054);
#4503=AXIS2_PLACEMENT_3D('',#6379,#5055,#5056);
#4504=AXIS2_PLACEMENT_3D('',#6381,#5057,#5058);
#4505=AXIS2_PLACEMENT_3D('',#6382,#5059,#5060);
#4506=AXIS2_PLACEMENT_3D('',#6383,#5061,#5062);
#4507=AXIS2_PLACEMENT_3D('',#6384,#5063,#5064);
#4508=AXIS2_PLACEMENT_3D('',#6385,#5065,#5066);
#4509=AXIS2_PLACEMENT_3D('',#6387,#5067,#5068);
#4510=AXIS2_PLACEMENT_3D('',#6390,#5070,#5071);
#4511=AXIS2_PLACEMENT_3D('',#6391,#5072,#5073);
#4512=AXIS2_PLACEMENT_3D('',#6392,#5074,#5075);
#4513=AXIS2_PLACEMENT_3D('',#6393,#5076,#5077);
#4514=AXIS2_PLACEMENT_3D('',#6394,#5078,#5079);
#4515=AXIS2_PLACEMENT_3D('',#6396,#5080,#5081);
#4516=AXIS2_PLACEMENT_3D('',#6399,#5083,#5084);
#4517=AXIS2_PLACEMENT_3D('',#6400,#5085,#5086);
#4518=AXIS2_PLACEMENT_3D('',#6402,#5087,#5088);
#4519=AXIS2_PLACEMENT_3D('',#6405,#5090,#5091);
#4520=AXIS2_PLACEMENT_3D('',#6406,#5092,#5093);
#4521=AXIS2_PLACEMENT_3D('',#6407,#5094,#5095);
#4522=AXIS2_PLACEMENT_3D('',#6408,#5096,#5097);
#4523=AXIS2_PLACEMENT_3D('',#6409,#5098,#5099);
#4524=AXIS2_PLACEMENT_3D('',#6419,#5101,#5102);
#4525=AXIS2_PLACEMENT_3D('',#6475,#5103,#5104);
#4526=AXIS2_PLACEMENT_3D('',#6909,#5106,#5107);
#4527=AXIS2_PLACEMENT_3D('',#7378,#5109,#5110);
#4528=AXIS2_PLACEMENT_3D('',#7844,#5112,#5113);
#4529=AXIS2_PLACEMENT_3D('',#8316,#5115,#5116);
#4530=AXIS2_PLACEMENT_3D('',#8779,#5118,#5119);
#4531=AXIS2_PLACEMENT_3D('',#9245,#5121,#5122);
#4532=AXIS2_PLACEMENT_3D('',#9293,#5124,#5125);
#4533=AXIS2_PLACEMENT_3D('',#9486,#5126,#5127);
#4534=AXIS2_PLACEMENT_3D('',#9648,#5129,#5130);
#4535=AXIS2_PLACEMENT_3D('',#9862,#5131,#5132);
#4536=AXIS2_PLACEMENT_3D('',#10097,#5134,#5135);
#4537=AXIS2_PLACEMENT_3D('',#10533,#5137,#5138);
#4538=AXIS2_PLACEMENT_3D('',#10925,#5140,#5141);
#4539=AXIS2_PLACEMENT_3D('',#11322,#5143,#5144);
#4540=AXIS2_PLACEMENT_3D('',#11702,#5146,#5147);
#4541=AXIS2_PLACEMENT_3D('',#11892,#5149,#5150);
#4542=AXIS2_PLACEMENT_3D('',#11894,#5151,#5152);
#4543=AXIS2_PLACEMENT_3D('',#11898,#5154,#5155);
#4544=AXIS2_PLACEMENT_3D('',#11953,#5157,#5158);
#4545=AXIS2_PLACEMENT_3D('',#11954,#5159,#5160);
#4546=AXIS2_PLACEMENT_3D('',#12344,#5161,#5162);
#4547=AXIS2_PLACEMENT_3D('',#13222,#5163,#5164);
#4548=AXIS2_PLACEMENT_3D('',#13629,#5165,#5166);
#4549=AXIS2_PLACEMENT_3D('',#13631,#5167,#5168);
#4550=AXIS2_PLACEMENT_3D('',#13634,#5170,#5171);
#4551=AXIS2_PLACEMENT_3D('',#13635,#5172,#5173);
#4552=AXIS2_PLACEMENT_3D('',#13637,#5174,#5175);
#4553=AXIS2_PLACEMENT_3D('',#13638,#5176,#5177);
#4554=AXIS2_PLACEMENT_3D('',#13640,#5178,#5179);
#4555=AXIS2_PLACEMENT_3D('',#13641,#5180,#5181);
#4556=AXIS2_PLACEMENT_3D('',#13643,#5183,#5184);
#4557=AXIS2_PLACEMENT_3D('',#13644,#5185,#5186);
#4558=AXIS2_PLACEMENT_3D('',#13645,#5187,#5188);
#4559=AXIS2_PLACEMENT_3D('',#13761,#5190,#5191);
#4560=AXIS2_PLACEMENT_3D('',#13844,#5192,#5193);
#4561=AXIS2_PLACEMENT_3D('',#14166,#5195,#5196);
#4562=AXIS2_PLACEMENT_3D('',#14488,#5198,#5199);
#4563=AXIS2_PLACEMENT_3D('',#14814,#5201,#5202);
#4564=AXIS2_PLACEMENT_3D('',#15134,#5204,#5205);
#4565=AXIS2_PLACEMENT_3D('',#15456,#5207,#5208);
#4566=AXIS2_PLACEMENT_3D('',#15466,#5209,#5210);
#4567=AXIS2_PLACEMENT_3D('',#16604,#5211,#5212);
#4568=AXIS2_PLACEMENT_3D('',#17899,#5213,#5214);
#4569=AXIS2_PLACEMENT_3D('',#18038,#5215,#5216);
#4570=AXIS2_PLACEMENT_3D('',#18232,#5218,#5219);
#4571=AXIS2_PLACEMENT_3D('',#18236,#5221,#5222);
#4572=AXIS2_PLACEMENT_3D('',#18238,#5224,#5225);
#4573=AXIS2_PLACEMENT_3D('',#18359,#5229,#5230);
#4574=AXIS2_PLACEMENT_3D('',#18441,#5232,#5233);
#4575=AXIS2_PLACEMENT_3D('',#18442,#5234,#5235);
#4576=AXIS2_PLACEMENT_3D('',#18443,#5236,#5237);
#4577=AXIS2_PLACEMENT_3D('',#19189,#5238,#5239);
#4578=AXIS2_PLACEMENT_3D('',#19190,#5240,#5241);
#4579=AXIS2_PLACEMENT_3D('',#19191,#5242,#5243);
#4580=AXIS2_PLACEMENT_3D('',#19192,#5244,#5245);
#4581=AXIS2_PLACEMENT_3D('',#19276,#5247,#5248);
#4582=AXIS2_PLACEMENT_3D('',#19335,#5249,#5250);
#4583=AXIS2_PLACEMENT_3D('',#19563,#5252,#5253);
#4584=AXIS2_PLACEMENT_3D('',#19864,#5255,#5256);
#4585=AXIS2_PLACEMENT_3D('',#20210,#5258,#5259);
#4586=AXIS2_PLACEMENT_3D('',#20562,#5261,#5262);
#4587=AXIS2_PLACEMENT_3D('',#20894,#5264,#5265);
#4588=AXIS2_PLACEMENT_3D('',#21271,#5267,#5268);
#4589=AXIS2_PLACEMENT_3D('',#21617,#5270,#5271);
#4590=AXIS2_PLACEMENT_3D('',#21658,#5272,#5273);
#4591=AXIS2_PLACEMENT_3D('',#21660,#5274,#5275);
#4592=AXIS2_PLACEMENT_3D('',#23053,#5276,#5277);
#4593=AXIS2_PLACEMENT_3D('',#24655,#5278,#5279);
#4594=AXIS2_PLACEMENT_3D('',#24786,#5280,#5281);
#4595=AXIS2_PLACEMENT_3D('',#24988,#5283,#5284);
#4596=AXIS2_PLACEMENT_3D('',#24992,#5286,#5287);
#4597=AXIS2_PLACEMENT_3D('',#24994,#5289,#5290);
#4598=AXIS2_PLACEMENT_3D('',#25115,#5294,#5295);
#4599=AXIS2_PLACEMENT_3D('',#25197,#5297,#5298);
#4600=AXIS2_PLACEMENT_3D('',#25198,#5299,#5300);
#4601=AXIS2_PLACEMENT_3D('',#25199,#5301,#5302);
#4602=AXIS2_PLACEMENT_3D('',#26040,#5303,#5304);
#4603=AXIS2_PLACEMENT_3D('',#26041,#5305,#5306);
#4604=AXIS2_PLACEMENT_3D('',#26042,#5307,#5308);
#4605=AXIS2_PLACEMENT_3D('',#26043,#5309,#5310);
#4606=AXIS2_PLACEMENT_3D('',#26053,#5312,#5313);
#4607=AXIS2_PLACEMENT_3D('',#26109,#5314,#5315);
#4608=AXIS2_PLACEMENT_3D('',#26500,#5317,#5318);
#4609=AXIS2_PLACEMENT_3D('',#26966,#5320,#5321);
#4610=AXIS2_PLACEMENT_3D('',#27432,#5323,#5324);
#4611=AXIS2_PLACEMENT_3D('',#27752,#5326,#5327);
#4612=AXIS2_PLACEMENT_3D('',#28142,#5329,#5330);
#4613=AXIS2_PLACEMENT_3D('',#28608,#5332,#5333);
#4614=AXIS2_PLACEMENT_3D('',#29074,#5335,#5336);
#4615=AXIS2_PLACEMENT_3D('',#29168,#5338,#5339);
#4616=AXIS2_PLACEMENT_3D('',#29319,#5340,#5341);
#4617=AXIS2_PLACEMENT_3D('',#29322,#5342,#5343);
#4618=AXIS2_PLACEMENT_3D('',#30766,#5344,#5345);
#4619=AXIS2_PLACEMENT_3D('',#32200,#5346,#5347);
#4620=AXIS2_PLACEMENT_3D('',#33524,#5348,#5349);
#4621=AXIS2_PLACEMENT_3D('',#33527,#5350,#5351);
#4622=AXIS2_PLACEMENT_3D('',#33528,#5352,#5353);
#4623=AXIS2_PLACEMENT_3D('',#33529,#5354,#5355);
#4624=AXIS2_PLACEMENT_3D('',#33531,#5356,#5357);
#4625=AXIS2_PLACEMENT_3D('',#33588,#5359,#5360);
#4626=AXIS2_PLACEMENT_3D('',#33589,#5361,#5362);
#4627=AXIS2_PLACEMENT_3D('',#33608,#5363,#5364);
#4628=AXIS2_PLACEMENT_3D('',#33628,#5365,#5366);
#4629=AXIS2_PLACEMENT_3D('',#33720,#5368,#5369);
#4630=AXIS2_PLACEMENT_3D('',#33724,#5371,#5372);
#4631=AXIS2_PLACEMENT_3D('',#33728,#5374,#5375);
#4632=AXIS2_PLACEMENT_3D('',#33730,#5377,#5378);
#4633=AXIS2_PLACEMENT_3D('',#33733,#5380,#5381);
#4634=AXIS2_PLACEMENT_3D('',#33734,#5382,#5383);
#4635=AXIS2_PLACEMENT_3D('',#33738,#5385,#5386);
#4636=AXIS2_PLACEMENT_3D('',#33742,#5388,#5389);
#4637=AXIS2_PLACEMENT_3D('',#33744,#5391,#5392);
#4638=AXIS2_PLACEMENT_3D('',#33747,#5394,#5395);
#4639=AXIS2_PLACEMENT_3D('',#33748,#5396,#5397);
#4640=AXIS2_PLACEMENT_3D('',#33750,#5398,#5399);
#4641=AXIS2_PLACEMENT_3D('',#33752,#5400,#5401);
#4642=AXIS2_PLACEMENT_3D('',#33753,#5402,#5403);
#4643=AXIS2_PLACEMENT_3D('',#33754,#5404,#5405);
#4644=AXIS2_PLACEMENT_3D('',#33757,#5406,#5407);
#4645=AXIS2_PLACEMENT_3D('',#33758,#5408,#5409);
#4646=AXIS2_PLACEMENT_3D('',#33759,#5410,#5411);
#4647=AXIS2_PLACEMENT_3D('',#33760,#5412,#5413);
#4648=AXIS2_PLACEMENT_3D('',#33763,#5414,#5415);
#4649=AXIS2_PLACEMENT_3D('',#33764,#5416,#5417);
#4650=AXIS2_PLACEMENT_3D('',#33765,#5418,#5419);
#4651=AXIS2_PLACEMENT_3D('',#33766,#5420,#5421);
#4652=AXIS2_PLACEMENT_3D('',#33769,#5422,#5423);
#4653=AXIS2_PLACEMENT_3D('',#33770,#5424,#5425);
#4654=AXIS2_PLACEMENT_3D('',#33771,#5426,#5427);
#4655=AXIS2_PLACEMENT_3D('',#33772,#5428,#5429);
#4656=AXIS2_PLACEMENT_3D('',#33775,#5430,#5431);
#4657=AXIS2_PLACEMENT_3D('',#33776,#5432,#5433);
#4658=AXIS2_PLACEMENT_3D('',#33777,#5434,#5435);
#4659=AXIS2_PLACEMENT_3D('',#33778,#5436,#5437);
#4660=AXIS2_PLACEMENT_3D('',#33781,#5438,#5439);
#4661=AXIS2_PLACEMENT_3D('',#33782,#5440,#5441);
#4662=AXIS2_PLACEMENT_3D('',#33783,#5442,#5443);
#4663=AXIS2_PLACEMENT_3D('',#33784,#5444,#5445);
#4664=AXIS2_PLACEMENT_3D('',#33787,#5446,#5447);
#4665=AXIS2_PLACEMENT_3D('',#33788,#5448,#5449);
#4666=AXIS2_PLACEMENT_3D('',#33789,#5450,#5451);
#4667=AXIS2_PLACEMENT_3D('',#33790,#5452,#5453);
#4668=AXIS2_PLACEMENT_3D('',#33793,#5454,#5455);
#4669=AXIS2_PLACEMENT_3D('',#33794,#5456,#5457);
#4670=AXIS2_PLACEMENT_3D('',#33795,#5458,#5459);
#4671=AXIS2_PLACEMENT_3D('',#33796,#5460,#5461);
#4672=AXIS2_PLACEMENT_3D('',#33799,#5462,#5463);
#4673=AXIS2_PLACEMENT_3D('',#33800,#5464,#5465);
#4674=AXIS2_PLACEMENT_3D('',#33801,#5466,#5467);
#4675=AXIS2_PLACEMENT_3D('',#33802,#5468,#5469);
#4676=AXIS2_PLACEMENT_3D('',#33805,#5470,#5471);
#4677=AXIS2_PLACEMENT_3D('',#33806,#5472,#5473);
#4678=AXIS2_PLACEMENT_3D('',#33807,#5474,#5475);
#4679=AXIS2_PLACEMENT_3D('',#33808,#5476,#5477);
#4680=AXIS2_PLACEMENT_3D('',#33811,#5478,#5479);
#4681=AXIS2_PLACEMENT_3D('',#33812,#5480,#5481);
#4682=AXIS2_PLACEMENT_3D('',#33813,#5482,#5483);
#4683=AXIS2_PLACEMENT_3D('',#33814,#5484,#5485);
#4684=AXIS2_PLACEMENT_3D('',#33817,#5486,#5487);
#4685=AXIS2_PLACEMENT_3D('',#33818,#5488,#5489);
#4686=AXIS2_PLACEMENT_3D('',#33819,#5490,#5491);
#4687=AXIS2_PLACEMENT_3D('',#33820,#5492,#5493);
#4688=AXIS2_PLACEMENT_3D('',#33823,#5494,#5495);
#4689=AXIS2_PLACEMENT_3D('',#33824,#5496,#5497);
#4690=AXIS2_PLACEMENT_3D('',#33825,#5498,#5499);
#4691=AXIS2_PLACEMENT_3D('',#33826,#5500,#5501);
#4692=AXIS2_PLACEMENT_3D('',#33828,#5502,#5503);
#4693=AXIS2_PLACEMENT_3D('',#33829,#5504,#5505);
#4694=AXIS2_PLACEMENT_3D('',#33830,#5506,#5507);
#4695=AXIS2_PLACEMENT_3D('',#33831,#5508,#5509);
#4696=AXIS2_PLACEMENT_3D('',#33833,#5510,#5511);
#4697=AXIS2_PLACEMENT_3D('',#33834,#5512,#5513);
#4698=AXIS2_PLACEMENT_3D('',#33835,#5514,#5515);
#4699=AXIS2_PLACEMENT_3D('',#33838,#5516,#5517);
#4700=AXIS2_PLACEMENT_3D('',#33839,#5518,#5519);
#4701=AXIS2_PLACEMENT_3D('',#33840,#5520,#5521);
#4702=AXIS2_PLACEMENT_3D('',#33841,#5522,#5523);
#4703=AXIS2_PLACEMENT_3D('',#33844,#5524,#5525);
#4704=AXIS2_PLACEMENT_3D('',#33845,#5526,#5527);
#4705=AXIS2_PLACEMENT_3D('',#33846,#5528,#5529);
#4706=AXIS2_PLACEMENT_3D('',#33847,#5530,#5531);
#4707=AXIS2_PLACEMENT_3D('',#33850,#5532,#5533);
#4708=AXIS2_PLACEMENT_3D('',#33851,#5534,#5535);
#4709=AXIS2_PLACEMENT_3D('',#33852,#5536,#5537);
#4710=AXIS2_PLACEMENT_3D('',#33853,#5538,#5539);
#4711=AXIS2_PLACEMENT_3D('',#33856,#5540,#5541);
#4712=AXIS2_PLACEMENT_3D('',#33857,#5542,#5543);
#4713=AXIS2_PLACEMENT_3D('',#33858,#5544,#5545);
#4714=AXIS2_PLACEMENT_3D('',#33859,#5546,#5547);
#4715=AXIS2_PLACEMENT_3D('',#33862,#5548,#5549);
#4716=AXIS2_PLACEMENT_3D('',#33863,#5550,#5551);
#4717=AXIS2_PLACEMENT_3D('',#33864,#5552,#5553);
#4718=AXIS2_PLACEMENT_3D('',#33865,#5554,#5555);
#4719=AXIS2_PLACEMENT_3D('',#33868,#5556,#5557);
#4720=AXIS2_PLACEMENT_3D('',#33869,#5558,#5559);
#4721=AXIS2_PLACEMENT_3D('',#33870,#5560,#5561);
#4722=AXIS2_PLACEMENT_3D('',#33871,#5562,#5563);
#4723=AXIS2_PLACEMENT_3D('',#33874,#5564,#5565);
#4724=AXIS2_PLACEMENT_3D('',#33875,#5566,#5567);
#4725=AXIS2_PLACEMENT_3D('',#33876,#5568,#5569);
#4726=AXIS2_PLACEMENT_3D('',#33877,#5570,#5571);
#4727=AXIS2_PLACEMENT_3D('',#33880,#5572,#5573);
#4728=AXIS2_PLACEMENT_3D('',#33881,#5574,#5575);
#4729=AXIS2_PLACEMENT_3D('',#33882,#5576,#5577);
#4730=AXIS2_PLACEMENT_3D('',#33883,#5578,#5579);
#4731=AXIS2_PLACEMENT_3D('',#33886,#5580,#5581);
#4732=AXIS2_PLACEMENT_3D('',#33887,#5582,#5583);
#4733=AXIS2_PLACEMENT_3D('',#33888,#5584,#5585);
#4734=AXIS2_PLACEMENT_3D('',#33889,#5586,#5587);
#4735=AXIS2_PLACEMENT_3D('',#33892,#5588,#5589);
#4736=AXIS2_PLACEMENT_3D('',#33893,#5590,#5591);
#4737=AXIS2_PLACEMENT_3D('',#33894,#5592,#5593);
#4738=AXIS2_PLACEMENT_3D('',#33895,#5594,#5595);
#4739=AXIS2_PLACEMENT_3D('',#33898,#5596,#5597);
#4740=AXIS2_PLACEMENT_3D('',#33899,#5598,#5599);
#4741=AXIS2_PLACEMENT_3D('',#33900,#5600,#5601);
#4742=AXIS2_PLACEMENT_3D('',#33901,#5602,#5603);
#4743=AXIS2_PLACEMENT_3D('',#33904,#5604,#5605);
#4744=AXIS2_PLACEMENT_3D('',#33905,#5606,#5607);
#4745=AXIS2_PLACEMENT_3D('',#33906,#5608,#5609);
#4746=AXIS2_PLACEMENT_3D('',#33907,#5610,#5611);
#4747=AXIS2_PLACEMENT_3D('',#33910,#5612,#5613);
#4748=AXIS2_PLACEMENT_3D('',#33911,#5614,#5615);
#4749=AXIS2_PLACEMENT_3D('',#33912,#5616,#5617);
#4750=AXIS2_PLACEMENT_3D('',#33913,#5618,#5619);
#4751=AXIS2_PLACEMENT_3D('',#33916,#5620,#5621);
#4752=AXIS2_PLACEMENT_3D('',#33917,#5622,#5623);
#4753=AXIS2_PLACEMENT_3D('',#33918,#5624,#5625);
#4754=AXIS2_PLACEMENT_3D('',#33919,#5626,#5627);
#4755=AXIS2_PLACEMENT_3D('',#33922,#5628,#5629);
#4756=AXIS2_PLACEMENT_3D('',#33923,#5630,#5631);
#4757=AXIS2_PLACEMENT_3D('',#33924,#5632,#5633);
#4758=AXIS2_PLACEMENT_3D('',#33925,#5634,#5635);
#4759=AXIS2_PLACEMENT_3D('',#33927,#5636,#5637);
#4760=AXIS2_PLACEMENT_3D('',#33928,#5638,#5639);
#4761=AXIS2_PLACEMENT_3D('',#33929,#5640,#5641);
#4762=AXIS2_PLACEMENT_3D('',#33930,#5642,#5643);
#4763=AXIS2_PLACEMENT_3D('',#33931,#5644,#5645);
#4764=AXIS2_PLACEMENT_3D('',#33932,#5646,#5647);
#4765=AXIS2_PLACEMENT_3D('',#33936,#5649,#5650);
#4766=AXIS2_PLACEMENT_3D('',#33938,#5652,#5653);
#4767=AXIS2_PLACEMENT_3D('',#33941,#5655,#5656);
#4768=AXIS2_PLACEMENT_3D('',#33942,#5657,#5658);
#4769=AXIS2_PLACEMENT_3D('',#33945,#5660,#5661);
#4770=AXIS2_PLACEMENT_3D('',#33946,#5662,#5663);
#4771=AXIS2_PLACEMENT_3D('',#33949,#5665,#5666);
#4772=AXIS2_PLACEMENT_3D('',#33950,#5667,#5668);
#4773=AXIS2_PLACEMENT_3D('',#33953,#5670,#5671);
#4774=AXIS2_PLACEMENT_3D('',#33954,#5672,#5673);
#4775=AXIS2_PLACEMENT_3D('',#33957,#5675,#5676);
#4776=AXIS2_PLACEMENT_3D('',#33958,#5677,#5678);
#4777=AXIS2_PLACEMENT_3D('',#33961,#5680,#5681);
#4778=AXIS2_PLACEMENT_3D('',#33962,#5682,#5683);
#4779=AXIS2_PLACEMENT_3D('',#33965,#5685,#5686);
#4780=AXIS2_PLACEMENT_3D('',#33966,#5687,#5688);
#4781=AXIS2_PLACEMENT_3D('',#33969,#5690,#5691);
#4782=AXIS2_PLACEMENT_3D('',#33970,#5692,#5693);
#4783=AXIS2_PLACEMENT_3D('',#33973,#5695,#5696);
#4784=AXIS2_PLACEMENT_3D('',#33974,#5697,#5698);
#4785=AXIS2_PLACEMENT_3D('',#33977,#5700,#5701);
#4786=AXIS2_PLACEMENT_3D('',#33978,#5702,#5703);
#4787=AXIS2_PLACEMENT_3D('',#33981,#5705,#5706);
#4788=AXIS2_PLACEMENT_3D('',#33982,#5707,#5708);
#4789=AXIS2_PLACEMENT_3D('',#33985,#5710,#5711);
#4790=AXIS2_PLACEMENT_3D('',#33986,#5712,#5713);
#4791=AXIS2_PLACEMENT_3D('',#33989,#5715,#5716);
#4792=AXIS2_PLACEMENT_3D('',#33990,#5717,#5718);
#4793=AXIS2_PLACEMENT_3D('',#33991,#5719,#5720);
#4794=AXIS2_PLACEMENT_3D('',#33992,#5721,#5722);
#4795=AXIS2_PLACEMENT_3D('',#33994,#5723,#5724);
#4796=AXIS2_PLACEMENT_3D('',#33996,#5725,#5726);
#4797=AXIS2_PLACEMENT_3D('',#33998,#5727,#5728);
#4798=AXIS2_PLACEMENT_3D('',#34000,#5729,#5730);
#4799=AXIS2_PLACEMENT_3D('',#34002,#5731,#5732);
#4800=AXIS2_PLACEMENT_3D('',#34004,#5733,#5734);
#4801=AXIS2_PLACEMENT_3D('',#34006,#5735,#5736);
#4802=AXIS2_PLACEMENT_3D('',#34008,#5737,#5738);
#4803=AXIS2_PLACEMENT_3D('',#34010,#5739,#5740);
#4804=AXIS2_PLACEMENT_3D('',#34011,#5741,#5742);
#4805=AXIS2_PLACEMENT_3D('',#34014,#5743,#5744);
#4806=AXIS2_PLACEMENT_3D('',#34016,#5745,#5746);
#4807=AXIS2_PLACEMENT_3D('',#34018,#5747,#5748);
#4808=AXIS2_PLACEMENT_3D('',#34019,#5749,#5750);
#4809=AXIS2_PLACEMENT_3D('',#34020,#5751,#5752);
#4810=AXIS2_PLACEMENT_3D('',#34022,#5753,#5754);
#4811=AXIS2_PLACEMENT_3D('',#34023,#5755,#5756);
#4812=AXIS2_PLACEMENT_3D('',#34024,#5757,#5758);
#4813=AXIS2_PLACEMENT_3D('',#34025,#5759,#5760);
#4814=AXIS2_PLACEMENT_3D('',#34027,#5761,#5762);
#4815=AXIS2_PLACEMENT_3D('',#34028,#5763,#5764);
#4816=AXIS2_PLACEMENT_3D('',#34029,#5765,#5766);
#4817=AXIS2_PLACEMENT_3D('',#34031,#5767,#5768);
#4818=AXIS2_PLACEMENT_3D('',#34032,#5769,#5770);
#4819=AXIS2_PLACEMENT_3D('',#34033,#5771,#5772);
#4820=AXIS2_PLACEMENT_3D('',#34035,#5773,#5774);
#4821=AXIS2_PLACEMENT_3D('',#34036,#5775,#5776);
#4822=AXIS2_PLACEMENT_3D('',#34037,#5777,#5778);
#4823=AXIS2_PLACEMENT_3D('',#34039,#5779,#5780);
#4824=AXIS2_PLACEMENT_3D('',#34040,#5781,#5782);
#4825=AXIS2_PLACEMENT_3D('',#34041,#5783,#5784);
#4826=AXIS2_PLACEMENT_3D('',#34043,#5785,#5786);
#4827=AXIS2_PLACEMENT_3D('',#34044,#5787,#5788);
#4828=AXIS2_PLACEMENT_3D('',#34045,#5789,#5790);
#4829=AXIS2_PLACEMENT_3D('',#34047,#5791,#5792);
#4830=AXIS2_PLACEMENT_3D('',#34048,#5793,#5794);
#4831=AXIS2_PLACEMENT_3D('',#34049,#5795,#5796);
#4832=AXIS2_PLACEMENT_3D('',#34051,#5797,#5798);
#4833=AXIS2_PLACEMENT_3D('',#34052,#5799,#5800);
#4834=AXIS2_PLACEMENT_3D('',#34053,#5801,#5802);
#4835=AXIS2_PLACEMENT_3D('',#34055,#5803,#5804);
#4836=AXIS2_PLACEMENT_3D('',#34056,#5805,#5806);
#4837=AXIS2_PLACEMENT_3D('',#34057,#5807,#5808);
#4838=AXIS2_PLACEMENT_3D('',#34059,#5809,#5810);
#4839=AXIS2_PLACEMENT_3D('',#34060,#5811,#5812);
#4840=AXIS2_PLACEMENT_3D('',#34061,#5813,#5814);
#4841=AXIS2_PLACEMENT_3D('',#34063,#5815,#5816);
#4842=AXIS2_PLACEMENT_3D('',#34064,#5817,#5818);
#4843=AXIS2_PLACEMENT_3D('',#34065,#5819,#5820);
#4844=AXIS2_PLACEMENT_3D('',#34067,#5821,#5822);
#4845=AXIS2_PLACEMENT_3D('',#34068,#5823,#5824);
#4846=AXIS2_PLACEMENT_3D('',#34069,#5825,#5826);
#4847=AXIS2_PLACEMENT_3D('',#34071,#5827,#5828);
#4848=AXIS2_PLACEMENT_3D('',#34072,#5829,#5830);
#4849=AXIS2_PLACEMENT_3D('',#34073,#5831,#5832);
#4850=AXIS2_PLACEMENT_3D('',#34075,#5833,#5834);
#4851=AXIS2_PLACEMENT_3D('',#34076,#5835,#5836);
#4852=AXIS2_PLACEMENT_3D('',#34077,#5837,#5838);
#4853=AXIS2_PLACEMENT_3D('',#34079,#5839,#5840);
#4854=AXIS2_PLACEMENT_3D('',#34080,#5841,#5842);
#4855=AXIS2_PLACEMENT_3D('',#34081,#5843,#5844);
#4856=AXIS2_PLACEMENT_3D('',#34083,#5845,#5846);
#4857=AXIS2_PLACEMENT_3D('',#34084,#5847,#5848);
#4858=AXIS2_PLACEMENT_3D('',#34085,#5849,#5850);
#4859=AXIS2_PLACEMENT_3D('',#34087,#5851,#5852);
#4860=AXIS2_PLACEMENT_3D('',#34088,#5853,#5854);
#4861=AXIS2_PLACEMENT_3D('',#34089,#5855,#5856);
#4862=AXIS2_PLACEMENT_3D('',#34091,#5857,#5858);
#4863=AXIS2_PLACEMENT_3D('',#34092,#5859,#5860);
#4864=AXIS2_PLACEMENT_3D('',#34093,#5861,#5862);
#4865=AXIS2_PLACEMENT_3D('',#34094,#5863,#5864);
#4866=AXIS2_PLACEMENT_3D('',#34096,#5865,#5866);
#4867=AXIS2_PLACEMENT_3D('',#34097,#5867,#5868);
#4868=AXIS2_PLACEMENT_3D('',#34098,#5869,#5870);
#4869=AXIS2_PLACEMENT_3D('',#34100,#5871,#5872);
#4870=AXIS2_PLACEMENT_3D('',#34101,#5873,#5874);
#4871=AXIS2_PLACEMENT_3D('',#34102,#5875,#5876);
#4872=AXIS2_PLACEMENT_3D('',#34105,#5877,#5878);
#4873=AXIS2_PLACEMENT_3D('',#34106,#5879,#5880);
#4874=AXIS2_PLACEMENT_3D('',#34107,#5881,#5882);
#4875=AXIS2_PLACEMENT_3D('',#34108,#5883,#5884);
#4876=AXIS2_PLACEMENT_3D('',#34111,#5885,#5886);
#4877=AXIS2_PLACEMENT_3D('',#34112,#5887,#5888);
#4878=AXIS2_PLACEMENT_3D('',#34113,#5889,#5890);
#4879=AXIS2_PLACEMENT_3D('',#34114,#5891,#5892);
#4880=AXIS2_PLACEMENT_3D('',#34117,#5893,#5894);
#4881=AXIS2_PLACEMENT_3D('',#34118,#5895,#5896);
#4882=AXIS2_PLACEMENT_3D('',#34119,#5897,#5898);
#4883=AXIS2_PLACEMENT_3D('',#34120,#5899,#5900);
#4884=AXIS2_PLACEMENT_3D('',#34123,#5901,#5902);
#4885=AXIS2_PLACEMENT_3D('',#34124,#5903,#5904);
#4886=AXIS2_PLACEMENT_3D('',#34125,#5905,#5906);
#4887=AXIS2_PLACEMENT_3D('',#34126,#5907,#5908);
#4888=AXIS2_PLACEMENT_3D('',#34129,#5909,#5910);
#4889=AXIS2_PLACEMENT_3D('',#34130,#5911,#5912);
#4890=AXIS2_PLACEMENT_3D('',#34131,#5913,#5914);
#4891=AXIS2_PLACEMENT_3D('',#34132,#5915,#5916);
#4892=AXIS2_PLACEMENT_3D('',#34135,#5917,#5918);
#4893=AXIS2_PLACEMENT_3D('',#34136,#5919,#5920);
#4894=AXIS2_PLACEMENT_3D('',#34137,#5921,#5922);
#4895=AXIS2_PLACEMENT_3D('',#34138,#5923,#5924);
#4896=AXIS2_PLACEMENT_3D('',#34141,#5925,#5926);
#4897=AXIS2_PLACEMENT_3D('',#34142,#5927,#5928);
#4898=AXIS2_PLACEMENT_3D('',#34143,#5929,#5930);
#4899=AXIS2_PLACEMENT_3D('',#34144,#5931,#5932);
#4900=AXIS2_PLACEMENT_3D('',#34147,#5933,#5934);
#4901=AXIS2_PLACEMENT_3D('',#34148,#5935,#5936);
#4902=AXIS2_PLACEMENT_3D('',#34149,#5937,#5938);
#4903=AXIS2_PLACEMENT_3D('',#34150,#5939,#5940);
#4904=AXIS2_PLACEMENT_3D('',#34153,#5941,#5942);
#4905=AXIS2_PLACEMENT_3D('',#34154,#5943,#5944);
#4906=AXIS2_PLACEMENT_3D('',#34155,#5945,#5946);
#4907=AXIS2_PLACEMENT_3D('',#34156,#5947,#5948);
#4908=AXIS2_PLACEMENT_3D('',#34159,#5949,#5950);
#4909=AXIS2_PLACEMENT_3D('',#34160,#5951,#5952);
#4910=AXIS2_PLACEMENT_3D('',#34161,#5953,#5954);
#4911=AXIS2_PLACEMENT_3D('',#34162,#5955,#5956);
#4912=AXIS2_PLACEMENT_3D('',#34163,#5957,#5958);
#4913=AXIS2_PLACEMENT_3D('',#34164,#5959,#5960);
#4914=AXIS2_PLACEMENT_3D('',#34165,#5961,#5962);
#4915=AXIS2_PLACEMENT_3D('',#34167,#5964,#5965);
#4916=AXIS2_PLACEMENT_3D('',#34168,#5966,#5967);
#4917=AXIS2_PLACEMENT_3D('',#34170,#5969,#5970);
#4918=AXIS2_PLACEMENT_3D('',#34172,#5972,#5973);
#4919=AXIS2_PLACEMENT_3D('',#34174,#5975,#5976);
#4920=AXIS2_PLACEMENT_3D('',#34176,#5978,#5979);
#4921=AXIS2_PLACEMENT_3D('',#34178,#5981,#5982);
#4922=AXIS2_PLACEMENT_3D('',#34180,#5984,#5985);
#4923=AXIS2_PLACEMENT_3D('',#34182,#5987,#5988);
#4924=AXIS2_PLACEMENT_3D('',#34184,#5990,#5991);
#4925=AXIS2_PLACEMENT_3D('',#34186,#5993,#5994);
#4926=AXIS2_PLACEMENT_3D('',#34188,#5996,#5997);
#4927=AXIS2_PLACEMENT_3D('',#34190,#5999,#6000);
#4928=AXIS2_PLACEMENT_3D('',#34192,#6002,#6003);
#4929=AXIS2_PLACEMENT_3D('',#34194,#6004,#6005);
#4930=AXIS2_PLACEMENT_3D('',#34196,#6006,#6007);
#4931=AXIS2_PLACEMENT_3D('',#34198,#6008,#6009);
#4932=AXIS2_PLACEMENT_3D('',#34200,#6010,#6011);
#4933=AXIS2_PLACEMENT_3D('',#34202,#6012,#6013);
#4934=AXIS2_PLACEMENT_3D('',#34204,#6014,#6015);
#4935=AXIS2_PLACEMENT_3D('',#34206,#6016,#6017);
#4936=AXIS2_PLACEMENT_3D('',#34208,#6018,#6019);
#4937=AXIS2_PLACEMENT_3D('',#34210,#6020,#6021);
#4938=AXIS2_PLACEMENT_3D('',#34211,#6022,#6023);
#4939=AXIS2_PLACEMENT_3D('',#34213,#6024,#6025);
#4940=AXIS2_PLACEMENT_3D('',#34215,#6026,#6027);
#4941=AXIS2_PLACEMENT_3D('',#34216,#6028,#6029);
#4942=AXIS2_PLACEMENT_3D('',#34217,#6030,#6031);
#4943=AXIS2_PLACEMENT_3D('',#34221,#6033,#6034);
#4944=AXIS2_PLACEMENT_3D('',#34222,#6035,#6036);
#4945=AXIS2_PLACEMENT_3D('',#34223,#6037,#6038);
#4946=AXIS2_PLACEMENT_3D('',#34224,#6039,#6040);
#4947=AXIS2_PLACEMENT_3D('',#34225,#6041,#6042);
#4948=AXIS2_PLACEMENT_3D('',#34226,#6043,#6044);
#4949=AXIS2_PLACEMENT_3D('',#34228,#6046,#6047);
#4950=AXIS2_PLACEMENT_3D('',#34230,#6049,#6050);
#4951=AXIS2_PLACEMENT_3D('',#34232,#6052,#6053);
#4952=AXIS2_PLACEMENT_3D('',#34234,#6055,#6056);
#4953=AXIS2_PLACEMENT_3D('',#34236,#6058,#6059);
#4954=AXIS2_PLACEMENT_3D('',#34238,#6061,#6062);
#4955=AXIS2_PLACEMENT_3D('',#34240,#6064,#6065);
#4956=AXIS2_PLACEMENT_3D('',#34242,#6067,#6068);
#4957=AXIS2_PLACEMENT_3D('',#34243,#6069,#6070);
#4958=AXIS2_PLACEMENT_3D('',#34246,#6071,#6072);
#4959=AXIS2_PLACEMENT_3D('',#34250,#6074,#6075);
#4960=AXIS2_PLACEMENT_3D('',#34256,#6079,#6080);
#4961=AXIS2_PLACEMENT_3D('',#34261,#6082,#6083);
#4962=AXIS2_PLACEMENT_3D('',#34263,#6084,#6085);
#4963=AXIS2_PLACEMENT_3D('',#34285,#6086,#6087);
#4964=AXIS2_PLACEMENT_3D('',#34286,#6088,#6089);
#4965=AXIS2_PLACEMENT_3D('',#34287,#6090,#6091);
#4966=AXIS2_PLACEMENT_3D('',#34311,#6094,#6095);
#4967=AXIS2_PLACEMENT_3D('',#34313,#6096,#6097);
#4968=AXIS2_PLACEMENT_3D('',#34314,#6098,#6099);
#4969=AXIS2_PLACEMENT_3D('',#34316,#6100,#6101);
#4970=AXIS2_PLACEMENT_3D('',#34317,#6102,#6103);
#4971=AXIS2_PLACEMENT_3D('',#34318,#6104,#6105);
#4972=AXIS2_PLACEMENT_3D('',#34320,#6107,#6108);
#4973=AXIS2_PLACEMENT_3D('',#34322,#6110,#6111);
#4974=AXIS2_PLACEMENT_3D('',#34328,#6115,#6116);
#4975=AXIS2_PLACEMENT_3D('',#34331,#6118,#6119);
#4976=AXIS2_PLACEMENT_3D('',#34332,#6120,#6121);
#4977=AXIS2_PLACEMENT_3D('',#34336,#6124,#6125);
#4978=AXIS2_PLACEMENT_3D('',#34340,#6128,#6129);
#4979=AXIS2_PLACEMENT_3D('',#34341,#6130,#6131);
#4980=AXIS2_PLACEMENT_3D('',#34342,#6132,#6133);
#4981=AXIS2_PLACEMENT_3D('',#34346,#6136,#6137);
#4982=AXIS2_PLACEMENT_3D('',#34347,#6138,#6139);
#4983=AXIS2_PLACEMENT_3D('',#34348,#6140,#6141);
#4984=AXIS2_PLACEMENT_3D('',#34349,#6142,#6143);
#4985=AXIS2_PLACEMENT_3D('',#34350,#6144,#6145);
#4986=AXIS2_PLACEMENT_3D('',#34359,#6150,#6151);
#4987=AXIS2_PLACEMENT_3D('',#34361,#6152,#6153);
#4988=AXIS2_PLACEMENT_3D('',#34363,#6154,#6155);
#4989=AXIS2_PLACEMENT_3D('',#34365,#6157,#6158);
#4990=AXIS2_PLACEMENT_3D('',#34371,#6162,#6163);
#4991=AXIS2_PLACEMENT_3D('',#34372,#6164,#6165);
#4992=AXIS2_PLACEMENT_3D('',#34373,#6166,#6167);
#4993=AXIS2_PLACEMENT_3D('',#34374,#6168,#6169);
#4994=AXIS2_PLACEMENT_3D('',#34375,#6170,#6171);
#4995=AXIS2_PLACEMENT_3D('',#34376,#6172,#6173);
#4996=AXIS2_PLACEMENT_3D('',#34377,#6174,#6175);
#4997=AXIS2_PLACEMENT_3D('',#34378,#6176,#6177);
#4998=AXIS2_PLACEMENT_3D('',#34379,#6178,#6179);
#4999=AXIS2_PLACEMENT_3D('',#34380,#6180,#6181);
#5000=AXIS2_PLACEMENT_3D('',#34381,#6182,#6183);
#5001=AXIS2_PLACEMENT_3D('',#34382,#6184,#6185);
#5002=AXIS2_PLACEMENT_3D('',#34383,#6186,#6187);
#5003=DIRECTION('axis',(0.,0.,1.));
#5004=DIRECTION('refdir',(1.,0.,0.));
#5005=DIRECTION('axis',(0.,0.,1.));
#5006=DIRECTION('refdir',(1.,0.,0.));
#5007=DIRECTION('center_axis',(0.,0.,1.));
#5008=DIRECTION('ref_axis',(1.,0.,0.));
#5009=DIRECTION('',(0.,0.,1.));
#5010=DIRECTION('center_axis',(0.,0.,1.));
#5011=DIRECTION('ref_axis',(1.,0.,0.));
#5012=DIRECTION('',(0.,0.,1.));
#5013=DIRECTION('center_axis',(0.,-1.,0.));
#5014=DIRECTION('ref_axis',(0.,0.,-1.));
#5015=DIRECTION('center_axis',(0.,1.,0.));
#5016=DIRECTION('ref_axis',(1.,0.,0.));
#5017=DIRECTION('center_axis',(-1.,0.,-1.22464679914735E-16));
#5018=DIRECTION('ref_axis',(-1.22464679914735E-16,0.,1.));
#5019=DIRECTION('center_axis',(0.,-1.,0.));
#5020=DIRECTION('ref_axis',(1.,0.,0.));
#5021=DIRECTION('center_axis',(0.,-1.,0.));
#5022=DIRECTION('ref_axis',(1.,0.,0.));
#5023=DIRECTION('center_axis',(0.,1.,0.));
#5024=DIRECTION('ref_axis',(1.,0.,0.));
#5025=DIRECTION('center_axis',(0.,-1.,0.));
#5026=DIRECTION('ref_axis',(1.,0.,0.));
#5027=DIRECTION('center_axis',(0.,1.,0.));
#5028=DIRECTION('ref_axis',(1.,0.,0.));
#5029=DIRECTION('center_axis',(0.,1.,0.));
#5030=DIRECTION('ref_axis',(1.,0.,0.));
#5031=DIRECTION('center_axis',(0.,1.,0.));
#5032=DIRECTION('ref_axis',(1.,0.,0.));
#5033=DIRECTION('',(0.,1.,0.));
#5034=DIRECTION('center_axis',(0.,1.,0.));
#5035=DIRECTION('ref_axis',(0.,0.,1.));
#5036=DIRECTION('center_axis',(-1.,0.,1.22464679914735E-16));
#5037=DIRECTION('ref_axis',(-1.22464679914735E-16,0.,-1.));
#5038=DIRECTION('center_axis',(0.,1.,0.));
#5039=DIRECTION('ref_axis',(1.,0.,0.));
#5040=DIRECTION('center_axis',(0.,1.,0.));
#5041=DIRECTION('ref_axis',(1.,0.,0.));
#5042=DIRECTION('center_axis',(0.,1.,0.));
#5043=DIRECTION('ref_axis',(1.,0.,0.));
#5044=DIRECTION('',(0.,-1.,0.));
#5045=DIRECTION('center_axis',(0.,-1.,0.));
#5046=DIRECTION('ref_axis',(1.,0.,0.));
#5047=DIRECTION('center_axis',(0.,-1.,0.));
#5048=DIRECTION('ref_axis',(1.,0.,0.));
#5049=DIRECTION('center_axis',(0.,-1.,0.));
#5050=DIRECTION('ref_axis',(0.,0.,-1.));
#5051=DIRECTION('center_axis',(0.,1.,0.));
#5052=DIRECTION('ref_axis',(1.,0.,0.));
#5053=DIRECTION('center_axis',(-1.,0.,-1.22464679914735E-16));
#5054=DIRECTION('ref_axis',(-1.22464679914735E-16,0.,1.));
#5055=DIRECTION('center_axis',(0.,1.,0.));
#5056=DIRECTION('ref_axis',(1.,0.,0.));
#5057=DIRECTION('center_axis',(0.,-1.,0.));
#5058=DIRECTION('ref_axis',(1.,0.,0.));
#5059=DIRECTION('center_axis',(0.,1.,0.));
#5060=DIRECTION('ref_axis',(0.,0.,1.));
#5061=DIRECTION('center_axis',(-1.,0.,1.22464679914735E-16));
#5062=DIRECTION('ref_axis',(-1.22464679914735E-16,0.,-1.));
#5063=DIRECTION('axis',(0.,0.,1.));
#5064=DIRECTION('refdir',(1.,0.,0.));
#5065=DIRECTION('center_axis',(1.,2.22044604925031E-16,0.));
#5066=DIRECTION('ref_axis',(-2.22044604925031E-16,1.,0.));
#5067=DIRECTION('center_axis',(1.,2.22044604925031E-16,0.));
#5068=DIRECTION('ref_axis',(-2.22044604925031E-16,1.,0.));
#5069=DIRECTION('',(-1.,-2.22044604925031E-16,0.));
#5070=DIRECTION('center_axis',(-1.,-2.22044604925031E-16,0.));
#5071=DIRECTION('ref_axis',(-2.22044604925031E-16,1.,0.));
#5072=DIRECTION('center_axis',(-1.,-2.22044604925031E-16,0.));
#5073=DIRECTION('ref_axis',(-2.22044604925031E-16,1.,0.));
#5074=DIRECTION('center_axis',(-1.,-2.22044604925031E-16,0.));
#5075=DIRECTION('ref_axis',(-2.22044604925031E-16,1.,0.));
#5076=DIRECTION('axis',(0.,0.,1.));
#5077=DIRECTION('refdir',(1.,0.,0.));
#5078=DIRECTION('center_axis',(0.,0.,1.));
#5079=DIRECTION('ref_axis',(-1.,0.,0.));
#5080=DIRECTION('center_axis',(0.,0.,-1.));
#5081=DIRECTION('ref_axis',(-1.,0.,0.));
#5082=DIRECTION('',(0.,0.,1.));
#5083=DIRECTION('center_axis',(0.,0.,-1.));
#5084=DIRECTION('ref_axis',(-1.,0.,0.));
#5085=DIRECTION('center_axis',(0.,0.,1.));
#5086=DIRECTION('ref_axis',(-1.,0.,0.));
#5087=DIRECTION('center_axis',(0.,0.,-1.));
#5088=DIRECTION('ref_axis',(-1.,0.,0.));
#5089=DIRECTION('',(0.,0.,-1.));
#5090=DIRECTION('center_axis',(0.,0.,-1.));
#5091=DIRECTION('ref_axis',(-1.,0.,0.));
#5092=DIRECTION('center_axis',(0.,0.,1.));
#5093=DIRECTION('ref_axis',(-1.,0.,0.));
#5094=DIRECTION('center_axis',(0.,0.,1.));
#5095=DIRECTION('ref_axis',(-1.,0.,0.));
#5096=DIRECTION('axis',(0.,0.,1.));
#5097=DIRECTION('refdir',(1.,0.,0.));
#5098=DIRECTION('center_axis',(0.,0.,1.));
#5099=DIRECTION('ref_axis',(0.566311127537338,0.824191547413215,0.));
#5100=DIRECTION('',(0.,0.,1.));
#5101=DIRECTION('center_axis',(0.,0.,-1.));
#5102=DIRECTION('ref_axis',(1.,3.22059269378563E-14,0.));
#5103=DIRECTION('center_axis',(0.,0.,1.));
#5104=DIRECTION('ref_axis',(0.566311127537338,0.824191547413215,0.));
#5105=DIRECTION('',(0.,0.,1.));
#5106=DIRECTION('center_axis',(0.,0.,1.));
#5107=DIRECTION('ref_axis',(0.566311127537338,0.824191547413215,0.));
#5108=DIRECTION('',(0.,0.,1.));
#5109=DIRECTION('center_axis',(0.,0.,1.));
#5110=DIRECTION('ref_axis',(0.566311127537338,0.824191547413215,0.));
#5111=DIRECTION('',(0.,0.,1.));
#5112=DIRECTION('center_axis',(0.,0.,1.));
#5113=DIRECTION('ref_axis',(0.566311127537338,0.824191547413215,0.));
#5114=DIRECTION('',(0.,0.,1.));
#5115=DIRECTION('center_axis',(0.,0.,1.));
#5116=DIRECTION('ref_axis',(0.566311127537338,0.824191547413215,0.));
#5117=DIRECTION('',(0.,0.,1.));
#5118=DIRECTION('center_axis',(0.,0.,1.));
#5119=DIRECTION('ref_axis',(0.566311127537338,0.824191547413215,0.));
#5120=DIRECTION('',(0.,0.,1.));
#5121=DIRECTION('center_axis',(0.,0.,1.));
#5122=DIRECTION('ref_axis',(0.566311127537338,0.824191547413215,0.));
#5123=DIRECTION('',(0.,0.,1.));
#5124=DIRECTION('center_axis',(0.,0.,1.));
#5125=DIRECTION('ref_axis',(1.,3.22059269378563E-14,0.));
#5126=DIRECTION('center_axis',(0.,0.,1.));
#5127=DIRECTION('ref_axis',(0.999190683258091,-0.0402241033489821,0.));
#5128=DIRECTION('',(0.,0.,1.));
#5129=DIRECTION('center_axis',(0.,0.,1.));
#5130=DIRECTION('ref_axis',(1.,0.,0.));
#5131=DIRECTION('center_axis',(0.,0.,1.));
#5132=DIRECTION('ref_axis',(0.999190683258091,-0.0402241033489821,0.));
#5133=DIRECTION('',(0.,0.,1.));
#5134=DIRECTION('center_axis',(0.,0.,1.));
#5135=DIRECTION('ref_axis',(0.999190683258091,-0.0402241033489821,0.));
#5136=DIRECTION('',(0.,0.,1.));
#5137=DIRECTION('center_axis',(0.,0.,1.));
#5138=DIRECTION('ref_axis',(0.999190683258091,-0.0402241033489821,0.));
#5139=DIRECTION('',(0.,0.,1.));
#5140=DIRECTION('center_axis',(0.,0.,1.));
#5141=DIRECTION('ref_axis',(0.999190683258091,-0.0402241033489821,0.));
#5142=DIRECTION('',(0.,0.,1.));
#5143=DIRECTION('center_axis',(0.,0.,1.));
#5144=DIRECTION('ref_axis',(0.999190683258091,-0.0402241033489821,0.));
#5145=DIRECTION('',(0.,0.,1.));
#5146=DIRECTION('center_axis',(0.,0.,1.));
#5147=DIRECTION('ref_axis',(0.999190683258091,-0.0402241033489821,0.));
#5148=DIRECTION('',(0.,0.,1.));
#5149=DIRECTION('center_axis',(0.,0.,1.));
#5150=DIRECTION('ref_axis',(0.999190683258091,-0.0402241033489821,0.));
#5151=DIRECTION('center_axis',(0.,0.,1.));
#5152=DIRECTION('ref_axis',(1.,0.,0.));
#5153=DIRECTION('',(0.,0.,1.));
#5154=DIRECTION('center_axis',(0.,0.,1.));
#5155=DIRECTION('ref_axis',(1.,0.,0.));
#5156=DIRECTION('',(0.,0.,1.));
#5157=DIRECTION('center_axis',(0.,0.,1.));
#5158=DIRECTION('ref_axis',(1.,0.,0.));
#5159=DIRECTION('center_axis',(0.,0.,1.));
#5160=DIRECTION('ref_axis',(0.999190683258091,-0.0402241033489821,0.));
#5161=DIRECTION('center_axis',(0.,0.,1.));
#5162=DIRECTION('ref_axis',(0.566311127537338,0.824191547413215,0.));
#5163=DIRECTION('center_axis',(0.,0.,1.));
#5164=DIRECTION('ref_axis',(1.,0.,0.));
#5165=DIRECTION('center_axis',(0.,0.,-1.));
#5166=DIRECTION('ref_axis',(-1.,0.,0.));
#5167=DIRECTION('center_axis',(0.,0.,-1.));
#5168=DIRECTION('ref_axis',(-1.,0.,0.));
#5169=DIRECTION('',(0.,0.,1.));
#5170=DIRECTION('center_axis',(0.,0.,1.));
#5171=DIRECTION('ref_axis',(-1.,0.,0.));
#5172=DIRECTION('center_axis',(0.,0.,1.));
#5173=DIRECTION('ref_axis',(-1.,0.,0.));
#5174=DIRECTION('center_axis',(0.,0.,-1.));
#5175=DIRECTION('ref_axis',(1.,0.,0.));
#5176=DIRECTION('center_axis',(0.,0.,1.));
#5177=DIRECTION('ref_axis',(1.,0.,0.));
#5178=DIRECTION('center_axis',(0.,0.,1.));
#5179=DIRECTION('ref_axis',(1.,0.,0.));
#5180=DIRECTION('center_axis',(0.,0.,1.));
#5181=DIRECTION('ref_axis',(1.,0.,0.));
#5182=DIRECTION('',(0.,0.,-1.));
#5183=DIRECTION('center_axis',(0.,0.,1.));
#5184=DIRECTION('ref_axis',(1.,0.,0.));
#5185=DIRECTION('axis',(0.,0.,1.));
#5186=DIRECTION('refdir',(1.,0.,0.));
#5187=DIRECTION('center_axis',(0.,0.,1.));
#5188=DIRECTION('ref_axis',(-0.70398889171803,0.71021098297451,0.));
#5189=DIRECTION('',(0.,0.,-1.));
#5190=DIRECTION('center_axis',(0.,0.,-1.));
#5191=DIRECTION('ref_axis',(-1.,-4.63459159752748E-15,0.));
#5192=DIRECTION('center_axis',(0.,0.,1.));
#5193=DIRECTION('ref_axis',(-0.70398889171803,0.71021098297451,0.));
#5194=DIRECTION('',(0.,0.,-1.));
#5195=DIRECTION('center_axis',(0.,0.,1.));
#5196=DIRECTION('ref_axis',(-0.70398889171803,0.71021098297451,0.));
#5197=DIRECTION('',(0.,0.,-1.));
#5198=DIRECTION('center_axis',(0.,0.,1.));
#5199=DIRECTION('ref_axis',(-0.70398889171803,0.71021098297451,0.));
#5200=DIRECTION('',(0.,0.,-1.));
#5201=DIRECTION('center_axis',(0.,0.,1.));
#5202=DIRECTION('ref_axis',(-0.70398889171803,0.71021098297451,0.));
#5203=DIRECTION('',(0.,0.,-1.));
#5204=DIRECTION('center_axis',(0.,0.,1.));
#5205=DIRECTION('ref_axis',(-0.70398889171803,0.71021098297451,0.));
#5206=DIRECTION('',(0.,0.,-1.));
#5207=DIRECTION('center_axis',(0.,0.,1.));
#5208=DIRECTION('ref_axis',(-1.,0.,0.));
#5209=DIRECTION('center_axis',(0.,0.,1.));
#5210=DIRECTION('ref_axis',(-1.,0.,0.));
#5211=DIRECTION('center_axis',(0.,0.,1.));
#5212=DIRECTION('ref_axis',(-1.,0.,0.));
#5213=DIRECTION('center_axis',(0.,0.,1.));
#5214=DIRECTION('ref_axis',(-0.70398889171803,0.71021098297451,0.));
#5215=DIRECTION('center_axis',(0.,0.,1.));
#5216=DIRECTION('ref_axis',(-1.,-4.63459159752748E-15,0.));
#5217=DIRECTION('',(-2.22044604925031E-16,1.,0.));
#5218=DIRECTION('center_axis',(-1.,-2.22044604925031E-16,0.));
#5219=DIRECTION('ref_axis',(-2.22044604925031E-16,1.,0.));
#5220=DIRECTION('',(0.,0.,1.));
#5221=DIRECTION('center_axis',(-1.,-2.22044604925031E-16,0.));
#5222=DIRECTION('ref_axis',(-2.22044604925031E-16,1.,0.));
#5223=DIRECTION('',(0.,0.,-1.));
#5224=DIRECTION('center_axis',(0.,0.,1.));
#5225=DIRECTION('ref_axis',(-1.,0.,0.));
#5226=DIRECTION('',(0.,0.,-1.));
#5227=DIRECTION('',(0.,0.,1.));
#5228=DIRECTION('',(0.,0.,-1.));
#5229=DIRECTION('center_axis',(0.,0.,1.));
#5230=DIRECTION('ref_axis',(-1.,0.,0.));
#5231=DIRECTION('',(2.22044604925031E-16,-1.,0.));
#5232=DIRECTION('center_axis',(-1.,-2.22044604925031E-16,0.));
#5233=DIRECTION('ref_axis',(-2.22044604925031E-16,1.,0.));
#5234=DIRECTION('center_axis',(1.,2.22044604925031E-16,0.));
#5235=DIRECTION('ref_axis',(-2.22044604925031E-16,1.,0.));
#5236=DIRECTION('center_axis',(1.,2.22044604925031E-16,0.));
#5237=DIRECTION('ref_axis',(-2.22044604925031E-16,1.,0.));
#5238=DIRECTION('center_axis',(0.,0.,-1.));
#5239=DIRECTION('ref_axis',(-1.,0.,0.));
#5240=DIRECTION('center_axis',(0.,0.,-1.));
#5241=DIRECTION('ref_axis',(-1.,0.,0.));
#5242=DIRECTION('axis',(0.,0.,1.));
#5243=DIRECTION('refdir',(1.,0.,0.));
#5244=DIRECTION('center_axis',(1.22464679914735E-16,0.,-1.));
#5245=DIRECTION('ref_axis',(0.152224682118134,0.988345914219325,1.86421469707196E-17));
#5246=DIRECTION('',(-1.22464679914735E-16,0.,1.));
#5247=DIRECTION('center_axis',(1.22464679914735E-16,0.,-1.));
#5248=DIRECTION('ref_axis',(1.,-4.63459159752748E-15,1.22464679914735E-16));
#5249=DIRECTION('center_axis',(1.22464679914735E-16,0.,-1.));
#5250=DIRECTION('ref_axis',(0.152224682118134,0.988345914219325,1.86421469707196E-17));
#5251=DIRECTION('',(-1.22464679914735E-16,0.,1.));
#5252=DIRECTION('center_axis',(1.22464679914735E-16,0.,-1.));
#5253=DIRECTION('ref_axis',(0.152224682118134,0.988345914219325,1.86421469707196E-17));
#5254=DIRECTION('',(-1.22464679914735E-16,0.,1.));
#5255=DIRECTION('center_axis',(1.22464679914735E-16,0.,-1.));
#5256=DIRECTION('ref_axis',(0.152224682118134,0.988345914219325,1.86421469707196E-17));
#5257=DIRECTION('',(-1.22464679914735E-16,0.,1.));
#5258=DIRECTION('center_axis',(1.22464679914735E-16,0.,-1.));
#5259=DIRECTION('ref_axis',(0.152224682118134,0.988345914219325,1.86421469707196E-17));
#5260=DIRECTION('',(-1.22464679914735E-16,0.,1.));
#5261=DIRECTION('center_axis',(1.22464679914735E-16,0.,-1.));
#5262=DIRECTION('ref_axis',(0.152224682118134,0.988345914219325,1.86421469707196E-17));
#5263=DIRECTION('',(-1.22464679914735E-16,0.,1.));
#5264=DIRECTION('center_axis',(1.22464679914735E-16,0.,-1.));
#5265=DIRECTION('ref_axis',(0.152224682118134,0.988345914219325,1.86421469707196E-17));
#5266=DIRECTION('',(-1.22464679914735E-16,0.,1.));
#5267=DIRECTION('center_axis',(1.22464679914735E-16,0.,-1.));
#5268=DIRECTION('ref_axis',(0.152224682118134,0.988345914219325,1.86421469707196E-17));
#5269=DIRECTION('',(-1.22464679914735E-16,0.,1.));
#5270=DIRECTION('center_axis',(1.22464679914735E-16,0.,-1.));
#5271=DIRECTION('ref_axis',(1.,0.,1.22464679914735E-16));
#5272=DIRECTION('center_axis',(-1.22464679914735E-16,0.,1.));
#5273=DIRECTION('ref_axis',(1.,0.,1.22464679914735E-16));
#5274=DIRECTION('center_axis',(0.00374951423302316,-0.05043654781332,-0.998720228986923));
#5275=DIRECTION('ref_axis',(-0.999992969847666,-0.000226459877875131,-0.00374285601754598));
#5276=DIRECTION('center_axis',(-1.22464679914735E-16,0.,1.));
#5277=DIRECTION('ref_axis',(1.,0.,1.22464679914735E-16));
#5278=DIRECTION('center_axis',(1.22464679914735E-16,0.,-1.));
#5279=DIRECTION('ref_axis',(-0.533717072258489,0.845663104776262,-6.53614904191654E-17));
#5280=DIRECTION('center_axis',(1.22464679914735E-16,0.,-1.));
#5281=DIRECTION('ref_axis',(1.,-4.63459159752748E-15,1.22464679914735E-16));
#5282=DIRECTION('',(-2.22044604925031E-16,1.,-2.71926214689378E-32));
#5283=DIRECTION('center_axis',(-1.,-2.22044604925031E-16,0.));
#5284=DIRECTION('ref_axis',(-2.22044604925031E-16,1.,0.));
#5285=DIRECTION('',(1.22464679914735E-16,0.,-1.));
#5286=DIRECTION('center_axis',(1.,2.22044604925031E-16,0.));
#5287=DIRECTION('ref_axis',(-2.22044604925031E-16,1.,0.));
#5288=DIRECTION('',(-1.22464679914735E-16,0.,1.));
#5289=DIRECTION('center_axis',(1.22464679914735E-16,0.,-1.));
#5290=DIRECTION('ref_axis',(1.,0.,1.22464679914735E-16));
#5291=DIRECTION('',(-1.22464679914735E-16,0.,1.));
#5292=DIRECTION('',(1.22464679914735E-16,0.,-1.));
#5293=DIRECTION('',(-1.22464679914735E-16,0.,1.));
#5294=DIRECTION('center_axis',(-1.22464679914735E-16,0.,1.));
#5295=DIRECTION('ref_axis',(1.,0.,1.22464679914735E-16));
#5296=DIRECTION('',(2.22044604925031E-16,-1.,2.71926214689378E-32));
#5297=DIRECTION('center_axis',(1.,2.22044604925031E-16,0.));
#5298=DIRECTION('ref_axis',(-2.22044604925031E-16,1.,0.));
#5299=DIRECTION('center_axis',(-1.,-2.22044604925031E-16,0.));
#5300=DIRECTION('ref_axis',(-2.22044604925031E-16,1.,0.));
#5301=DIRECTION('center_axis',(-1.,-2.22044604925031E-16,0.));
#5302=DIRECTION('ref_axis',(-2.22044604925031E-16,1.,0.));
#5303=DIRECTION('center_axis',(-1.22464679914735E-16,0.,1.));
#5304=DIRECTION('ref_axis',(1.,0.,1.22464679914735E-16));
#5305=DIRECTION('center_axis',(-1.22464679914735E-16,0.,1.));
#5306=DIRECTION('ref_axis',(1.,0.,1.22464679914735E-16));
#5307=DIRECTION('axis',(0.,0.,1.));
#5308=DIRECTION('refdir',(1.,0.,0.));
#5309=DIRECTION('center_axis',(0.,0.,-1.));
#5310=DIRECTION('ref_axis',(-0.608826750567588,-0.793303213023439,0.));
#5311=DIRECTION('',(0.,0.,-1.));
#5312=DIRECTION('center_axis',(0.,0.,1.));
#5313=DIRECTION('ref_axis',(1.,-1.81309624337467E-14,0.));
#5314=DIRECTION('center_axis',(0.,0.,-1.));
#5315=DIRECTION('ref_axis',(-0.608826750567588,-0.793303213023439,0.));
#5316=DIRECTION('',(0.,0.,-1.));
#5317=DIRECTION('center_axis',(0.,0.,-1.));
#5318=DIRECTION('ref_axis',(-0.608826750567588,-0.793303213023439,0.));
#5319=DIRECTION('',(0.,0.,-1.));
#5320=DIRECTION('center_axis',(0.,0.,-1.));
#5321=DIRECTION('ref_axis',(-0.608826750567588,-0.793303213023439,0.));
#5322=DIRECTION('',(0.,0.,-1.));
#5323=DIRECTION('center_axis',(0.,0.,-1.));
#5324=DIRECTION('ref_axis',(-0.608826750567588,-0.793303213023439,0.));
#5325=DIRECTION('',(0.,0.,-1.));
#5326=DIRECTION('center_axis',(0.,0.,-1.));
#5327=DIRECTION('ref_axis',(-0.608826750567588,-0.793303213023439,0.));
#5328=DIRECTION('',(0.,0.,-1.));
#5329=DIRECTION('center_axis',(0.,0.,-1.));
#5330=DIRECTION('ref_axis',(-0.608826750567588,-0.793303213023439,0.));
#5331=DIRECTION('',(0.,0.,-1.));
#5332=DIRECTION('center_axis',(0.,0.,-1.));
#5333=DIRECTION('ref_axis',(-0.608826750567588,-0.793303213023439,0.));
#5334=DIRECTION('',(0.,0.,-1.));
#5335=DIRECTION('center_axis',(0.,0.,-1.));
#5336=DIRECTION('ref_axis',(-0.608826750567588,-0.793303213023439,0.));
#5337=DIRECTION('',(0.,0.,-1.));
#5338=DIRECTION('center_axis',(0.,0.,-1.));
#5339=DIRECTION('ref_axis',(1.,-1.81309624337467E-14,0.));
#5340=DIRECTION('center_axis',(0.,0.,-1.));
#5341=DIRECTION('ref_axis',(1.,0.,0.));
#5342=DIRECTION('center_axis',(0.,0.,1.));
#5343=DIRECTION('ref_axis',(1.,0.,0.));
#5344=DIRECTION('center_axis',(0.,0.,1.));
#5345=DIRECTION('ref_axis',(1.,0.,0.));
#5346=DIRECTION('center_axis',(0.,0.,-1.));
#5347=DIRECTION('ref_axis',(-0.608826750567588,-0.793303213023439,0.));
#5348=DIRECTION('center_axis',(0.,0.,1.));
#5349=DIRECTION('ref_axis',(1.,0.,0.));
#5350=DIRECTION('center_axis',(0.,0.,-1.));
#5351=DIRECTION('ref_axis',(1.,0.,0.));
#5352=DIRECTION('center_axis',(0.,0.,-1.));
#5353=DIRECTION('ref_axis',(1.,0.,0.));
#5354=DIRECTION('center_axis',(0.,0.,-1.));
#5355=DIRECTION('ref_axis',(1.,0.,0.));
#5356=DIRECTION('center_axis',(0.,0.,-1.));
#5357=DIRECTION('ref_axis',(1.,0.,0.));
#5358=DIRECTION('',(0.,0.,1.));
#5359=DIRECTION('center_axis',(0.,0.,1.));
#5360=DIRECTION('ref_axis',(1.,0.,0.));
#5361=DIRECTION('center_axis',(0.,0.,1.));
#5362=DIRECTION('ref_axis',(1.,0.,0.));
#5363=DIRECTION('center_axis',(0.,0.,1.));
#5364=DIRECTION('ref_axis',(-1.,1.22464679914735E-16,0.));
#5365=DIRECTION('center_axis',(0.,0.,1.));
#5366=DIRECTION('ref_axis',(1.,0.,0.));
#5367=DIRECTION('',(0.,0.,1.));
#5368=DIRECTION('center_axis',(0.,-1.,0.));
#5369=DIRECTION('ref_axis',(-0.523000124799862,0.,-0.852332604949106));
#5370=DIRECTION('',(0.,1.,0.));
#5371=DIRECTION('center_axis',(0.,-1.,0.));
#5372=DIRECTION('ref_axis',(-0.523000124799863,0.,-0.852332604949106));
#5373=DIRECTION('',(0.,-1.,0.));
#5374=DIRECTION('center_axis',(0.,1.,0.));
#5375=DIRECTION('ref_axis',(-0.523000124799863,0.,-0.852332604949106));
#5376=DIRECTION('',(0.,1.,0.));
#5377=DIRECTION('center_axis',(0.,-1.,0.));
#5378=DIRECTION('ref_axis',(1.,0.,0.));
#5379=DIRECTION('',(0.,-1.,0.));
#5380=DIRECTION('center_axis',(0.,1.,0.));
#5381=DIRECTION('ref_axis',(6.12323399573677E-17,0.,1.));
#5382=DIRECTION('center_axis',(0.,1.,0.));
#5383=DIRECTION('ref_axis',(-0.523000124799863,0.,0.852332604949106));
#5384=DIRECTION('',(0.,-1.,0.));
#5385=DIRECTION('center_axis',(0.,1.,0.));
#5386=DIRECTION('ref_axis',(-0.523000124799863,0.,0.852332604949105));
#5387=DIRECTION('',(0.,1.,0.));
#5388=DIRECTION('center_axis',(0.,-1.,0.));
#5389=DIRECTION('ref_axis',(-0.523000124799863,0.,0.852332604949105));
#5390=DIRECTION('',(0.,-1.,0.));
#5391=DIRECTION('center_axis',(0.,-1.,0.));
#5392=DIRECTION('ref_axis',(1.,0.,0.));
#5393=DIRECTION('',(0.,1.,0.));
#5394=DIRECTION('center_axis',(0.,-1.,0.));
#5395=DIRECTION('ref_axis',(-1.60812264967664E-16,0.,-1.));
#5396=DIRECTION('center_axis',(0.,1.,0.));
#5397=DIRECTION('ref_axis',(-0.523000124799863,0.,-0.852332604949105));
#5398=DIRECTION('center_axis',(-0.996128362168068,0.,-0.0879106710494425));
#5399=DIRECTION('ref_axis',(-0.0879106710494425,0.,0.996128362168068));
#5400=DIRECTION('center_axis',(0.,1.,0.));
#5401=DIRECTION('ref_axis',(-0.523000124799863,0.,-0.852332604949106));
#5402=DIRECTION('center_axis',(0.372812222548027,0.,-0.927906809285717));
#5403=DIRECTION('ref_axis',(0.,1.,0.));
#5404=DIRECTION('center_axis',(0.,1.,0.));
#5405=DIRECTION('ref_axis',(0.,0.,1.));
#5406=DIRECTION('center_axis',(-0.392511146482165,0.,0.919747247828041));
#5407=DIRECTION('ref_axis',(0.,1.,0.));
#5408=DIRECTION('center_axis',(0.,1.,0.));
#5409=DIRECTION('ref_axis',(-0.382683432365091,0.,0.923879532511286));
#5410=DIRECTION('center_axis',(0.,-1.,0.));
#5411=DIRECTION('ref_axis',(-0.382683432365091,0.,0.923879532511286));
#5412=DIRECTION('center_axis',(0.,1.,0.));
#5413=DIRECTION('ref_axis',(0.,0.,1.));
#5414=DIRECTION('center_axis',(0.766531351459009,0.,0.642206888183571));
#5415=DIRECTION('ref_axis',(0.,1.,0.));
#5416=DIRECTION('center_axis',(0.,-1.,0.));
#5417=DIRECTION('ref_axis',(0.972507099593301,0.,-0.232873229978514));
#5418=DIRECTION('center_axis',(0.,1.,0.));
#5419=DIRECTION('ref_axis',(0.972507099593301,0.,-0.232873229978514));
#5420=DIRECTION('center_axis',(0.,1.,0.));
#5421=DIRECTION('ref_axis',(0.,0.,1.));
#5422=DIRECTION('center_axis',(0.642206888183567,0.,0.766531351459012));
#5423=DIRECTION('ref_axis',(0.,1.,0.));
#5424=DIRECTION('center_axis',(0.,1.,0.));
#5425=DIRECTION('ref_axis',(-0.707106781186547,0.,0.707106781186548));
#5426=DIRECTION('center_axis',(0.,-1.,0.));
#5427=DIRECTION('ref_axis',(-0.707106781186547,0.,0.707106781186548));
#5428=DIRECTION('center_axis',(0.,1.,0.));
#5429=DIRECTION('ref_axis',(0.232873229978514,0.,-0.972507099593301));
#5430=DIRECTION('center_axis',(0.919747247828041,0.,-0.392511146482166));
#5431=DIRECTION('ref_axis',(0.,1.,0.));
#5432=DIRECTION('center_axis',(0.,-1.,0.));
#5433=DIRECTION('ref_axis',(0.232873229978513,0.,-0.972507099593301));
#5434=DIRECTION('center_axis',(0.,1.,0.));
#5435=DIRECTION('ref_axis',(0.232873229978513,0.,-0.972507099593301));
#5436=DIRECTION('center_axis',(0.,1.,0.));
#5437=DIRECTION('ref_axis',(0.,0.,1.));
#5438=DIRECTION('center_axis',(-0.927906809285719,0.,0.372812222548022));
#5439=DIRECTION('ref_axis',(0.,1.,0.));
#5440=DIRECTION('center_axis',(0.,1.,0.));
#5441=DIRECTION('ref_axis',(-0.923879532511287,0.,0.382683432365089));
#5442=DIRECTION('center_axis',(0.,-1.,0.));
#5443=DIRECTION('ref_axis',(-0.923879532511287,0.,0.382683432365089));
#5444=DIRECTION('center_axis',(0.,1.,0.));
#5445=DIRECTION('ref_axis',(0.,0.,1.));
#5446=DIRECTION('center_axis',(0.087910671049441,0.,0.996128362168068));
#5447=DIRECTION('ref_axis',(0.,1.,0.));
#5448=DIRECTION('center_axis',(0.,-1.,0.));
#5449=DIRECTION('ref_axis',(0.852332604949105,0.,0.523000124799863));
#5450=DIRECTION('center_axis',(0.,1.,0.));
#5451=DIRECTION('ref_axis',(0.852332604949105,0.,0.523000124799863));
#5452=DIRECTION('center_axis',(0.,1.,0.));
#5453=DIRECTION('ref_axis',(0.,0.,1.));
#5454=DIRECTION('center_axis',(-0.087910671049441,0.,0.996128362168068));
#5455=DIRECTION('ref_axis',(0.,1.,0.));
#5456=DIRECTION('center_axis',(0.,1.,0.));
#5457=DIRECTION('ref_axis',(-1.,0.,1.22464679914735E-16));
#5458=DIRECTION('center_axis',(0.,-1.,0.));
#5459=DIRECTION('ref_axis',(-1.,0.,1.22464679914735E-16));
#5460=DIRECTION('center_axis',(0.,1.,0.));
#5461=DIRECTION('ref_axis',(0.,0.,1.));
#5462=DIRECTION('center_axis',(0.927906809285718,0.,0.372812222548024));
#5463=DIRECTION('ref_axis',(0.,1.,0.));
#5464=DIRECTION('center_axis',(0.,-1.,0.));
#5465=DIRECTION('ref_axis',(0.852332604949105,0.,-0.523000124799863));
#5466=DIRECTION('center_axis',(0.,1.,0.));
#5467=DIRECTION('ref_axis',(0.852332604949105,0.,-0.523000124799863));
#5468=DIRECTION('center_axis',(0.,1.,0.));
#5469=DIRECTION('ref_axis',(-0.923879532511287,0.,-0.38268343236509));
#5470=DIRECTION('center_axis',(-0.919747247828042,0.,-0.392511146482165));
#5471=DIRECTION('ref_axis',(0.,1.,0.));
#5472=DIRECTION('center_axis',(0.,1.,0.));
#5473=DIRECTION('ref_axis',(-0.923879532511287,0.,-0.38268343236509));
#5474=DIRECTION('center_axis',(0.,-1.,0.));
#5475=DIRECTION('ref_axis',(-0.923879532511287,0.,-0.38268343236509));
#5476=DIRECTION('center_axis',(0.,1.,0.));
#5477=DIRECTION('ref_axis',(0.,0.,1.));
#5478=DIRECTION('center_axis',(-0.642206888183571,0.,0.766531351459009));
#5479=DIRECTION('ref_axis',(0.,1.,0.));
#5480=DIRECTION('center_axis',(0.,-1.,0.));
#5481=DIRECTION('ref_axis',(0.232873229978512,0.,0.972507099593301));
#5482=DIRECTION('center_axis',(0.,1.,0.));
#5483=DIRECTION('ref_axis',(0.232873229978512,0.,0.972507099593301));
#5484=DIRECTION('center_axis',(0.,1.,0.));
#5485=DIRECTION('ref_axis',(0.,0.,1.));
#5486=DIRECTION('center_axis',(-0.766531351459001,0.,0.642206888183581));
#5487=DIRECTION('ref_axis',(0.,1.,0.));
#5488=DIRECTION('center_axis',(0.,1.,0.));
#5489=DIRECTION('ref_axis',(-0.707106781186548,0.,-0.707106781186547));
#5490=DIRECTION('center_axis',(0.,-1.,0.));
#5491=DIRECTION('ref_axis',(-0.707106781186548,0.,-0.707106781186547));
#5492=DIRECTION('center_axis',(0.,1.,0.));
#5493=DIRECTION('ref_axis',(0.,0.,1.));
#5494=DIRECTION('center_axis',(0.392511146482166,0.,0.919747247828041));
#5495=DIRECTION('ref_axis',(0.,1.,0.));
#5496=DIRECTION('center_axis',(0.,-1.,0.));
#5497=DIRECTION('ref_axis',(0.972507099593301,0.,0.232873229978512));
#5498=DIRECTION('center_axis',(0.,1.,0.));
#5499=DIRECTION('ref_axis',(0.972507099593301,0.,0.232873229978512));
#5500=DIRECTION('center_axis',(0.,1.,0.));
#5501=DIRECTION('ref_axis',(-0.38268343236509,0.,-0.923879532511287));
#5502=DIRECTION('center_axis',(-0.372812222548024,0.,-0.927906809285718));
#5503=DIRECTION('ref_axis',(0.,1.,0.));
#5504=DIRECTION('center_axis',(0.,1.,0.));
#5505=DIRECTION('ref_axis',(-0.38268343236509,0.,-0.923879532511287));
#5506=DIRECTION('center_axis',(0.,-1.,0.));
#5507=DIRECTION('ref_axis',(-0.38268343236509,0.,-0.923879532511287));
#5508=DIRECTION('center_axis',(0.,1.,0.));
#5509=DIRECTION('ref_axis',(0.,0.,1.));
#5510=DIRECTION('center_axis',(-0.996128362168068,0.,0.087910671049441));
#5511=DIRECTION('ref_axis',(0.,1.,0.));
#5512=DIRECTION('center_axis',(0.,1.,0.));
#5513=DIRECTION('ref_axis',(-0.523000124799863,0.,0.852332604949105));
#5514=DIRECTION('center_axis',(0.,1.,0.));
#5515=DIRECTION('ref_axis',(1.22464679914735E-16,0.,-1.));
#5516=DIRECTION('center_axis',(-0.996128362168068,0.,-0.0879106710494399));
#5517=DIRECTION('ref_axis',(0.,1.,0.));
#5518=DIRECTION('center_axis',(0.,1.,0.));
#5519=DIRECTION('ref_axis',(-1.83697019872103E-16,0.,-1.));
#5520=DIRECTION('center_axis',(0.,-1.,0.));
#5521=DIRECTION('ref_axis',(-1.83697019872103E-16,0.,-1.));
#5522=DIRECTION('center_axis',(0.,1.,0.));
#5523=DIRECTION('ref_axis',(0.,0.,1.));
#5524=DIRECTION('center_axis',(-0.372812222548024,0.,0.927906809285718));
#5525=DIRECTION('ref_axis',(0.,1.,0.));
#5526=DIRECTION('center_axis',(0.,-1.,0.));
#5527=DIRECTION('ref_axis',(0.523000124799863,0.,0.852332604949105));
#5528=DIRECTION('center_axis',(0.,1.,0.));
#5529=DIRECTION('ref_axis',(0.523000124799863,0.,0.852332604949105));
#5530=DIRECTION('center_axis',(0.,1.,0.));
#5531=DIRECTION('ref_axis',(0.38268343236509,0.,-0.923879532511287));
#5532=DIRECTION('center_axis',(0.392511146482165,0.,-0.919747247828041));
#5533=DIRECTION('ref_axis',(0.,1.,0.));
#5534=DIRECTION('center_axis',(0.,1.,0.));
#5535=DIRECTION('ref_axis',(0.38268343236509,0.,-0.923879532511287));
#5536=DIRECTION('center_axis',(0.,-1.,0.));
#5537=DIRECTION('ref_axis',(0.38268343236509,0.,-0.923879532511287));
#5538=DIRECTION('center_axis',(0.,1.,0.));
#5539=DIRECTION('ref_axis',(0.,0.,1.));
#5540=DIRECTION('center_axis',(-0.766531351459009,0.,-0.642206888183571));
#5541=DIRECTION('ref_axis',(0.,1.,0.));
#5542=DIRECTION('center_axis',(0.,-1.,0.));
#5543=DIRECTION('ref_axis',(-0.972507099593301,0.,0.232873229978513));
#5544=DIRECTION('center_axis',(0.,1.,0.));
#5545=DIRECTION('ref_axis',(-0.972507099593301,0.,0.232873229978513));
#5546=DIRECTION('center_axis',(0.,1.,0.));
#5547=DIRECTION('ref_axis',(0.,0.,1.));
#5548=DIRECTION('center_axis',(-0.642206888183576,0.,-0.766531351459005));
#5549=DIRECTION('ref_axis',(0.,1.,0.));
#5550=DIRECTION('center_axis',(0.,1.,0.));
#5551=DIRECTION('ref_axis',(0.707106781186547,0.,-0.707106781186548));
#5552=DIRECTION('center_axis',(0.,-1.,0.));
#5553=DIRECTION('ref_axis',(0.707106781186547,0.,-0.707106781186548));
#5554=DIRECTION('center_axis',(0.,1.,0.));
#5555=DIRECTION('ref_axis',(0.,0.,1.));
#5556=DIRECTION('center_axis',(-0.919747247828041,0.,0.392511146482166));
#5557=DIRECTION('ref_axis',(0.,1.,0.));
#5558=DIRECTION('center_axis',(0.,-1.,0.));
#5559=DIRECTION('ref_axis',(-0.232873229978512,0.,0.972507099593301));
#5560=DIRECTION('center_axis',(0.,1.,0.));
#5561=DIRECTION('ref_axis',(-0.232873229978512,0.,0.972507099593301));
#5562=DIRECTION('center_axis',(0.,1.,0.));
#5563=DIRECTION('ref_axis',(0.923879532511287,0.,-0.38268343236509));
#5564=DIRECTION('center_axis',(0.927906809285716,0.,-0.37281222254803));
#5565=DIRECTION('ref_axis',(0.,1.,0.));
#5566=DIRECTION('center_axis',(0.,1.,0.));
#5567=DIRECTION('ref_axis',(0.923879532511287,0.,-0.382683432365089));
#5568=DIRECTION('center_axis',(0.,-1.,0.));
#5569=DIRECTION('ref_axis',(0.923879532511287,0.,-0.382683432365089));
#5570=DIRECTION('center_axis',(0.,1.,0.));
#5571=DIRECTION('ref_axis',(0.,0.,1.));
#5572=DIRECTION('center_axis',(-0.0879106710494421,0.,-0.996128362168068));
#5573=DIRECTION('ref_axis',(0.,1.,0.));
#5574=DIRECTION('center_axis',(0.,-1.,0.));
#5575=DIRECTION('ref_axis',(-0.852332604949105,0.,-0.523000124799863));
#5576=DIRECTION('center_axis',(0.,1.,0.));
#5577=DIRECTION('ref_axis',(-0.852332604949105,0.,-0.523000124799863));
#5578=DIRECTION('center_axis',(0.,1.,0.));
#5579=DIRECTION('ref_axis',(0.,0.,1.));
#5580=DIRECTION('center_axis',(0.0879106710494428,0.,-0.996128362168068));
#5581=DIRECTION('ref_axis',(0.,1.,0.));
#5582=DIRECTION('center_axis',(0.,1.,0.));
#5583=DIRECTION('ref_axis',(1.,0.,-2.44929359829471E-16));
#5584=DIRECTION('center_axis',(0.,-1.,0.));
#5585=DIRECTION('ref_axis',(1.,0.,-2.44929359829471E-16));
#5586=DIRECTION('center_axis',(0.,1.,0.));
#5587=DIRECTION('ref_axis',(0.,0.,1.));
#5588=DIRECTION('center_axis',(-0.927906809285717,0.,-0.372812222548027));
#5589=DIRECTION('ref_axis',(0.,1.,0.));
#5590=DIRECTION('center_axis',(0.,-1.,0.));
#5591=DIRECTION('ref_axis',(-0.852332604949106,0.,0.523000124799863));
#5592=DIRECTION('center_axis',(0.,1.,0.));
#5593=DIRECTION('ref_axis',(-0.852332604949106,0.,0.523000124799863));
#5594=DIRECTION('center_axis',(0.,1.,0.));
#5595=DIRECTION('ref_axis',(0.,0.,1.));
#5596=DIRECTION('center_axis',(0.919747247828042,0.,0.392511146482165));
#5597=DIRECTION('ref_axis',(0.,1.,0.));
#5598=DIRECTION('center_axis',(0.,1.,0.));
#5599=DIRECTION('ref_axis',(0.923879532511286,0.,0.382683432365091));
#5600=DIRECTION('center_axis',(0.,-1.,0.));
#5601=DIRECTION('ref_axis',(0.923879532511286,0.,0.382683432365091));
#5602=DIRECTION('center_axis',(0.,1.,0.));
#5603=DIRECTION('ref_axis',(-0.232873229978513,0.,-0.972507099593301));
#5604=DIRECTION('center_axis',(0.642206888183571,0.,-0.766531351459009));
#5605=DIRECTION('ref_axis',(0.,1.,0.));
#5606=DIRECTION('center_axis',(0.,-1.,0.));
#5607=DIRECTION('ref_axis',(-0.232873229978514,0.,-0.972507099593301));
#5608=DIRECTION('center_axis',(0.,1.,0.));
#5609=DIRECTION('ref_axis',(-0.232873229978514,0.,-0.972507099593301));
#5610=DIRECTION('center_axis',(0.,1.,0.));
#5611=DIRECTION('ref_axis',(0.,0.,1.));
#5612=DIRECTION('center_axis',(0.766531351459006,0.,-0.642206888183574));
#5613=DIRECTION('ref_axis',(0.,1.,0.));
#5614=DIRECTION('center_axis',(0.,1.,0.));
#5615=DIRECTION('ref_axis',(0.707106781186547,0.,0.707106781186547));
#5616=DIRECTION('center_axis',(0.,-1.,0.));
#5617=DIRECTION('ref_axis',(0.707106781186547,0.,0.707106781186547));
#5618=DIRECTION('center_axis',(0.,1.,0.));
#5619=DIRECTION('ref_axis',(0.,0.,1.));
#5620=DIRECTION('center_axis',(-0.392511146482166,0.,-0.919747247828041));
#5621=DIRECTION('ref_axis',(0.,1.,0.));
#5622=DIRECTION('center_axis',(0.,-1.,0.));
#5623=DIRECTION('ref_axis',(-0.972507099593301,0.,-0.232873229978513));
#5624=DIRECTION('center_axis',(0.,1.,0.));
#5625=DIRECTION('ref_axis',(-0.972507099593301,0.,-0.232873229978513));
#5626=DIRECTION('center_axis',(0.,1.,0.));
#5627=DIRECTION('ref_axis',(0.,0.,1.));
#5628=DIRECTION('center_axis',(0.37281222254803,0.,0.927906809285716));
#5629=DIRECTION('ref_axis',(0.,1.,0.));
#5630=DIRECTION('center_axis',(0.,1.,0.));
#5631=DIRECTION('ref_axis',(0.382683432365089,0.,0.923879532511287));
#5632=DIRECTION('center_axis',(0.,-1.,0.));
#5633=DIRECTION('ref_axis',(0.382683432365089,0.,0.923879532511287));
#5634=DIRECTION('center_axis',(0.,1.,0.));
#5635=DIRECTION('ref_axis',(0.523000124799863,0.,-0.852332604949105));
#5636=DIRECTION('center_axis',(0.996128362168068,0.,-0.0879106710494421));
#5637=DIRECTION('ref_axis',(0.,1.,0.));
#5638=DIRECTION('center_axis',(0.,-1.,0.));
#5639=DIRECTION('ref_axis',(0.523000124799863,0.,-0.852332604949105));
#5640=DIRECTION('center_axis',(0.,1.,0.));
#5641=DIRECTION('ref_axis',(0.523000124799863,0.,-0.852332604949105));
#5642=DIRECTION('center_axis',(0.,1.,0.));
#5643=DIRECTION('ref_axis',(0.,0.,1.));
#5644=DIRECTION('center_axis',(0.,-1.,0.));
#5645=DIRECTION('ref_axis',(6.12323399573677E-17,0.,1.));
#5646=DIRECTION('center_axis',(0.,1.,0.));
#5647=DIRECTION('ref_axis',(0.38268343236509,0.,-0.923879532511287));
#5648=DIRECTION('',(0.,1.,0.));
#5649=DIRECTION('center_axis',(0.,-1.,0.));
#5650=DIRECTION('ref_axis',(0.38268343236509,0.,-0.923879532511287));
#5651=DIRECTION('',(0.,-1.,0.));
#5652=DIRECTION('center_axis',(0.,1.,0.));
#5653=DIRECTION('ref_axis',(-0.972507099593301,0.,0.232873229978513));
#5654=DIRECTION('',(0.,-1.,0.));
#5655=DIRECTION('center_axis',(0.,1.,0.));
#5656=DIRECTION('ref_axis',(-0.972507099593301,0.,0.232873229978513));
#5657=DIRECTION('center_axis',(0.,-1.,0.));
#5658=DIRECTION('ref_axis',(1.,0.,0.));
#5659=DIRECTION('',(0.,1.,0.));
#5660=DIRECTION('center_axis',(0.,-1.,0.));
#5661=DIRECTION('ref_axis',(0.707106781186547,0.,-0.707106781186547));
#5662=DIRECTION('center_axis',(0.,-1.,0.));
#5663=DIRECTION('ref_axis',(-0.232873229978513,0.,0.972507099593301));
#5664=DIRECTION('',(0.,-1.,0.));
#5665=DIRECTION('center_axis',(0.,1.,0.));
#5666=DIRECTION('ref_axis',(-0.232873229978512,0.,0.972507099593301));
#5667=DIRECTION('center_axis',(0.,1.,0.));
#5668=DIRECTION('ref_axis',(0.923879532511287,0.,-0.382683432365089));
#5669=DIRECTION('',(0.,1.,0.));
#5670=DIRECTION('center_axis',(0.,-1.,0.));
#5671=DIRECTION('ref_axis',(0.923879532511287,0.,-0.382683432365089));
#5672=DIRECTION('center_axis',(0.,1.,0.));
#5673=DIRECTION('ref_axis',(-0.852332604949105,0.,-0.523000124799864));
#5674=DIRECTION('',(0.,-1.,0.));
#5675=DIRECTION('center_axis',(0.,1.,0.));
#5676=DIRECTION('ref_axis',(-0.852332604949105,0.,-0.523000124799863));
#5677=DIRECTION('center_axis',(0.,-1.,0.));
#5678=DIRECTION('ref_axis',(1.,0.,0.));
#5679=DIRECTION('',(0.,1.,0.));
#5680=DIRECTION('center_axis',(0.,-1.,0.));
#5681=DIRECTION('ref_axis',(1.,0.,1.17961196366423E-16));
#5682=DIRECTION('center_axis',(0.,-1.,0.));
#5683=DIRECTION('ref_axis',(-0.852332604949106,0.,0.523000124799862));
#5684=DIRECTION('',(0.,-1.,0.));
#5685=DIRECTION('center_axis',(0.,1.,0.));
#5686=DIRECTION('ref_axis',(-0.852332604949106,0.,0.523000124799863));
#5687=DIRECTION('center_axis',(0.,1.,0.));
#5688=DIRECTION('ref_axis',(0.923879532511287,0.,0.38268343236509));
#5689=DIRECTION('',(0.,1.,0.));
#5690=DIRECTION('center_axis',(0.,-1.,0.));
#5691=DIRECTION('ref_axis',(0.923879532511286,0.,0.382683432365091));
#5692=DIRECTION('center_axis',(0.,1.,0.));
#5693=DIRECTION('ref_axis',(-0.232873229978514,0.,-0.972507099593301));
#5694=DIRECTION('',(0.,-1.,0.));
#5695=DIRECTION('center_axis',(0.,1.,0.));
#5696=DIRECTION('ref_axis',(-0.232873229978514,0.,-0.972507099593301));
#5697=DIRECTION('center_axis',(0.,-1.,0.));
#5698=DIRECTION('ref_axis',(1.,0.,0.));
#5699=DIRECTION('',(0.,1.,0.));
#5700=DIRECTION('center_axis',(0.,-1.,0.));
#5701=DIRECTION('ref_axis',(0.707106781186547,0.,0.707106781186548));
#5702=DIRECTION('center_axis',(0.,-1.,0.));
#5703=DIRECTION('ref_axis',(-0.972507099593301,0.,-0.232873229978514));
#5704=DIRECTION('',(0.,-1.,0.));
#5705=DIRECTION('center_axis',(0.,1.,0.));
#5706=DIRECTION('ref_axis',(-0.972507099593301,0.,-0.232873229978513));
#5707=DIRECTION('center_axis',(0.,1.,0.));
#5708=DIRECTION('ref_axis',(0.382683432365089,0.,0.923879532511287));
#5709=DIRECTION('',(0.,1.,0.));
#5710=DIRECTION('center_axis',(0.,-1.,0.));
#5711=DIRECTION('ref_axis',(0.382683432365089,0.,0.923879532511287));
#5712=DIRECTION('center_axis',(0.,1.,0.));
#5713=DIRECTION('ref_axis',(0.523000124799864,0.,-0.852332604949105));
#5714=DIRECTION('',(0.,-1.,0.));
#5715=DIRECTION('center_axis',(0.,1.,0.));
#5716=DIRECTION('ref_axis',(0.523000124799863,0.,-0.852332604949105));
#5717=DIRECTION('center_axis',(0.,-1.,0.));
#5718=DIRECTION('ref_axis',(1.,0.,0.));
#5719=DIRECTION('center_axis',(0.,-1.,0.));
#5720=DIRECTION('ref_axis',(-1.83697019872103E-16,0.,1.));
#5721=DIRECTION('center_axis',(0.,1.,0.));
#5722=DIRECTION('ref_axis',(1.,0.,0.));
#5723=DIRECTION('center_axis',(0.,1.,0.));
#5724=DIRECTION('ref_axis',(1.,0.,0.));
#5725=DIRECTION('center_axis',(0.,-1.,0.));
#5726=DIRECTION('ref_axis',(-0.38268343236509,0.,-0.923879532511287));
#5727=DIRECTION('center_axis',(0.,-1.,0.));
#5728=DIRECTION('ref_axis',(-0.923879532511287,0.,0.38268343236509));
#5729=DIRECTION('center_axis',(0.,-1.,0.));
#5730=DIRECTION('ref_axis',(-0.923879532511287,0.,-0.38268343236509));
#5731=DIRECTION('center_axis',(0.,-1.,0.));
#5732=DIRECTION('ref_axis',(0.923879532511287,0.,-0.38268343236509));
#5733=DIRECTION('center_axis',(0.,-1.,0.));
#5734=DIRECTION('ref_axis',(0.923879532511287,0.,0.38268343236509));
#5735=DIRECTION('center_axis',(0.,-1.,0.));
#5736=DIRECTION('ref_axis',(0.38268343236509,0.,-0.923879532511287));
#5737=DIRECTION('center_axis',(0.,-1.,0.));
#5738=DIRECTION('ref_axis',(0.38268343236509,0.,0.923879532511287));
#5739=DIRECTION('center_axis',(0.,-1.,0.));
#5740=DIRECTION('ref_axis',(-0.38268343236509,0.,0.923879532511287));
#5741=DIRECTION('center_axis',(0.,-1.,0.));
#5742=DIRECTION('ref_axis',(0.,0.,-1.));
#5743=DIRECTION('center_axis',(0.766531351459009,0.,0.642206888183571));
#5744=DIRECTION('ref_axis',(-0.642206888183571,0.,0.766531351459009));
#5745=DIRECTION('center_axis',(0.,-1.,0.));
#5746=DIRECTION('ref_axis',(0.972507099593301,0.,-0.232873229978514));
#5747=DIRECTION('center_axis',(0.392511146482161,0.,-0.919747247828043));
#5748=DIRECTION('ref_axis',(0.,-1.,0.));
#5749=DIRECTION('center_axis',(0.,1.,0.));
#5750=DIRECTION('ref_axis',(0.972507099593301,0.,-0.232873229978514));
#5751=DIRECTION('center_axis',(0.,-1.,0.));
#5752=DIRECTION('ref_axis',(-0.38268343236509,0.,0.923879532511287));
#5753=DIRECTION('center_axis',(-0.372812222548022,0.,0.927906809285719));
#5754=DIRECTION('ref_axis',(0.,-1.,0.));
#5755=DIRECTION('center_axis',(0.,-1.,0.));
#5756=DIRECTION('ref_axis',(-0.382683432365091,0.,0.923879532511286));
#5757=DIRECTION('center_axis',(0.,1.,0.));
#5758=DIRECTION('ref_axis',(-0.382683432365091,0.,0.923879532511286));
#5759=DIRECTION('center_axis',(0.,-1.,0.));
#5760=DIRECTION('ref_axis',(0.,0.,-1.));
#5761=DIRECTION('center_axis',(-0.996128362168068,0.,-0.0879106710494425));
#5762=DIRECTION('ref_axis',(0.,-1.,0.));
#5763=DIRECTION('center_axis',(0.,-1.,0.));
#5764=DIRECTION('ref_axis',(-0.523000124799863,0.,-0.852332604949106));
#5765=DIRECTION('center_axis',(0.,-1.,0.));
#5766=DIRECTION('ref_axis',(1.22464679914735E-16,0.,1.));
#5767=DIRECTION('center_axis',(-0.996128362168068,0.,0.087910671049441));
#5768=DIRECTION('ref_axis',(0.,-1.,0.));
#5769=DIRECTION('center_axis',(0.,1.,0.));
#5770=DIRECTION('ref_axis',(-1.83697019872103E-16,0.,1.));
#5771=DIRECTION('center_axis',(0.,-1.,0.));
#5772=DIRECTION('ref_axis',(0.,0.,-1.));
#5773=DIRECTION('center_axis',(-0.372812222548023,0.,-0.927906809285719));
#5774=DIRECTION('ref_axis',(0.,-1.,0.));
#5775=DIRECTION('center_axis',(0.,-1.,0.));
#5776=DIRECTION('ref_axis',(0.523000124799863,0.,-0.852332604949105));
#5777=DIRECTION('center_axis',(0.,-1.,0.));
#5778=DIRECTION('ref_axis',(0.382683432365089,0.,0.923879532511287));
#5779=DIRECTION('center_axis',(0.392511146482171,0.,0.919747247828039));
#5780=DIRECTION('ref_axis',(0.,-1.,0.));
#5781=DIRECTION('center_axis',(0.,1.,0.));
#5782=DIRECTION('ref_axis',(0.382683432365089,0.,0.923879532511287));
#5783=DIRECTION('center_axis',(0.,-1.,0.));
#5784=DIRECTION('ref_axis',(0.,0.,-1.));
#5785=DIRECTION('center_axis',(-0.766531351459011,0.,0.642206888183568));
#5786=DIRECTION('ref_axis',(0.,-1.,0.));
#5787=DIRECTION('center_axis',(0.,-1.,0.));
#5788=DIRECTION('ref_axis',(-0.972507099593301,0.,-0.232873229978513));
#5789=DIRECTION('center_axis',(0.,-1.,0.));
#5790=DIRECTION('ref_axis',(0.,0.,-1.));
#5791=DIRECTION('center_axis',(-0.642206888183576,0.,0.766531351459005));
#5792=DIRECTION('ref_axis',(0.,-1.,0.));
#5793=DIRECTION('center_axis',(0.,1.,0.));
#5794=DIRECTION('ref_axis',(0.707106781186547,0.,0.707106781186548));
#5795=DIRECTION('center_axis',(0.,-1.,0.));
#5796=DIRECTION('ref_axis',(0.,0.,-1.));
#5797=DIRECTION('center_axis',(-0.919747247828043,0.,-0.392511146482161));
#5798=DIRECTION('ref_axis',(0.,-1.,0.));
#5799=DIRECTION('center_axis',(0.,-1.,0.));
#5800=DIRECTION('ref_axis',(-0.232873229978514,0.,-0.972507099593301));
#5801=DIRECTION('center_axis',(0.,-1.,0.));
#5802=DIRECTION('ref_axis',(0.923879532511287,0.,0.38268343236509));
#5803=DIRECTION('center_axis',(0.92790680928572,0.,0.372812222548021));
#5804=DIRECTION('ref_axis',(0.,-1.,0.));
#5805=DIRECTION('center_axis',(0.,1.,0.));
#5806=DIRECTION('ref_axis',(0.923879532511286,0.,0.382683432365091));
#5807=DIRECTION('center_axis',(0.,-1.,0.));
#5808=DIRECTION('ref_axis',(0.,0.,-1.));
#5809=DIRECTION('center_axis',(-0.0879106710494425,0.,0.996128362168068));
#5810=DIRECTION('ref_axis',(0.,-1.,0.));
#5811=DIRECTION('center_axis',(0.,-1.,0.));
#5812=DIRECTION('ref_axis',(-0.852332604949106,0.,0.523000124799863));
#5813=DIRECTION('center_axis',(0.,-1.,0.));
#5814=DIRECTION('ref_axis',(0.,0.,-1.));
#5815=DIRECTION('center_axis',(0.0879106710494399,0.,0.996128362168068));
#5816=DIRECTION('ref_axis',(0.,-1.,0.));
#5817=DIRECTION('center_axis',(0.,1.,0.));
#5818=DIRECTION('ref_axis',(1.,0.,1.17961196366423E-16));
#5819=DIRECTION('center_axis',(0.,-1.,0.));
#5820=DIRECTION('ref_axis',(0.,0.,-1.));
#5821=DIRECTION('center_axis',(-0.927906809285719,0.,0.372812222548023));
#5822=DIRECTION('ref_axis',(0.,-1.,0.));
#5823=DIRECTION('center_axis',(0.,-1.,0.));
#5824=DIRECTION('ref_axis',(-0.852332604949105,0.,-0.523000124799863));
#5825=DIRECTION('center_axis',(0.,-1.,0.));
#5826=DIRECTION('ref_axis',(0.,0.,-1.));
#5827=DIRECTION('center_axis',(0.919747247828038,0.,-0.392511146482172));
#5828=DIRECTION('ref_axis',(0.,-1.,0.));
#5829=DIRECTION('center_axis',(0.,1.,0.));
#5830=DIRECTION('ref_axis',(0.923879532511287,0.,-0.382683432365089));
#5831=DIRECTION('center_axis',(0.,-1.,0.));
#5832=DIRECTION('ref_axis',(-0.232873229978513,0.,0.972507099593301));
#5833=DIRECTION('center_axis',(0.642206888183571,0.,0.766531351459009));
#5834=DIRECTION('ref_axis',(0.,-1.,0.));
#5835=DIRECTION('center_axis',(0.,-1.,0.));
#5836=DIRECTION('ref_axis',(-0.232873229978512,0.,0.972507099593301));
#5837=DIRECTION('center_axis',(0.,-1.,0.));
#5838=DIRECTION('ref_axis',(0.,0.,-1.));
#5839=DIRECTION('center_axis',(0.766531351459006,0.,0.642206888183574));
#5840=DIRECTION('ref_axis',(0.,-1.,0.));
#5841=DIRECTION('center_axis',(0.,1.,0.));
#5842=DIRECTION('ref_axis',(0.707106781186547,0.,-0.707106781186547));
#5843=DIRECTION('center_axis',(0.,-1.,0.));
#5844=DIRECTION('ref_axis',(0.,0.,-1.));
#5845=DIRECTION('center_axis',(-0.392511146482168,0.,0.91974724782804));
#5846=DIRECTION('ref_axis',(0.,-1.,0.));
#5847=DIRECTION('center_axis',(0.,-1.,0.));
#5848=DIRECTION('ref_axis',(-0.972507099593301,0.,0.232873229978513));
#5849=DIRECTION('center_axis',(0.,-1.,0.));
#5850=DIRECTION('ref_axis',(0.,0.,-1.));
#5851=DIRECTION('center_axis',(0.372812222548023,0.,-0.927906809285719));
#5852=DIRECTION('ref_axis',(0.,-1.,0.));
#5853=DIRECTION('center_axis',(0.,1.,0.));
#5854=DIRECTION('ref_axis',(0.38268343236509,0.,-0.923879532511287));
#5855=DIRECTION('center_axis',(0.,-1.,0.));
#5856=DIRECTION('ref_axis',(0.523000124799863,0.,0.852332604949105));
#5857=DIRECTION('center_axis',(0.996128362168068,0.,0.087910671049441));
#5858=DIRECTION('ref_axis',(0.,-1.,0.));
#5859=DIRECTION('center_axis',(0.,1.,0.));
#5860=DIRECTION('ref_axis',(0.523000124799863,0.,0.852332604949105));
#5861=DIRECTION('center_axis',(0.,-1.,0.));
#5862=DIRECTION('ref_axis',(0.523000124799863,0.,0.852332604949105));
#5863=DIRECTION('center_axis',(0.,-1.,0.));
#5864=DIRECTION('ref_axis',(0.,0.,-1.));
#5865=DIRECTION('center_axis',(0.996128362168068,0.,-0.0879106710494399));
#5866=DIRECTION('ref_axis',(0.,-1.,0.));
#5867=DIRECTION('center_axis',(0.,1.,0.));
#5868=DIRECTION('ref_axis',(-1.60812264967664E-16,0.,-1.));
#5869=DIRECTION('center_axis',(0.,-1.,0.));
#5870=DIRECTION('ref_axis',(-0.523000124799863,0.,0.852332604949106));
#5871=DIRECTION('center_axis',(0.372812222548025,0.,0.927906809285718));
#5872=DIRECTION('ref_axis',(0.,-1.,0.));
#5873=DIRECTION('center_axis',(0.,-1.,0.));
#5874=DIRECTION('ref_axis',(-0.523000124799863,0.,0.852332604949105));
#5875=DIRECTION('center_axis',(0.,-1.,0.));
#5876=DIRECTION('ref_axis',(0.,0.,-1.));
#5877=DIRECTION('center_axis',(-0.392511146482174,0.,-0.919747247828038));
#5878=DIRECTION('ref_axis',(0.,-1.,0.));
#5879=DIRECTION('center_axis',(0.,-1.,0.));
#5880=DIRECTION('ref_axis',(-0.38268343236509,0.,-0.923879532511287));
#5881=DIRECTION('center_axis',(0.,1.,0.));
#5882=DIRECTION('ref_axis',(-0.38268343236509,0.,-0.923879532511287));
#5883=DIRECTION('center_axis',(0.,-1.,0.));
#5884=DIRECTION('ref_axis',(0.,0.,-1.));
#5885=DIRECTION('center_axis',(0.766531351459009,0.,-0.642206888183571));
#5886=DIRECTION('ref_axis',(0.,-1.,0.));
#5887=DIRECTION('center_axis',(0.,1.,0.));
#5888=DIRECTION('ref_axis',(0.972507099593301,0.,0.232873229978512));
#5889=DIRECTION('center_axis',(0.,-1.,0.));
#5890=DIRECTION('ref_axis',(0.972507099593301,0.,0.232873229978512));
#5891=DIRECTION('center_axis',(0.,-1.,0.));
#5892=DIRECTION('ref_axis',(0.,0.,-1.));
#5893=DIRECTION('center_axis',(0.642206888183569,0.,-0.76653135145901));
#5894=DIRECTION('ref_axis',(0.,-1.,0.));
#5895=DIRECTION('center_axis',(0.,-1.,0.));
#5896=DIRECTION('ref_axis',(-0.707106781186547,0.,-0.707106781186548));
#5897=DIRECTION('center_axis',(0.,1.,0.));
#5898=DIRECTION('ref_axis',(-0.707106781186547,0.,-0.707106781186548));
#5899=DIRECTION('center_axis',(0.,-1.,0.));
#5900=DIRECTION('ref_axis',(0.232873229978514,0.,0.972507099593301));
#5901=DIRECTION('center_axis',(0.919747247828041,0.,0.392511146482166));
#5902=DIRECTION('ref_axis',(0.,-1.,0.));
#5903=DIRECTION('center_axis',(0.,1.,0.));
#5904=DIRECTION('ref_axis',(0.232873229978512,0.,0.972507099593301));
#5905=DIRECTION('center_axis',(0.,-1.,0.));
#5906=DIRECTION('ref_axis',(0.232873229978512,0.,0.972507099593301));
#5907=DIRECTION('center_axis',(0.,-1.,0.));
#5908=DIRECTION('ref_axis',(0.,0.,-1.));
#5909=DIRECTION('center_axis',(-0.927906809285719,0.,-0.372812222548023));
#5910=DIRECTION('ref_axis',(0.,-1.,0.));
#5911=DIRECTION('center_axis',(0.,-1.,0.));
#5912=DIRECTION('ref_axis',(-0.923879532511287,0.,-0.38268343236509));
#5913=DIRECTION('center_axis',(0.,1.,0.));
#5914=DIRECTION('ref_axis',(-0.923879532511287,0.,-0.38268343236509));
#5915=DIRECTION('center_axis',(0.,-1.,0.));
#5916=DIRECTION('ref_axis',(0.,0.,-1.));
#5917=DIRECTION('center_axis',(0.0879106710494421,0.,-0.996128362168068));
#5918=DIRECTION('ref_axis',(0.,-1.,0.));
#5919=DIRECTION('center_axis',(0.,1.,0.));
#5920=DIRECTION('ref_axis',(0.852332604949105,0.,-0.523000124799863));
#5921=DIRECTION('center_axis',(0.,-1.,0.));
#5922=DIRECTION('ref_axis',(0.852332604949105,0.,-0.523000124799863));
#5923=DIRECTION('center_axis',(0.,-1.,0.));
#5924=DIRECTION('ref_axis',(0.,0.,-1.));
#5925=DIRECTION('center_axis',(-0.0879106710494421,0.,-0.996128362168068));
#5926=DIRECTION('ref_axis',(0.,-1.,0.));
#5927=DIRECTION('center_axis',(0.,-1.,0.));
#5928=DIRECTION('ref_axis',(-1.,0.,-1.22464679914735E-16));
#5929=DIRECTION('center_axis',(0.,1.,0.));
#5930=DIRECTION('ref_axis',(-1.,0.,-1.22464679914735E-16));
#5931=DIRECTION('center_axis',(0.,-1.,0.));
#5932=DIRECTION('ref_axis',(0.,0.,-1.));
#5933=DIRECTION('center_axis',(0.927906809285717,0.,-0.372812222548027));
#5934=DIRECTION('ref_axis',(0.,-1.,0.));
#5935=DIRECTION('center_axis',(0.,1.,0.));
#5936=DIRECTION('ref_axis',(0.852332604949105,0.,0.523000124799863));
#5937=DIRECTION('center_axis',(0.,-1.,0.));
#5938=DIRECTION('ref_axis',(0.852332604949105,0.,0.523000124799863));
#5939=DIRECTION('center_axis',(0.,-1.,0.));
#5940=DIRECTION('ref_axis',(-0.923879532511287,0.,0.382683432365089));
#5941=DIRECTION('center_axis',(-0.919747247828039,0.,0.392511146482171));
#5942=DIRECTION('ref_axis',(0.,-1.,0.));
#5943=DIRECTION('center_axis',(0.,-1.,0.));
#5944=DIRECTION('ref_axis',(-0.923879532511287,0.,0.382683432365089));
#5945=DIRECTION('center_axis',(0.,1.,0.));
#5946=DIRECTION('ref_axis',(-0.923879532511287,0.,0.382683432365089));
#5947=DIRECTION('center_axis',(0.,-1.,0.));
#5948=DIRECTION('ref_axis',(0.,0.,-1.));
#5949=DIRECTION('center_axis',(-0.642206888183565,0.,-0.766531351459014));
#5950=DIRECTION('ref_axis',(0.,-1.,0.));
#5951=DIRECTION('center_axis',(0.,1.,0.));
#5952=DIRECTION('ref_axis',(0.232873229978513,0.,-0.972507099593301));
#5953=DIRECTION('center_axis',(0.,-1.,0.));
#5954=DIRECTION('ref_axis',(0.232873229978513,0.,-0.972507099593301));
#5955=DIRECTION('center_axis',(0.,-1.,0.));
#5956=DIRECTION('ref_axis',(0.,0.,-1.));
#5957=DIRECTION('center_axis',(0.,1.,0.));
#5958=DIRECTION('ref_axis',(-0.707106781186548,0.,0.707106781186547));
#5959=DIRECTION('center_axis',(0.,-1.,0.));
#5960=DIRECTION('ref_axis',(-0.707106781186548,0.,0.707106781186547));
#5961=DIRECTION('center_axis',(0.,-1.,0.));
#5962=DIRECTION('ref_axis',(0.523000124799864,0.,0.852332604949105));
#5963=DIRECTION('',(0.,1.,0.));
#5964=DIRECTION('center_axis',(0.,-1.,0.));
#5965=DIRECTION('ref_axis',(1.,0.,0.));
#5966=DIRECTION('center_axis',(0.,1.,0.));
#5967=DIRECTION('ref_axis',(-0.38268343236509,0.,-0.923879532511287));
#5968=DIRECTION('',(0.,-1.,0.));
#5969=DIRECTION('center_axis',(0.,-1.,0.));
#5970=DIRECTION('ref_axis',(0.972507099593301,0.,0.232873229978513));
#5971=DIRECTION('',(0.,1.,0.));
#5972=DIRECTION('center_axis',(0.,-1.,0.));
#5973=DIRECTION('ref_axis',(1.,0.,0.));
#5974=DIRECTION('',(0.,-1.,0.));
#5975=DIRECTION('center_axis',(0.,1.,0.));
#5976=DIRECTION('ref_axis',(0.232873229978513,0.,0.972507099593301));
#5977=DIRECTION('',(0.,1.,0.));
#5978=DIRECTION('center_axis',(0.,1.,0.));
#5979=DIRECTION('ref_axis',(-0.923879532511287,0.,-0.38268343236509));
#5980=DIRECTION('',(0.,-1.,0.));
#5981=DIRECTION('center_axis',(0.,-1.,0.));
#5982=DIRECTION('ref_axis',(0.852332604949105,0.,-0.523000124799864));
#5983=DIRECTION('',(0.,1.,0.));
#5984=DIRECTION('center_axis',(0.,-1.,0.));
#5985=DIRECTION('ref_axis',(-1.,0.,1.22464679914735E-16));
#5986=DIRECTION('',(0.,-1.,0.));
#5987=DIRECTION('center_axis',(0.,1.,0.));
#5988=DIRECTION('ref_axis',(0.852332604949106,0.,0.523000124799863));
#5989=DIRECTION('',(0.,1.,0.));
#5990=DIRECTION('center_axis',(0.,1.,0.));
#5991=DIRECTION('ref_axis',(-0.923879532511287,0.,0.38268343236509));
#5992=DIRECTION('',(0.,-1.,0.));
#5993=DIRECTION('center_axis',(0.,-1.,0.));
#5994=DIRECTION('ref_axis',(0.232873229978513,0.,-0.972507099593301));
#5995=DIRECTION('',(0.,1.,0.));
#5996=DIRECTION('center_axis',(0.,-1.,0.));
#5997=DIRECTION('ref_axis',(1.,0.,0.));
#5998=DIRECTION('',(0.,-1.,0.));
#5999=DIRECTION('center_axis',(0.,1.,0.));
#6000=DIRECTION('ref_axis',(0.972507099593301,0.,-0.232873229978514));
#6001=DIRECTION('',(0.,1.,0.));
#6002=DIRECTION('center_axis',(0.,1.,0.));
#6003=DIRECTION('ref_axis',(1.,0.,0.));
#6004=DIRECTION('center_axis',(0.,-1.,0.));
#6005=DIRECTION('ref_axis',(1.,0.,0.));
#6006=DIRECTION('center_axis',(0.,1.,0.));
#6007=DIRECTION('ref_axis',(-0.38268343236509,0.,-0.923879532511287));
#6008=DIRECTION('center_axis',(0.,1.,0.));
#6009=DIRECTION('ref_axis',(0.923879532511287,0.,0.38268343236509));
#6010=DIRECTION('center_axis',(0.,1.,0.));
#6011=DIRECTION('ref_axis',(0.923879532511287,0.,-0.38268343236509));
#6012=DIRECTION('center_axis',(0.,1.,0.));
#6013=DIRECTION('ref_axis',(0.38268343236509,0.,-0.923879532511287));
#6014=DIRECTION('center_axis',(0.,1.,0.));
#6015=DIRECTION('ref_axis',(-0.923879532511287,0.,-0.38268343236509));
#6016=DIRECTION('center_axis',(0.,1.,0.));
#6017=DIRECTION('ref_axis',(0.38268343236509,0.,0.923879532511287));
#6018=DIRECTION('center_axis',(0.,1.,0.));
#6019=DIRECTION('ref_axis',(-0.923879532511287,0.,0.38268343236509));
#6020=DIRECTION('center_axis',(0.,1.,0.));
#6021=DIRECTION('ref_axis',(-0.38268343236509,0.,0.923879532511287));
#6022=DIRECTION('center_axis',(0.,-1.,0.));
#6023=DIRECTION('ref_axis',(0.,0.,-1.));
#6024=DIRECTION('center_axis',(-1.,0.,-1.22464679914735E-16));
#6025=DIRECTION('ref_axis',(-1.22464679914735E-16,0.,1.));
#6026=DIRECTION('center_axis',(0.,-1.,0.));
#6027=DIRECTION('ref_axis',(1.,0.,0.));
#6028=DIRECTION('center_axis',(0.,-1.,0.));
#6029=DIRECTION('ref_axis',(1.,0.,0.));
#6030=DIRECTION('center_axis',(0.,-1.,0.));
#6031=DIRECTION('ref_axis',(1.,0.,0.));
#6032=DIRECTION('',(0.,-1.,0.));
#6033=DIRECTION('center_axis',(0.,1.,0.));
#6034=DIRECTION('ref_axis',(1.,0.,0.));
#6035=DIRECTION('center_axis',(0.,1.,0.));
#6036=DIRECTION('ref_axis',(1.,0.,0.));
#6037=DIRECTION('center_axis',(0.,1.,0.));
#6038=DIRECTION('ref_axis',(0.,0.,1.));
#6039=DIRECTION('center_axis',(-1.,0.,1.22464679914735E-16));
#6040=DIRECTION('ref_axis',(-1.22464679914735E-16,0.,-1.));
#6041=DIRECTION('center_axis',(0.,1.,0.));
#6042=DIRECTION('ref_axis',(-0.38268343236509,0.,0.923879532511287));
#6043=DIRECTION('center_axis',(0.,1.,0.));
#6044=DIRECTION('ref_axis',(-0.38268343236509,0.,-0.923879532511287));
#6045=DIRECTION('',(0.,1.,0.));
#6046=DIRECTION('center_axis',(0.,1.,0.));
#6047=DIRECTION('ref_axis',(-0.38268343236509,0.,0.923879532511287));
#6048=DIRECTION('',(0.,1.,0.));
#6049=DIRECTION('center_axis',(0.,1.,0.));
#6050=DIRECTION('ref_axis',(-0.923879532511287,0.,0.38268343236509));
#6051=DIRECTION('',(0.,1.,0.));
#6052=DIRECTION('center_axis',(0.,1.,0.));
#6053=DIRECTION('ref_axis',(0.38268343236509,0.,0.923879532511287));
#6054=DIRECTION('',(0.,1.,0.));
#6055=DIRECTION('center_axis',(0.,1.,0.));
#6056=DIRECTION('ref_axis',(-0.923879532511287,0.,-0.38268343236509));
#6057=DIRECTION('',(0.,1.,0.));
#6058=DIRECTION('center_axis',(0.,1.,0.));
#6059=DIRECTION('ref_axis',(0.38268343236509,0.,-0.923879532511287));
#6060=DIRECTION('',(0.,1.,0.));
#6061=DIRECTION('center_axis',(0.,1.,0.));
#6062=DIRECTION('ref_axis',(0.923879532511287,0.,-0.38268343236509));
#6063=DIRECTION('',(0.,1.,0.));
#6064=DIRECTION('center_axis',(0.,1.,0.));
#6065=DIRECTION('ref_axis',(0.923879532511287,0.,0.38268343236509));
#6066=DIRECTION('',(0.,1.,0.));
#6067=DIRECTION('axis',(0.,0.,1.));
#6068=DIRECTION('refdir',(1.,0.,0.));
#6069=DIRECTION('center_axis',(0.952700805058341,0.,-0.303909815638107));
#6070=DIRECTION('ref_axis',(-0.303909815638107,0.,-0.952700805058341));
#6071=DIRECTION('center_axis',(-0.952700805058341,0.,0.303909815638107));
#6072=DIRECTION('ref_axis',(0.303909815638107,0.,0.952700805058341));
#6073=DIRECTION('',(0.,1.,0.));
#6074=DIRECTION('center_axis',(-0.952700805058341,0.,0.303909815638107));
#6075=DIRECTION('ref_axis',(0.303909815638107,0.,0.952700805058341));
#6076=DIRECTION('',(0.303909815638107,0.,0.952700805058341));
#6077=DIRECTION('',(0.,1.,0.));
#6078=DIRECTION('',(-0.303909815638107,0.,-0.952700805058341));
#6079=DIRECTION('center_axis',(0.,1.,0.));
#6080=DIRECTION('ref_axis',(-0.286009483054508,0.,0.958226787145346));
#6081=DIRECTION('',(0.,-1.,0.));
#6082=DIRECTION('center_axis',(0.,1.,0.));
#6083=DIRECTION('ref_axis',(-0.286009483054508,0.,0.958226787145346));
#6084=DIRECTION('center_axis',(0.,1.,0.));
#6085=DIRECTION('ref_axis',(-0.286009483054508,0.,0.958226787145346));
#6086=DIRECTION('center_axis',(0.,-1.,0.));
#6087=DIRECTION('ref_axis',(-0.286009483054508,0.,0.958226787145346));
#6088=DIRECTION('center_axis',(0.,-1.,0.));
#6089=DIRECTION('ref_axis',(-0.286009483054508,0.,0.958226787145346));
#6090=DIRECTION('center_axis',(0.286009483054514,0.,-0.958226787145345));
#6091=DIRECTION('ref_axis',(-0.677568659105072,-0.707106781186547,-0.202239244951506));
#6092=DIRECTION('',(-0.286009483054514,0.,0.958226787145345));
#6093=DIRECTION('',(0.286009483054514,0.,-0.958226787145345));
#6094=DIRECTION('center_axis',(0.,1.,0.));
#6095=DIRECTION('ref_axis',(-0.286009483054508,0.,0.958226787145346));
#6096=DIRECTION('center_axis',(0.,-1.,0.));
#6097=DIRECTION('ref_axis',(-0.286009483054508,0.,0.958226787145346));
#6098=DIRECTION('center_axis',(0.,-1.,0.));
#6099=DIRECTION('ref_axis',(-0.286009483054508,0.,0.958226787145346));
#6100=DIRECTION('center_axis',(0.,1.,0.));
#6101=DIRECTION('ref_axis',(-0.286009483054508,0.,0.958226787145346));
#6102=DIRECTION('center_axis',(0.,1.,0.));
#6103=DIRECTION('ref_axis',(-0.286009483054508,0.,0.958226787145346));
#6104=DIRECTION('center_axis',(0.,1.,0.));
#6105=DIRECTION('ref_axis',(1.,0.,0.));
#6106=DIRECTION('',(1.,0.,0.));
#6107=DIRECTION('center_axis',(0.,1.,0.));
#6108=DIRECTION('ref_axis',(1.,0.,0.));
#6109=DIRECTION('',(-1.,0.,0.));
#6110=DIRECTION('center_axis',(0.,1.,0.));
#6111=DIRECTION('ref_axis',(-1.,0.,0.));
#6112=DIRECTION('',(1.,0.,0.));
#6113=DIRECTION('',(0.,0.,1.));
#6114=DIRECTION('',(-1.,0.,0.));
#6115=DIRECTION('center_axis',(0.,0.,1.));
#6116=DIRECTION('ref_axis',(-1.,0.,0.));
#6117=DIRECTION('',(-1.,0.,0.));
#6118=DIRECTION('center_axis',(0.,0.,-1.));
#6119=DIRECTION('ref_axis',(0.,1.,0.));
#6120=DIRECTION('center_axis',(0.,-1.,0.));
#6121=DIRECTION('ref_axis',(1.,0.,0.));
#6122=DIRECTION('',(0.,0.,1.));
#6123=DIRECTION('',(1.,0.,0.));
#6124=DIRECTION('center_axis',(0.,-1.,0.));
#6125=DIRECTION('ref_axis',(1.,0.,0.));
#6126=DIRECTION('',(1.,0.,0.));
#6127=DIRECTION('',(0.,0.,1.));
#6128=DIRECTION('center_axis',(0.,0.,1.));
#6129=DIRECTION('ref_axis',(0.,1.,0.));
#6130=DIRECTION('center_axis',(0.,0.,1.));
#6131=DIRECTION('ref_axis',(0.,1.,0.));
#6132=DIRECTION('center_axis',(0.,1.,0.));
#6133=DIRECTION('ref_axis',(-1.,0.,0.));
#6134=DIRECTION('',(-1.,0.,0.));
#6135=DIRECTION('',(0.,0.,1.));
#6136=DIRECTION('center_axis',(0.,0.,1.));
#6137=DIRECTION('ref_axis',(0.,-1.,0.));
#6138=DIRECTION('center_axis',(0.,0.,1.));
#6139=DIRECTION('ref_axis',(0.,-1.,0.));
#6140=DIRECTION('center_axis',(0.,0.,-1.));
#6141=DIRECTION('ref_axis',(0.,-1.,0.));
#6142=DIRECTION('center_axis',(0.,0.,1.));
#6143=DIRECTION('ref_axis',(-1.,0.,0.));
#6144=DIRECTION('center_axis',(0.,-1.,0.));
#6145=DIRECTION('ref_axis',(1.,0.,0.));
#6146=DIRECTION('',(1.,0.,0.));
#6147=DIRECTION('',(0.,0.,1.));
#6148=DIRECTION('',(1.,0.,0.));
#6149=DIRECTION('',(0.,0.,1.));
#6150=DIRECTION('center_axis',(0.,0.,1.));
#6151=DIRECTION('ref_axis',(0.,1.,0.));
#6152=DIRECTION('center_axis',(0.,0.,1.));
#6153=DIRECTION('ref_axis',(0.,1.,0.));
#6154=DIRECTION('center_axis',(0.,0.,1.));
#6155=DIRECTION('ref_axis',(0.,1.,0.));
#6156=DIRECTION('',(0.,0.,1.));
#6157=DIRECTION('center_axis',(0.,1.,0.));
#6158=DIRECTION('ref_axis',(-1.,0.,0.));
#6159=DIRECTION('',(-1.,0.,0.));
#6160=DIRECTION('',(-1.,0.,0.));
#6161=DIRECTION('',(0.,0.,1.));
#6162=DIRECTION('center_axis',(0.,0.,1.));
#6163=DIRECTION('ref_axis',(0.,-1.,0.));
#6164=DIRECTION('center_axis',(0.,0.,1.));
#6165=DIRECTION('ref_axis',(0.,-1.,0.));
#6166=DIRECTION('center_axis',(0.,0.,1.));
#6167=DIRECTION('ref_axis',(0.,-1.,0.));
#6168=DIRECTION('center_axis',(0.,0.,1.));
#6169=DIRECTION('ref_axis',(-1.,0.,0.));
#6170=DIRECTION('center_axis',(0.,0.,1.));
#6171=DIRECTION('ref_axis',(-1.,0.,0.));
#6172=DIRECTION('',(0.,0.,1.));
#6173=DIRECTION('',(1.,0.,0.));
#6174=DIRECTION('',(0.,0.,1.));
#6175=DIRECTION('',(1.,0.,0.));
#6176=DIRECTION('',(0.,0.,1.));
#6177=DIRECTION('',(1.,0.,0.));
#6178=DIRECTION('',(0.,0.,1.));
#6179=DIRECTION('',(1.,0.,0.));
#6180=DIRECTION('',(0.,0.,1.));
#6181=DIRECTION('',(1.,0.,0.));
#6182=DIRECTION('',(0.,0.,1.));
#6183=DIRECTION('',(1.,0.,0.));
#6184=DIRECTION('',(0.,0.,1.));
#6185=DIRECTION('',(1.,0.,0.));
#6186=DIRECTION('',(0.,0.,1.));
#6187=DIRECTION('',(1.,0.,0.));
#6188=CARTESIAN_POINT('',(0.,0.,0.));
#6189=CARTESIAN_POINT('',(0.,0.,0.));
#6190=CARTESIAN_POINT('Origin',(0.,0.,0.));
#6191=CARTESIAN_POINT('',(5.,0.,-27.5499546279118));
#6192=CARTESIAN_POINT('',(-5.,-3.06161699786838E-16,-27.5499546279118));
#6193=CARTESIAN_POINT('Ctrl Pts',(5.,1.38777878078145E-16,-27.5499546279118));
#6194=CARTESIAN_POINT('Ctrl Pts',(5.,0.629275259871354,-27.5499546279118));
#6195=CARTESIAN_POINT('Ctrl Pts',(4.87396226264421,1.29954919562912,-27.5737468441049));
#6196=CARTESIAN_POINT('Ctrl Pts',(4.36328000904425,2.53103238085929,-27.6591541770631));
#6197=CARTESIAN_POINT('Ctrl Pts',(3.97870723422023,3.09236057764524,-27.7194782327905));
#6198=CARTESIAN_POINT('Ctrl Pts',(3.09237623737018,3.9786915744953,-27.832297423241));
#6199=CARTESIAN_POINT('Ctrl Pts',(2.53104134263485,4.3632766282051,-27.8921989820475));
#6200=CARTESIAN_POINT('Ctrl Pts',(1.29953505458189,4.87396779126795,-27.9766356618315));
#6201=CARTESIAN_POINT('Ctrl Pts',(0.62925302415262,5.,-28.));
#6202=CARTESIAN_POINT('Ctrl Pts',(-0.62925302415262,5.,-28.));
#6203=CARTESIAN_POINT('Ctrl Pts',(-1.29953505458189,4.87396779126795,-27.9766356618315));
#6204=CARTESIAN_POINT('Ctrl Pts',(-2.53104134263485,4.3632766282051,-27.8921989820475));
#6205=CARTESIAN_POINT('Ctrl Pts',(-3.09237623737018,3.9786915744953,-27.832297423241));
#6206=CARTESIAN_POINT('Ctrl Pts',(-3.97870723422023,3.09236057764524,-27.7194782327905));
#6207=CARTESIAN_POINT('Ctrl Pts',(-4.36328000904425,2.53103238085929,-27.6591541770631));
#6208=CARTESIAN_POINT('Ctrl Pts',(-4.87396226264421,1.29954919562912,-27.5737468441049));
#6209=CARTESIAN_POINT('Ctrl Pts',(-5.,0.629275259871354,-27.5499546279118));
#6210=CARTESIAN_POINT('Ctrl Pts',(-5.,-1.38777878078145E-16,-27.5499546279118));
#6211=CARTESIAN_POINT('Ctrl Pts',(-5.,0.,-27.5499546279118));
#6212=CARTESIAN_POINT('Ctrl Pts',(-5.,-0.629275259871354,-27.5499546279118));
#6213=CARTESIAN_POINT('Ctrl Pts',(-4.87396226264421,-1.29954919562912,-27.5737468441049));
#6214=CARTESIAN_POINT('Ctrl Pts',(-4.36328000904425,-2.53103238085929,-27.6591541770631));
#6215=CARTESIAN_POINT('Ctrl Pts',(-3.97870723422023,-3.09236057764524,-27.7194782327905));
#6216=CARTESIAN_POINT('Ctrl Pts',(-3.09237623737018,-3.9786915744953,-27.832297423241));
#6217=CARTESIAN_POINT('Ctrl Pts',(-2.53104134263485,-4.3632766282051,-27.8921989820475));
#6218=CARTESIAN_POINT('Ctrl Pts',(-1.29953505458189,-4.87396779126795,-27.9766356618315));
#6219=CARTESIAN_POINT('Ctrl Pts',(-0.629253024152621,-5.,-28.));
#6220=CARTESIAN_POINT('Ctrl Pts',(0.629253024152618,-5.,-28.));
#6221=CARTESIAN_POINT('Ctrl Pts',(1.29953505458189,-4.87396779126795,-27.9766356618315));
#6222=CARTESIAN_POINT('Ctrl Pts',(2.53104134263485,-4.3632766282051,-27.8921989820475));
#6223=CARTESIAN_POINT('Ctrl Pts',(3.09237623737018,-3.9786915744953,-27.832297423241));
#6224=CARTESIAN_POINT('Ctrl Pts',(3.97870723422023,-3.09236057764525,-27.7194782327905));
#6225=CARTESIAN_POINT('Ctrl Pts',(4.36328000904425,-2.5310323808593,-27.6591541770631));
#6226=CARTESIAN_POINT('Ctrl Pts',(4.87396226264421,-1.29954919562912,-27.5737468441049));
#6227=CARTESIAN_POINT('Ctrl Pts',(5.,-0.629275259871355,-27.5499546279118));
#6228=CARTESIAN_POINT('Ctrl Pts',(5.,0.,-27.5499546279118));
#6229=CARTESIAN_POINT('',(-5.,-6.12323399573677E-16,-24.4948974278318));
#6230=CARTESIAN_POINT('',(-5.,-6.12323399573677E-16,0.));
#6231=CARTESIAN_POINT('',(5.,1.38777878078145E-16,-24.4948974278318));
#6232=CARTESIAN_POINT('Ctrl Pts',(5.,0.,-24.4948974278318));
#6233=CARTESIAN_POINT('Ctrl Pts',(5.,-0.62965875981699,-24.4948974278318));
#6234=CARTESIAN_POINT('Ctrl Pts',(4.87381398124307,-1.30008888580946,-24.5216938309223));
#6235=CARTESIAN_POINT('Ctrl Pts',(4.36302708824191,-2.53146002515027,-24.6177075396385));
#6236=CARTESIAN_POINT('Ctrl Pts',(3.97851551096044,-3.09255230090503,-24.6854542550966));
#6237=CARTESIAN_POINT('Ctrl Pts',(3.09257712322547,-3.97849068864001,-24.8120168819159));
#6238=CARTESIAN_POINT('Ctrl Pts',(2.53147430598813,-4.36302170772379,-24.8791673575932));
#6239=CARTESIAN_POINT('Ctrl Pts',(1.30006653040932,-4.87382271117917,-24.9738094323541));
#6240=CARTESIAN_POINT('Ctrl Pts',(0.629623477106996,-5.,-25.));
#6241=CARTESIAN_POINT('Ctrl Pts',(-0.629623477106999,-5.,-25.));
#6242=CARTESIAN_POINT('Ctrl Pts',(-1.30006653040933,-4.87382271117917,-24.9738094323541));
#6243=CARTESIAN_POINT('Ctrl Pts',(-2.53147430598813,-4.36302170772379,-24.8791673575932));
#6244=CARTESIAN_POINT('Ctrl Pts',(-3.09257712322547,-3.97849068864001,-24.8120168819159));
#6245=CARTESIAN_POINT('Ctrl Pts',(-3.97851551096044,-3.09255230090503,-24.6854542550966));
#6246=CARTESIAN_POINT('Ctrl Pts',(-4.36302708824191,-2.53146002515027,-24.6177075396385));
#6247=CARTESIAN_POINT('Ctrl Pts',(-4.87381398124307,-1.30008888580945,-24.5216938309223));
#6248=CARTESIAN_POINT('Ctrl Pts',(-5.,-0.62965875981699,-24.4948974278318));
#6249=CARTESIAN_POINT('Ctrl Pts',(-5.,4.16333634234434E-16,-24.4948974278318));
#6250=CARTESIAN_POINT('Ctrl Pts',(-5.,1.38777878078145E-16,-24.4948974278318));
#6251=CARTESIAN_POINT('Ctrl Pts',(-5.,0.62965875981699,-24.4948974278318));
#6252=CARTESIAN_POINT('Ctrl Pts',(-4.87381398124307,1.30008888580945,-24.5216938309223));
#6253=CARTESIAN_POINT('Ctrl Pts',(-4.36302708824191,2.53146002515027,-24.6177075396385));
#6254=CARTESIAN_POINT('Ctrl Pts',(-3.97851551096044,3.09255230090503,-24.6854542550966));
#6255=CARTESIAN_POINT('Ctrl Pts',(-3.09257712322547,3.97849068864001,-24.8120168819159));
#6256=CARTESIAN_POINT('Ctrl Pts',(-2.53147430598813,4.36302170772379,-24.8791673575932));
#6257=CARTESIAN_POINT('Ctrl Pts',(-1.30006653040932,4.87382271117917,-24.9738094323541));
#6258=CARTESIAN_POINT('Ctrl Pts',(-0.629623477106998,5.,-25.));
#6259=CARTESIAN_POINT('Ctrl Pts',(0.629623477106998,5.,-25.));
#6260=CARTESIAN_POINT('Ctrl Pts',(1.30006653040932,4.87382271117917,-24.9738094323541));
#6261=CARTESIAN_POINT('Ctrl Pts',(2.53147430598813,4.36302170772379,-24.8791673575932));
#6262=CARTESIAN_POINT('Ctrl Pts',(3.09257712322547,3.97849068864001,-24.8120168819159));
#6263=CARTESIAN_POINT('Ctrl Pts',(3.97851551096044,3.09255230090503,-24.6854542550966));
#6264=CARTESIAN_POINT('Ctrl Pts',(4.36302708824191,2.53146002515027,-24.6177075396385));
#6265=CARTESIAN_POINT('Ctrl Pts',(4.87381398124307,1.30008888580945,-24.5216938309223));
#6266=CARTESIAN_POINT('Ctrl Pts',(5.,0.62965875981699,-24.4948974278318));
#6267=CARTESIAN_POINT('Ctrl Pts',(5.,-2.77555756156289E-16,-24.4948974278318));
#6268=CARTESIAN_POINT('Origin',(0.,0.,0.));
#6269=CARTESIAN_POINT('',(5.,1.38777878078145E-16,24.4948974278318));
#6270=CARTESIAN_POINT('',(-5.,-6.12323399573677E-16,24.4948974278318));
#6271=CARTESIAN_POINT('Ctrl Pts',(5.,0.,24.4948974278318));
#6272=CARTESIAN_POINT('Ctrl Pts',(5.,0.62965875981699,24.4948974278318));
#6273=CARTESIAN_POINT('Ctrl Pts',(4.87381398124307,1.30008888580945,24.5216938309223));
#6274=CARTESIAN_POINT('Ctrl Pts',(4.36302708824191,2.53146002515027,24.6177075396385));
#6275=CARTESIAN_POINT('Ctrl Pts',(3.97851551096044,3.09255230090503,24.6854542550966));
#6276=CARTESIAN_POINT('Ctrl Pts',(3.09257712322547,3.97849068864001,24.8120168819159));
#6277=CARTESIAN_POINT('Ctrl Pts',(2.53147430598813,4.36302170772379,24.8791673575932));
#6278=CARTESIAN_POINT('Ctrl Pts',(1.30006653040932,4.87382271117917,24.9738094323541));
#6279=CARTESIAN_POINT('Ctrl Pts',(0.629623477106997,5.,25.));
#6280=CARTESIAN_POINT('Ctrl Pts',(-0.629623477106997,5.,25.));
#6281=CARTESIAN_POINT('Ctrl Pts',(-1.30006653040932,4.87382271117917,24.9738094323541));
#6282=CARTESIAN_POINT('Ctrl Pts',(-2.53147430598813,4.36302170772379,24.8791673575932));
#6283=CARTESIAN_POINT('Ctrl Pts',(-3.09257712322547,3.97849068864001,24.8120168819159));
#6284=CARTESIAN_POINT('Ctrl Pts',(-3.97851551096044,3.09255230090503,24.6854542550966));
#6285=CARTESIAN_POINT('Ctrl Pts',(-4.36302708824191,2.53146002515027,24.6177075396385));
#6286=CARTESIAN_POINT('Ctrl Pts',(-4.87381398124307,1.30008888580945,24.5216938309223));
#6287=CARTESIAN_POINT('Ctrl Pts',(-5.,0.62965875981699,24.4948974278318));
#6288=CARTESIAN_POINT('Ctrl Pts',(-5.,0.,24.4948974278318));
#6289=CARTESIAN_POINT('Ctrl Pts',(-5.,1.38777878078145E-16,24.4948974278318));
#6290=CARTESIAN_POINT('Ctrl Pts',(-5.,-0.62965875981699,24.4948974278318));
#6291=CARTESIAN_POINT('Ctrl Pts',(-4.87381398124307,-1.30008888580945,24.5216938309223));
#6292=CARTESIAN_POINT('Ctrl Pts',(-4.36302708824191,-2.53146002515027,24.6177075396385));
#6293=CARTESIAN_POINT('Ctrl Pts',(-3.97851551096044,-3.09255230090503,24.6854542550966));
#6294=CARTESIAN_POINT('Ctrl Pts',(-3.09257712322547,-3.97849068864001,24.8120168819159));
#6295=CARTESIAN_POINT('Ctrl Pts',(-2.53147430598813,-4.36302170772379,24.8791673575932));
#6296=CARTESIAN_POINT('Ctrl Pts',(-1.30006653040932,-4.87382271117917,24.9738094323541));
#6297=CARTESIAN_POINT('Ctrl Pts',(-0.629623477106999,-5.,25.));
#6298=CARTESIAN_POINT('Ctrl Pts',(0.629623477106997,-5.,25.));
#6299=CARTESIAN_POINT('Ctrl Pts',(1.30006653040932,-4.87382271117917,24.9738094323541));
#6300=CARTESIAN_POINT('Ctrl Pts',(2.53147430598813,-4.36302170772379,24.8791673575932));
#6301=CARTESIAN_POINT('Ctrl Pts',(3.09257712322547,-3.97849068864001,24.8120168819159));
#6302=CARTESIAN_POINT('Ctrl Pts',(3.97851551096044,-3.09255230090503,24.6854542550966));
#6303=CARTESIAN_POINT('Ctrl Pts',(4.36302708824191,-2.53146002515027,24.6177075396385));
#6304=CARTESIAN_POINT('Ctrl Pts',(4.87381398124307,-1.30008888580946,24.5216938309223));
#6305=CARTESIAN_POINT('Ctrl Pts',(5.,-0.62965875981699,24.4948974278318));
#6306=CARTESIAN_POINT('Ctrl Pts',(5.,0.,24.4948974278318));
#6307=CARTESIAN_POINT('',(-5.,-1.67383821708694E-16,27.5499546279118));
#6308=CARTESIAN_POINT('',(-5.,-6.12323399573677E-16,0.));
#6309=CARTESIAN_POINT('',(5.,0.,27.5499546279118));
#6310=CARTESIAN_POINT('Ctrl Pts',(5.,1.38777878078145E-16,27.5499546279118));
#6311=CARTESIAN_POINT('Ctrl Pts',(5.,-0.629275259871354,27.5499546279118));
#6312=CARTESIAN_POINT('Ctrl Pts',(4.87396226264421,-1.29954919562912,27.5737468441049));
#6313=CARTESIAN_POINT('Ctrl Pts',(4.36328000904425,-2.53103238085929,27.6591541770631));
#6314=CARTESIAN_POINT('Ctrl Pts',(3.97870723422023,-3.09236057764524,27.7194782327905));
#6315=CARTESIAN_POINT('Ctrl Pts',(3.09237623737018,-3.9786915744953,27.832297423241));
#6316=CARTESIAN_POINT('Ctrl Pts',(2.53104134263485,-4.3632766282051,27.8921989820475));
#6317=CARTESIAN_POINT('Ctrl Pts',(1.29953505458189,-4.87396779126795,27.9766356618315));
#6318=CARTESIAN_POINT('Ctrl Pts',(0.629253024152619,-5.,28.));
#6319=CARTESIAN_POINT('Ctrl Pts',(-0.629253024152621,-5.,28.));
#6320=CARTESIAN_POINT('Ctrl Pts',(-1.29953505458189,-4.87396779126795,27.9766356618315));
#6321=CARTESIAN_POINT('Ctrl Pts',(-2.53104134263485,-4.3632766282051,27.8921989820475));
#6322=CARTESIAN_POINT('Ctrl Pts',(-3.09237623737018,-3.9786915744953,27.832297423241));
#6323=CARTESIAN_POINT('Ctrl Pts',(-3.97870723422023,-3.09236057764524,27.7194782327905));
#6324=CARTESIAN_POINT('Ctrl Pts',(-4.36328000904426,-2.53103238085929,27.6591541770631));
#6325=CARTESIAN_POINT('Ctrl Pts',(-4.87396226264421,-1.29954919562912,27.5737468441049));
#6326=CARTESIAN_POINT('Ctrl Pts',(-5.,-0.629275259871353,27.5499546279118));
#6327=CARTESIAN_POINT('Ctrl Pts',(-5.,-1.38777878078145E-16,27.5499546279118));
#6328=CARTESIAN_POINT('Ctrl Pts',(-5.,2.77555756156289E-16,27.5499546279118));
#6329=CARTESIAN_POINT('Ctrl Pts',(-5.,0.629275259871354,27.5499546279118));
#6330=CARTESIAN_POINT('Ctrl Pts',(-4.87396226264421,1.29954919562912,27.5737468441049));
#6331=CARTESIAN_POINT('Ctrl Pts',(-4.36328000904425,2.53103238085929,27.6591541770631));
#6332=CARTESIAN_POINT('Ctrl Pts',(-3.97870723422023,3.09236057764524,27.7194782327905));
#6333=CARTESIAN_POINT('Ctrl Pts',(-3.09237623737018,3.9786915744953,27.832297423241));
#6334=CARTESIAN_POINT('Ctrl Pts',(-2.53104134263485,4.3632766282051,27.8921989820475));
#6335=CARTESIAN_POINT('Ctrl Pts',(-1.29953505458189,4.87396779126795,27.9766356618315));
#6336=CARTESIAN_POINT('Ctrl Pts',(-0.629253024152619,5.,28.));
#6337=CARTESIAN_POINT('Ctrl Pts',(0.629253024152621,5.,28.));
#6338=CARTESIAN_POINT('Ctrl Pts',(1.29953505458189,4.87396779126795,27.9766356618315));
#6339=CARTESIAN_POINT('Ctrl Pts',(2.53104134263485,4.3632766282051,27.8921989820475));
#6340=CARTESIAN_POINT('Ctrl Pts',(3.09237623737018,3.9786915744953,27.832297423241));
#6341=CARTESIAN_POINT('Ctrl Pts',(3.97870723422023,3.09236057764524,27.7194782327905));
#6342=CARTESIAN_POINT('Ctrl Pts',(4.36328000904425,2.53103238085929,27.6591541770631));
#6343=CARTESIAN_POINT('Ctrl Pts',(4.87396226264421,1.29954919562912,27.5737468441049));
#6344=CARTESIAN_POINT('Ctrl Pts',(5.,0.629275259871354,27.5499546279118));
#6345=CARTESIAN_POINT('Ctrl Pts',(5.,2.77555756156289E-16,27.5499546279118));
#6346=CARTESIAN_POINT('Origin',(0.,5.5,0.));
#6347=CARTESIAN_POINT('',(-3.12284933782575E-15,6.,25.5));
#6348=CARTESIAN_POINT('Origin',(0.,6.,0.));
#6349=CARTESIAN_POINT('',(-3.06161699786838E-15,5.5,25.));
#6350=CARTESIAN_POINT('Origin',(-3.12284933782575E-15,5.5,25.5));
#6351=CARTESIAN_POINT('',(-25.,5.5,-3.06161699786838E-15));
#6352=CARTESIAN_POINT('Origin',(0.,5.5,0.));
#6353=CARTESIAN_POINT('Origin',(0.,5.5,0.));
#6354=CARTESIAN_POINT('Origin',(0.,6.,0.));
#6355=CARTESIAN_POINT('',(-3.36777869765522E-15,6.,-27.5));
#6356=CARTESIAN_POINT('Origin',(0.,6.,0.));
#6357=CARTESIAN_POINT('Origin',(0.,0.,0.));
#6358=CARTESIAN_POINT('',(-3.06161699786838E-15,-5.5,-25.));
#6359=CARTESIAN_POINT('',(-25.,-5.5,3.06161699786838E-15));
#6360=CARTESIAN_POINT('Origin',(0.,-5.5,0.));
#6361=CARTESIAN_POINT('Origin',(0.,-5.5,0.));
#6362=CARTESIAN_POINT('',(-25.,0.,3.06161699786838E-15));
#6363=CARTESIAN_POINT('Origin',(0.,5.5,0.));
#6364=CARTESIAN_POINT('',(-3.42901103761259E-15,5.5,-28.));
#6365=CARTESIAN_POINT('Origin',(-3.36777869765522E-15,5.5,-27.5));
#6366=CARTESIAN_POINT('',(-28.,5.5,3.42901103761259E-15));
#6367=CARTESIAN_POINT('Origin',(0.,5.5,0.));
#6368=CARTESIAN_POINT('Origin',(0.,5.5,0.));
#6369=CARTESIAN_POINT('Origin',(0.,0.,0.));
#6370=CARTESIAN_POINT('',(-28.,-5.5,3.42901103761259E-15));
#6371=CARTESIAN_POINT('',(-28.,0.,3.42901103761259E-15));
#6372=CARTESIAN_POINT('',(-3.42901103761259E-15,-5.5,28.));
#6373=CARTESIAN_POINT('Origin',(0.,-5.5,0.));
#6374=CARTESIAN_POINT('Origin',(0.,-5.5,0.));
#6375=CARTESIAN_POINT('Origin',(0.,-5.5,0.));
#6376=CARTESIAN_POINT('',(-3.36777869765522E-15,-6.,27.5));
#6377=CARTESIAN_POINT('Origin',(0.,-6.,0.));
#6378=CARTESIAN_POINT('Origin',(-3.36777869765522E-15,-5.5,27.5));
#6379=CARTESIAN_POINT('Origin',(0.,-6.,0.));
#6380=CARTESIAN_POINT('',(-3.12284933782575E-15,-6.,-25.5));
#6381=CARTESIAN_POINT('Origin',(0.,-6.,0.));
#6382=CARTESIAN_POINT('Origin',(0.,-5.5,0.));
#6383=CARTESIAN_POINT('Origin',(-3.12284933782575E-15,-5.5,-25.5));
#6384=CARTESIAN_POINT('',(0.,0.,0.));
#6385=CARTESIAN_POINT('Origin',(-0.5,0.,0.));
#6386=CARTESIAN_POINT('',(0.500000000000005,-24.5,3.00038465791102E-15));
#6387=CARTESIAN_POINT('Origin',(0.5,2.22044604925031E-16,0.));
#6388=CARTESIAN_POINT('',(-0.499999999999995,-24.5,3.00038465791102E-15));
#6389=CARTESIAN_POINT('',(-0.499999999999995,-24.5,-3.00038465791102E-15));
#6390=CARTESIAN_POINT('Origin',(-0.5,0.,0.));
#6391=CARTESIAN_POINT('Origin',(-0.5,0.,0.));
#6392=CARTESIAN_POINT('Origin',(0.5,2.22044604925031E-16,0.));
#6393=CARTESIAN_POINT('',(0.,0.,0.));
#6394=CARTESIAN_POINT('Origin',(0.,0.,60.));
#6395=CARTESIAN_POINT('',(4.,4.89858719658941E-16,60.));
#6396=CARTESIAN_POINT('Origin',(0.,0.,60.));
#6397=CARTESIAN_POINT('',(4.,4.89858719658941E-16,60.2));
#6398=CARTESIAN_POINT('',(4.,4.89858719658941E-16,60.));
#6399=CARTESIAN_POINT('Origin',(0.,0.,60.2));
#6400=CARTESIAN_POINT('Origin',(0.,0.,60.));
#6401=CARTESIAN_POINT('',(10.,-1.22464679914735E-15,60.2));
#6402=CARTESIAN_POINT('Origin',(0.,0.,60.2));
#6403=CARTESIAN_POINT('',(10.,-1.22464679914735E-15,60.));
#6404=CARTESIAN_POINT('',(10.,1.22464679914735E-15,60.));
#6405=CARTESIAN_POINT('Origin',(0.,0.,60.));
#6406=CARTESIAN_POINT('Origin',(0.,0.,60.2));
#6407=CARTESIAN_POINT('Origin',(0.,0.,60.));
#6408=CARTESIAN_POINT('',(0.,0.,0.));
#6409=CARTESIAN_POINT('Origin',(0.,0.,46.4896150285955));
#6410=CARTESIAN_POINT('',(-2.31338095599003,-3.36682247118298,59.7031574977731));
#6411=CARTESIAN_POINT('',(-2.31666171942419,-3.37161025274083,59.8073433279728));
#6412=CARTESIAN_POINT('',(-2.31338095599002,-3.36682247118298,46.4896150285955));
#6413=CARTESIAN_POINT('',(1.46332546897508,-3.81390922438499,60.));
#6414=CARTESIAN_POINT('Ctrl Pts',(-2.31666171942481,-3.3716102527404,59.8073433279728));
#6415=CARTESIAN_POINT('Ctrl Pts',(-1.23546730076796,-4.11246432174188,59.8715622186486));
#6416=CARTESIAN_POINT('Ctrl Pts',(0.232198041727834,-4.28626973793002,59.9357811093243));
#6417=CARTESIAN_POINT('Ctrl Pts',(1.46332546897508,-3.81390922438499,60.));
#6418=CARTESIAN_POINT('',(3.17563310416156,-2.56954847935454,59.9999997913602));
#6419=CARTESIAN_POINT('Origin',(0.,0.,60.));
#6420=CARTESIAN_POINT('Ctrl Pts',(-2.31338095599003,-3.36682247118298,59.7031574977731));
#6421=CARTESIAN_POINT('Ctrl Pts',(-2.21469513777677,-3.43463058831267,59.7089734558387));
#6422=CARTESIAN_POINT('Ctrl Pts',(-2.11300662318653,-3.49810921792803,59.7147894139042));
#6423=CARTESIAN_POINT('Ctrl Pts',(-2.0087347754621,-3.5569944618806,59.7206053719698));
#6424=CARTESIAN_POINT('Ctrl Pts',(-1.90445636797313,-3.61588341031662,59.7264216959185));
#6425=CARTESIAN_POINT('Ctrl Pts',(-1.79759465807523,-3.67017819886025,59.7322380198673));
#6426=CARTESIAN_POINT('Ctrl Pts',(-1.68859434101989,-3.71966048873759,59.738054343816));
#6427=CARTESIAN_POINT('Ctrl Pts',(-1.57956176687172,-3.76915742219453,59.743872389023));
#6428=CARTESIAN_POINT('Ctrl Pts',(-1.46838969662447,-3.81383885657602,59.7496904342301));
#6429=CARTESIAN_POINT('Ctrl Pts',(-1.35554298540466,-3.85353450934596,59.7555084794371));
#6430=CARTESIAN_POINT('Ctrl Pts',(-1.24257680898892,-3.89327218592754,59.761332683919));
#6431=CARTESIAN_POINT('Ctrl Pts',(-1.1279328361525,-3.92801340962138,59.7671568884009));
#6432=CARTESIAN_POINT('Ctrl Pts',(-1.01209142685303,-3.95763767210827,59.7729810928828));
#6433=CARTESIAN_POINT('Ctrl Pts',(-0.896177332833092,-3.98728052234588,
59.7788089517633));
#6434=CARTESIAN_POINT('Ctrl Pts',(-0.779064702686944,-4.01179993297524,
59.7846368106437));
#6435=CARTESIAN_POINT('Ctrl Pts',(-0.66124285712451,-4.03112675115802,59.7904646695241));
#6436=CARTESIAN_POINT('Ctrl Pts',(-0.543257750327005,-4.05048034977521,
59.7963006038462));
#6437=CARTESIAN_POINT('Ctrl Pts',(-0.424561868666963,-4.06462694542446,
59.8021365381682));
#6438=CARTESIAN_POINT('Ctrl Pts',(-0.305648550467959,-4.0735493078637,59.8079724724903));
#6439=CARTESIAN_POINT('Ctrl Pts',(-0.27391858731232,-4.07593008602838,59.8095296906709));
#6440=CARTESIAN_POINT('Ctrl Pts',(-0.242173134744564,-4.07793918777959,
59.8110869088515));
#6441=CARTESIAN_POINT('Ctrl Pts',(-0.210421531939963,-4.07957691175152,
59.8126441270322));
#6442=CARTESIAN_POINT('Ctrl Pts',(-0.0923883607714591,-4.08566497461545,
59.8184329182687));
#6443=CARTESIAN_POINT('Ctrl Pts',(0.0261069165980141,-4.086636406536,59.8242217095052));
#6444=CARTESIAN_POINT('Ctrl Pts',(0.144580903785145,-4.08244061343955,59.8300105007417));
#6445=CARTESIAN_POINT('Ctrl Pts',(0.262908175693732,-4.07825001631031,59.8357921232812));
#6446=CARTESIAN_POINT('Ctrl Pts',(0.381213800033834,-4.06890493319291,59.8415737458207));
#6447=CARTESIAN_POINT('Ctrl Pts',(0.499010729166501,-4.05440665106212,59.8473553683602));
#6448=CARTESIAN_POINT('Ctrl Pts',(0.61669345438166,-4.03992242499058,59.8531313856267));
#6449=CARTESIAN_POINT('Ctrl Pts',(0.733868056967211,-4.02029498706776,59.8589074028932));
#6450=CARTESIAN_POINT('Ctrl Pts',(0.850049640732392,-3.9955776313683,59.8646834201597));
#6451=CARTESIAN_POINT('Ctrl Pts',(0.966153102927478,-3.97087689584714,59.8704555535788));
#6452=CARTESIAN_POINT('Ctrl Pts',(1.08126447101308,-3.94109313594346,59.876227686998));
#6453=CARTESIAN_POINT('Ctrl Pts',(1.19490673987542,-3.90633112818157,59.8819998204171));
#6454=CARTESIAN_POINT('Ctrl Pts',(1.30850926666104,-3.87158127711449,59.8877699352514));
#6455=CARTESIAN_POINT('Ctrl Pts',(1.42064332039576,-3.83185675992719,59.8935400500856));
#6456=CARTESIAN_POINT('Ctrl Pts',(1.53084539717501,-3.7873126844701,59.8993101649198));
#6457=CARTESIAN_POINT('Ctrl Pts',(1.64103575391707,-3.74277334629415,59.9050796660999));
#6458=CARTESIAN_POINT('Ctrl Pts',(1.74929415882466,-3.69341562428457,59.91084916728));
#6459=CARTESIAN_POINT('Ctrl Pts',(1.8551761647154,-3.63944314392626,59.9166186684601));
#6460=CARTESIAN_POINT('Ctrl Pts',(1.96107267801672,-3.5854632685349,59.9223889601478));
#6461=CARTESIAN_POINT('Ctrl Pts',(2.06459177664333,-3.52686756612609,59.9281592518354));
#6462=CARTESIAN_POINT('Ctrl Pts',(2.16531338027168,-3.46390573850046,59.933929543523));
#6463=CARTESIAN_POINT('Ctrl Pts',(2.2661332664976,-3.40088247368814,59.9397054657729));
#6464=CARTESIAN_POINT('Ctrl Pts',(2.36414985453216,-3.33348479456704,59.9454813880227));
#6465=CARTESIAN_POINT('Ctrl Pts',(2.45897173564387,-3.2620059784287,59.9512573102726));
#6466=CARTESIAN_POINT('Ctrl Pts',(2.55384135103432,-3.19049117914286,59.9570361401791));
#6467=CARTESIAN_POINT('Ctrl Pts',(2.64551273705809,-3.11489141383132,59.9628149700857));
#6468=CARTESIAN_POINT('Ctrl Pts',(2.73362866411939,-3.03553937986395,59.9685937999923));
#6469=CARTESIAN_POINT('Ctrl Pts',(2.82188055805937,-2.95606490210311,59.974381546896));
#6470=CARTESIAN_POINT('Ctrl Pts',(2.90656573841288,-2.87282687955783,59.9801692937997));
#6471=CARTESIAN_POINT('Ctrl Pts',(2.987364550522,-2.78619418603307,59.9859570407034));
#6472=CARTESIAN_POINT('Ctrl Pts',(3.05271165885833,-2.71612884891419,59.990637957589));
#6473=CARTESIAN_POINT('Ctrl Pts',(3.11551739932373,-2.64384379773319,59.9953188744746));
#6474=CARTESIAN_POINT('Ctrl Pts',(3.17563310416156,-2.56954847935454,59.9999997913602));
#6475=CARTESIAN_POINT('Origin',(0.,0.,46.4896150285955));
#6476=CARTESIAN_POINT('',(-2.31338095599002,-3.36682247118298,58.4531830718678));
#6477=CARTESIAN_POINT('',(-2.31338095599002,-3.36682247118299,58.5572666440642));
#6478=CARTESIAN_POINT('',(-2.31338095599002,-3.36682247118298,46.4896150285955));
#6479=CARTESIAN_POINT('',(-4.08799668051687,0.000978769805548399,59.6146155644207));
#6480=CARTESIAN_POINT('Ctrl Pts',(-2.31338095599002,-3.36682247118299,58.5572666440642));
#6481=CARTESIAN_POINT('Ctrl Pts',(-2.21480203430358,-3.43455713852685,58.5630789515449));
#6482=CARTESIAN_POINT('Ctrl Pts',(-2.11329234559576,-3.49792673610757,58.5688912590256));
#6483=CARTESIAN_POINT('Ctrl Pts',(-2.00928105362083,-3.55668590791489,58.5747035665063));
#6484=CARTESIAN_POINT('Ctrl Pts',(-1.90521720845016,-3.61547476863578,58.5805188107387));
#6485=CARTESIAN_POINT('Ctrl Pts',(-1.79864960515187,-3.66964837696318,58.586334054971));
#6486=CARTESIAN_POINT('Ctrl Pts',(-1.69003007411857,-3.71900838242868,58.5921492992033));
#6487=CARTESIAN_POINT('Ctrl Pts',(-1.58123532526954,-3.76844801217777,58.5979739242016));
#6488=CARTESIAN_POINT('Ctrl Pts',(-1.4703824130478,-3.81305836949707,58.6037985491998));
#6489=CARTESIAN_POINT('Ctrl Pts',(-1.35794170423633,-3.85268988213375,58.6096231741981));
#6490=CARTESIAN_POINT('Ctrl Pts',(-1.25108141854553,-3.89035448606127,58.6151587235372));
#6491=CARTESIAN_POINT('Ctrl Pts',(-1.14278744447073,-3.92352250021008,58.6206942728764));
#6492=CARTESIAN_POINT('Ctrl Pts',(-1.03347228199655,-3.95210830346852,58.6262298222155));
#6493=CARTESIAN_POINT('Ctrl Pts',(-0.918388533385041,-3.98220258610594,
58.6320574837599));
#6494=CARTESIAN_POINT('Ctrl Pts',(-0.80180629177334,-4.00731374478515,58.6378851453043));
#6495=CARTESIAN_POINT('Ctrl Pts',(-0.684194478847014,-4.02729473904199,
58.6437128068487));
#6496=CARTESIAN_POINT('Ctrl Pts',(-0.566729849994398,-4.04725072829245,
58.649533175427));
#6497=CARTESIAN_POINT('Ctrl Pts',(-0.448238611066349,-4.06208925536335,
58.6553535440054));
#6498=CARTESIAN_POINT('Ctrl Pts',(-0.329203545658992,-4.0717134016929,58.6611739125836));
#6499=CARTESIAN_POINT('Ctrl Pts',(-0.210286549509897,-4.08132800196293,
58.6669885080177));
#6500=CARTESIAN_POINT('Ctrl Pts',(-0.0908272040805449,-4.08573847844648,
58.6728031034518));
#6501=CARTESIAN_POINT('Ctrl Pts',(0.028683427381987,-4.08489929630996,58.6786176988859));
#6502=CARTESIAN_POINT('Ctrl Pts',(0.15188917382253,-4.08403416774137,58.6846120741305));
#6503=CARTESIAN_POINT('Ctrl Pts',(0.275148994387207,-4.07758940390421,58.6906064493751));
#6504=CARTESIAN_POINT('Ctrl Pts',(0.39792082571284,-4.06557302436742,58.6966008246197));
#6505=CARTESIAN_POINT('Ctrl Pts',(0.516878449304106,-4.05392996310137,58.7024089699109));
#6506=CARTESIAN_POINT('Ctrl Pts',(0.635377520845544,-4.03705639683912,58.7082171152021));
#6507=CARTESIAN_POINT('Ctrl Pts',(0.752927554220468,-4.01501246549691,58.7140252604934));
#6508=CARTESIAN_POINT('Ctrl Pts',(0.870460595530278,-3.99297172064395,58.7198325662069));
#6509=CARTESIAN_POINT('Ctrl Pts',(0.987044470944633,-3.96576217225358,58.7256398719205));
#6510=CARTESIAN_POINT('Ctrl Pts',(1.10219760709635,-3.93349532031132,58.7314471776341));
#6511=CARTESIAN_POINT('Ctrl Pts',(1.21736116147698,-3.90122554909599,58.737255008751));
#6512=CARTESIAN_POINT('Ctrl Pts',(1.33109332668071,-3.86389767461634,58.7430628398679));
#6513=CARTESIAN_POINT('Ctrl Pts',(1.44292705635254,-3.82167326050328,58.7488706709848));
#6514=CARTESIAN_POINT('Ctrl Pts',(1.55479718736688,-3.77943510254599,58.7546803925229));
#6515=CARTESIAN_POINT('Ctrl Pts',(1.66476727271772,-3.73229737908953,58.7604901140609));
#6516=CARTESIAN_POINT('Ctrl Pts',(1.77239022362783,-3.68046979272871,58.766299835599));
#6517=CARTESIAN_POINT('Ctrl Pts',(1.88013104605108,-3.62858544341932,58.7721159200983));
#6518=CARTESIAN_POINT('Ctrl Pts',(1.98551923548309,-3.57200115566269,58.7779320045977));
#6519=CARTESIAN_POINT('Ctrl Pts',(2.08813216743317,-3.51097266456617,58.783748089097));
#6520=CARTESIAN_POINT('Ctrl Pts',(2.19081247945898,-3.44990409953088,58.7895679926882));
#6521=CARTESIAN_POINT('Ctrl Pts',(2.29071356451001,-3.38438574219185,58.7953878962794));
#6522=CARTESIAN_POINT('Ctrl Pts',(2.3874430131871,-3.3147158036224,58.8012077998706));
#6523=CARTESIAN_POINT('Ctrl Pts',(2.48430817974334,-3.24494811347438,58.8070358691754));
#6524=CARTESIAN_POINT('Ctrl Pts',(2.57799250963747,-3.1710174681164,58.8128639384801));
#6525=CARTESIAN_POINT('Ctrl Pts',(2.66813771436471,-3.0932614078323,58.8186920077849));
#6526=CARTESIAN_POINT('Ctrl Pts',(2.68768181703163,-3.07640335720425,58.819955573442));
#6527=CARTESIAN_POINT('Ctrl Pts',(2.70705970490966,-3.0593656245969,58.8212191390991));
#6528=CARTESIAN_POINT('Ctrl Pts',(2.7262679680436,-3.04215186445703,58.8224827047561));
#6529=CARTESIAN_POINT('Ctrl Pts',(2.81485875306806,-2.9627599635142,58.8283104192511));
#6530=CARTESIAN_POINT('Ctrl Pts',(2.90011916689984,-2.87936917863925,58.8341381337461));
#6531=CARTESIAN_POINT('Ctrl Pts',(2.9816679295944,-2.79228962638697,58.8399658482411));
#6532=CARTESIAN_POINT('Ctrl Pts',(3.06311488129128,-2.70531879014458,58.8457862870227));
#6533=CARTESIAN_POINT('Ctrl Pts',(3.14085912268164,-2.61466864175858,58.8516067258043));
#6534=CARTESIAN_POINT('Ctrl Pts',(3.21455354374732,-2.52068850006928,58.8574271645859));
#6535=CARTESIAN_POINT('Ctrl Pts',(3.288175083505,-2.42680130158455,58.863241847149));
#6536=CARTESIAN_POINT('Ctrl Pts',(3.35775452088454,-2.32959098058406,58.869056529712));
#6537=CARTESIAN_POINT('Ctrl Pts',(3.42298304622498,-2.22944209730963,58.8748712122751));
#6538=CARTESIAN_POINT('Ctrl Pts',(3.49022705116358,-2.1261987391875,58.8808655612344));
#6539=CARTESIAN_POINT('Ctrl Pts',(3.55284659891326,-2.01983259477798,58.8868599101936));
#6540=CARTESIAN_POINT('Ctrl Pts',(3.61054944869451,-1.91080027175312,58.8928542591528));
#6541=CARTESIAN_POINT('Ctrl Pts',(3.66646109651549,-1.80515251138807,58.8986625325604));
#6542=CARTESIAN_POINT('Ctrl Pts',(3.71775657481677,-1.69700203731464,58.904470805968));
#6543=CARTESIAN_POINT('Ctrl Pts',(3.76421554653954,-1.58679120214037,58.9102790793755));
#6544=CARTESIAN_POINT('Ctrl Pts',(3.81066792155213,-1.47659601580442,58.9160865280663));
#6545=CARTESIAN_POINT('Ctrl Pts',(3.85228499748508,-1.36434142572157,58.921893976757));
#6546=CARTESIAN_POINT('Ctrl Pts',(3.88889419766639,-1.25049067143929,58.9277014254477));
#6547=CARTESIAN_POINT('Ctrl Pts',(3.9255068021072,-1.13662933026876,58.9335094141683));
#6548=CARTESIAN_POINT('Ctrl Pts',(3.95711048011525,-1.02117191786059,58.9393174028889));
#6549=CARTESIAN_POINT('Ctrl Pts',(3.98358242959187,-0.904597162634811,58.9451253916095));
#6550=CARTESIAN_POINT('Ctrl Pts',(4.01006306097334,-0.787984174828753,58.9509352851542));
#6551=CARTESIAN_POINT('Ctrl Pts',(4.03140852632769,-0.670253512687353,58.9567451786988));
#6552=CARTESIAN_POINT('Ctrl Pts',(4.04754718700238,-0.55189380227464,58.9625550722435));
#6553=CARTESIAN_POINT('Ctrl Pts',(4.06370357871512,-0.433404053776822,58.9683713489351));
#6554=CARTESIAN_POINT('Ctrl Pts',(4.07464169228339,-0.314284281622832,58.9741876256268));
#6555=CARTESIAN_POINT('Ctrl Pts',(4.08034178029111,-0.195028090312132,58.9800039023184));
#6556=CARTESIAN_POINT('Ctrl Pts',(4.08604562287243,-0.0756933465039628,
58.9858240101157));
#6557=CARTESIAN_POINT('Ctrl Pts',(4.08650456688263,0.0437775887584125,58.9916441179129));
#6558=CARTESIAN_POINT('Ctrl Pts',(4.08175096073643,0.162892892807668,58.9974642257101));
#6559=CARTESIAN_POINT('Ctrl Pts',(4.07699067235224,0.282175639590705,59.0032925149478));
#6560=CARTESIAN_POINT('Ctrl Pts',(4.06700324362255,0.401101352731584,59.0091208041854));
#6561=CARTESIAN_POINT('Ctrl Pts',(4.05187264766116,0.519184983541846,59.014949093423));
#6562=CARTESIAN_POINT('Ctrl Pts',(4.04859599096257,0.544756978252116,59.0162112580476));
#6563=CARTESIAN_POINT('Ctrl Pts',(4.04507832130802,0.570289527183952,59.0174734226722));
#6564=CARTESIAN_POINT('Ctrl Pts',(4.04132080248762,0.595777786914541,59.0187355872969));
#6565=CARTESIAN_POINT('Ctrl Pts',(4.02399372819974,0.713311987255443,59.0245558163521));
#6566=CARTESIAN_POINT('Ctrl Pts',(4.00150705452874,0.830279252287219,59.0303760454074));
#6567=CARTESIAN_POINT('Ctrl Pts',(3.9739082330223,0.946191500446708,59.0361962744627));
#6568=CARTESIAN_POINT('Ctrl Pts',(3.94634404342939,1.0619582980856,59.0420092001022));
#6569=CARTESIAN_POINT('Ctrl Pts',(3.91368055870973,1.17667231773673,59.0478221257416));
#6570=CARTESIAN_POINT('Ctrl Pts',(3.87601678876237,1.28985226023457,59.0536350513811));
#6571=CARTESIAN_POINT('Ctrl Pts',(3.8383904348959,1.4029197670976,59.0594422023226));
#6572=CARTESIAN_POINT('Ctrl Pts',(3.79577380602717,1.51445584284936,59.0652493532641));
#6573=CARTESIAN_POINT('Ctrl Pts',(3.74831645208154,1.62399161791399,59.0710565042056));
#6574=CARTESIAN_POINT('Ctrl Pts',(3.69930625825683,1.73711148491725,59.0770536694402));
#6575=CARTESIAN_POINT('Ctrl Pts',(3.64513321897757,1.84809746915126,59.0830508346749));
#6576=CARTESIAN_POINT('Ctrl Pts',(3.58601726917939,1.95645218319979,59.0890479999095));
#6577=CARTESIAN_POINT('Ctrl Pts',(3.52883750725453,2.06125802280622,59.0948487437276));
#6578=CARTESIAN_POINT('Ctrl Pts',(3.46703376658915,2.1636018711068,59.1006494875457));
#6579=CARTESIAN_POINT('Ctrl Pts',(3.40085273196375,2.26305671504157,59.1064502313638));
#6580=CARTESIAN_POINT('Ctrl Pts',(3.33468094939703,2.36249765526422,59.1122501642423));
#6581=CARTESIAN_POINT('Ctrl Pts',(3.26413331623943,2.45905005402977,59.1180500971208));
#6582=CARTESIAN_POINT('Ctrl Pts',(3.18950029622193,2.5523151961308,59.1238500299992));
#6583=CARTESIAN_POINT('Ctrl Pts',(3.11486004490109,2.64558937482895,59.1296505248418));
#6584=CARTESIAN_POINT('Ctrl Pts',(3.03613387514371,2.73557534438076,59.1354510196843));
#6585=CARTESIAN_POINT('Ctrl Pts',(2.95365262978066,2.82190735896659,59.1412515145268));
#6586=CARTESIAN_POINT('Ctrl Pts',(2.8711438702172,2.9082681722974,59.1470539443059));
#6587=CARTESIAN_POINT('Ctrl Pts',(2.78487782617163,2.99097231118155,59.152856374085));
#6588=CARTESIAN_POINT('Ctrl Pts',(2.69522181074791,3.06969125334597,59.1586588038641));
#6589=CARTESIAN_POINT('Ctrl Pts',(2.60546590609003,3.14849789932825,59.1644676983546));
#6590=CARTESIAN_POINT('Ctrl Pts',(2.51231279877493,3.22331021641309,59.1702765928451));
#6591=CARTESIAN_POINT('Ctrl Pts',(2.41616256541551,3.29384022950184,59.1760854873356));
#6592=CARTESIAN_POINT('Ctrl Pts',(2.31994826942968,3.36441723507018,59.1818982521551));
#6593=CARTESIAN_POINT('Ctrl Pts',(2.22073320978952,3.43070602817889,59.1877110169746));
#6594=CARTESIAN_POINT('Ctrl Pts',(2.11894467561774,3.49246309381663,59.1935237817942));
#6595=CARTESIAN_POINT('Ctrl Pts',(2.01701091720085,3.55430826980305,59.1993448398305));
#6596=CARTESIAN_POINT('Ctrl Pts',(1.91249671358373,3.61160861883483,59.2051658978668));
#6597=CARTESIAN_POINT('Ctrl Pts',(1.80585213975437,3.66416744286401,59.2109869559032));
#6598=CARTESIAN_POINT('Ctrl Pts',(1.7814155885564,3.6762107784804,59.2123207938813));
#6599=CARTESIAN_POINT('Ctrl Pts',(1.75686725501579,3.6880053628731,59.2136546318593));
#6600=CARTESIAN_POINT('Ctrl Pts',(1.7322126759275,3.69954919488254,59.2149884698374));
#6601=CARTESIAN_POINT('Ctrl Pts',(1.6243304851827,3.75006207860726,59.2208250068418));
#6602=CARTESIAN_POINT('Ctrl Pts',(1.51406786472336,3.79593132511904,59.2266615438461));
#6603=CARTESIAN_POINT('Ctrl Pts',(1.4018606953227,3.83692736325688,59.2324980808505));
#6604=CARTESIAN_POINT('Ctrl Pts',(1.28979407647794,3.87787204981014,59.2383273070161));
#6605=CARTESIAN_POINT('Ctrl Pts',(1.17578813223202,3.9139555320868,59.2441565331817));
#6606=CARTESIAN_POINT('Ctrl Pts',(1.0603013915889,3.94499505183399,59.2499857593473));
#6607=CARTESIAN_POINT('Ctrl Pts',(0.944929590676493,3.97600367908199,59.2558091838973));
#6608=CARTESIAN_POINT('Ctrl Pts',(0.828080315782685,4.0019782267766,59.2616326084472));
#6609=CARTESIAN_POINT('Ctrl Pts',(0.710229496298609,4.0227849883616,59.2674560329971));
#6610=CARTESIAN_POINT('Ctrl Pts',(0.588986277256128,4.04419068382862,59.2734470879713));
#6611=CARTESIAN_POINT('Ctrl Pts',(0.466683389476337,4.06012641257512,59.2794381429455));
#6612=CARTESIAN_POINT('Ctrl Pts',(0.343853381635293,4.07050240780398,59.2854291979197));
#6613=CARTESIAN_POINT('Ctrl Pts',(0.224595022545729,4.08057669003081,59.2912460451055));
#6614=CARTESIAN_POINT('Ctrl Pts',(0.104840207494035,4.08541006779284,59.2970628922913));
#6615=CARTESIAN_POINT('Ctrl Pts',(-0.0149166290420977,4.08497276541448,
59.3028797394771));
#6616=CARTESIAN_POINT('Ctrl Pts',(-0.134654890628517,4.08453553086414,59.3086956844376));
#6617=CARTESIAN_POINT('Ctrl Pts',(-0.254394766907548,4.07882924373015,59.3145116293981));
#6618=CARTESIAN_POINT('Ctrl Pts',(-0.373641271704787,4.0678762518148,59.3203275743586));
#6619=CARTESIAN_POINT('Ctrl Pts',(-0.492897068477597,4.05692240641587,59.3261439725116));
#6620=CARTESIAN_POINT('Ctrl Pts',(-0.611659012737289,4.04072108060403,59.3319603706646));
#6621=CARTESIAN_POINT('Ctrl Pts',(-0.729437304627361,4.01934649148565,59.3377767688175));
#6622=CARTESIAN_POINT('Ctrl Pts',(-0.853404820528018,3.99684867228755,59.3438988174476));
#6623=CARTESIAN_POINT('Ctrl Pts',(-0.976282000004267,3.96861920300436,59.3500208660776));
#6624=CARTESIAN_POINT('Ctrl Pts',(-1.09751133468474,3.93480544248868,59.3561429147077));
#6625=CARTESIAN_POINT('Ctrl Pts',(-1.21285000561375,3.90263472896237,59.3619674864107));
#6626=CARTESIAN_POINT('Ctrl Pts',(-1.32669682307987,3.86540981904723,59.3677920581137));
#6627=CARTESIAN_POINT('Ctrl Pts',(-1.43858953256563,3.82330814306048,59.3736166298167));
#6628=CARTESIAN_POINT('Ctrl Pts',(-1.55055517746741,3.78117902379108,59.3794449981706));
#6629=CARTESIAN_POINT('Ctrl Pts',(-1.66056380461322,3.73416696619259,59.3852733665245));
#6630=CARTESIAN_POINT('Ctrl Pts',(-1.76817536986392,3.68249655280308,59.3911017348784));
#6631=CARTESIAN_POINT('Ctrl Pts',(-1.87593288195363,3.63075606206188,59.396938007884));
#6632=CARTESIAN_POINT('Ctrl Pts',(-1.98128648734886,3.57434479807323,59.4027742808896));
#6633=CARTESIAN_POINT('Ctrl Pts',(-2.08382278545184,3.5135320688492,59.4086105538952));
#6634=CARTESIAN_POINT('Ctrl Pts',(-2.09922944064847,3.50439461442521,59.4094874867228));
#6635=CARTESIAN_POINT('Ctrl Pts',(-2.11457254781778,3.49515786583985,59.4103644195504));
#6636=CARTESIAN_POINT('Ctrl Pts',(-2.12985076712583,3.4858228167498,59.4112413523781));
#6637=CARTESIAN_POINT('Ctrl Pts',(-2.23144216804306,3.42375009115478,59.4170724530236));
#6638=CARTESIAN_POINT('Ctrl Pts',(-2.33047596081803,3.35713581779339,59.4229035536691));
#6639=CARTESIAN_POINT('Ctrl Pts',(-2.42652081805006,3.28621693130105,59.4287346543146));
#6640=CARTESIAN_POINT('Ctrl Pts',(-2.5224473135942,3.21538544229515,59.4345585689542));
#6641=CARTESIAN_POINT('Ctrl Pts',(-2.61539187581421,3.14026013195042,59.4403824835938));
#6642=CARTESIAN_POINT('Ctrl Pts',(-2.70494976812292,3.06112262935214,59.4462063982334));
#6643=CARTESIAN_POINT('Ctrl Pts',(-2.79442043709696,2.98206220133317,59.4520246407737));
#6644=CARTESIAN_POINT('Ctrl Pts',(-2.88051069512174,2.89899762343173,59.457842883314));
#6645=CARTESIAN_POINT('Ctrl Pts',(-2.96284716265808,2.81225206742372,59.4636611258543));
#6646=CARTESIAN_POINT('Ctrl Pts',(-3.04765735257003,2.72290032208913,59.4696541720653));
#6647=CARTESIAN_POINT('Ctrl Pts',(-3.12848427370886,2.62964318008027,59.4756472182763));
#6648=CARTESIAN_POINT('Ctrl Pts',(-3.20495877380643,2.53287667646911,59.4816402644873));
#6649=CARTESIAN_POINT('Ctrl Pts',(-3.27912323320859,2.43903316759487,59.4874522806737));
#6650=CARTESIAN_POINT('Ctrl Pts',(-3.34919416765684,2.34188960451496,59.4932642968601));
#6651=CARTESIAN_POINT('Ctrl Pts',(-3.41487480817952,2.24184188658809,59.4990763130465));
#6652=CARTESIAN_POINT('Ctrl Pts',(-3.48054681238641,2.14180732388749,59.5048875650136));
#6653=CARTESIAN_POINT('Ctrl Pts',(-3.54182944750191,2.0388697059567,59.5106988169808));
#6654=CARTESIAN_POINT('Ctrl Pts',(-3.59846916632478,1.93345407470927,59.516510068948));
#6655=CARTESIAN_POINT('Ctrl Pts',(-3.65511469235969,1.82802763530572,59.5223219167368));
#6656=CARTESIAN_POINT('Ctrl Pts',(-3.70711616289021,1.72012303589154,59.5281337645257));
#6657=CARTESIAN_POINT('Ctrl Pts',(-3.75426620079138,1.61018952101777,59.5339456123145));
#6658=CARTESIAN_POINT('Ctrl Pts',(-3.80143210680293,1.50021900856721,59.5397594160518));
#6659=CARTESIAN_POINT('Ctrl Pts',(-3.84374317245761,1.38821859637699,59.545573219789));
#6660=CARTESIAN_POINT('Ctrl Pts',(-3.8810405605059,1.27465649008196,59.5513870235263));
#6661=CARTESIAN_POINT('Ctrl Pts',(-3.91837924876688,1.16096863398541,59.5572072650155));
#6662=CARTESIAN_POINT('Ctrl Pts',(-3.9506930508458,1.04571601888337,59.5630275065047));
#6663=CARTESIAN_POINT('Ctrl Pts',(-3.9778732688924,0.929381114845428,59.5688477479938));
#6664=CARTESIAN_POINT('Ctrl Pts',(-4.00507154745216,0.812968909438439,59.5746718568746));
#6665=CARTESIAN_POINT('Ctrl Pts',(-4.02712937328489,0.695473381826771,59.5804959657555));
#6666=CARTESIAN_POINT('Ctrl Pts',(-4.04398960873745,0.577384658978328,59.5863200746363));
#6667=CARTESIAN_POINT('Ctrl Pts',(-4.06087359175116,0.459129608727532,59.5921523867466));
#6668=CARTESIAN_POINT('Ctrl Pts',(-4.07254533364047,0.340280099194447,59.597984698857));
#6669=CARTESIAN_POINT('Ctrl Pts',(-4.07899969437103,0.221328925631193,59.6038170109674));
#6670=CARTESIAN_POINT('Ctrl Pts',(-4.080356167837,0.196329685982205,59.6050427522845));
#6671=CARTESIAN_POINT('Ctrl Pts',(-4.0814823787454,0.171325945607201,59.6062684936016));
#6672=CARTESIAN_POINT('Ctrl Pts',(-4.0823785710486,0.146322256144288,59.6074942349187));
#6673=CARTESIAN_POINT('Ctrl Pts',(-4.08411401076354,0.0979036348743599,
59.6098678328109));
#6674=CARTESIAN_POINT('Ctrl Pts',(-4.08498814701933,0.0494523315283915,
59.6122414307032));
#6675=CARTESIAN_POINT('Ctrl Pts',(-4.0849998802783,0.000989002666605911,
59.6146150285954));
#6676=CARTESIAN_POINT('Ctrl Pts',(-4.09175882131913,0.000965923615931607,
59.6146162370882));
#6677=CARTESIAN_POINT('Ctrl Pts',(-4.08719829507769,-1.28836881771013,59.6776598638786));
#6678=CARTESIAN_POINT('Ctrl Pts',(-3.41121669487228,-2.60606765915847,59.7419022275068));
#6679=CARTESIAN_POINT('Ctrl Pts',(-2.3368437494292,-3.35778115892392,59.806144591135));
#6680=CARTESIAN_POINT('Ctrl Pts',(-2.31666171942481,-3.3716102527404,59.8073433279728));
#6681=CARTESIAN_POINT('',(-4.08499993153545,0.000747900661492352,59.5103849713657));
#6682=CARTESIAN_POINT('Ctrl Pts',(-4.08499993153559,0.000747899860698453,
59.5103849714045));
#6683=CARTESIAN_POINT('Ctrl Pts',(-4.08502251884219,-0.122623089693615,
59.5163621312386));
#6684=CARTESIAN_POINT('Ctrl Pts',(-4.07945188006652,-0.245929705076146,
59.5223392910726));
#6685=CARTESIAN_POINT('Ctrl Pts',(-4.06833157303784,-0.368650528039084,
59.5283164509067));
#6686=CARTESIAN_POINT('Ctrl Pts',(-4.05720221521403,-0.491471233228483,
59.5342984755389));
#6687=CARTESIAN_POINT('Ctrl Pts',(-4.04051422026161,-0.613704825425184,
59.5402805001711));
#6688=CARTESIAN_POINT('Ctrl Pts',(-4.01836273482416,-0.73483735028681,59.5462625248033));
#6689=CARTESIAN_POINT('Ctrl Pts',(-3.9961705780107,-0.856192281292652,59.5522555327699));
#6690=CARTESIAN_POINT('Ctrl Pts',(-3.96849495158413,-0.976441738099162,
59.5582485407366));
#6691=CARTESIAN_POINT('Ctrl Pts',(-3.93548191022,-1.09508316320322,59.5642415487032));
#6692=CARTESIAN_POINT('Ctrl Pts',(-3.90243773520088,-1.21383647564159,59.5702402085042));
#6693=CARTESIAN_POINT('Ctrl Pts',(-3.86404622307644,-1.3309783788317,59.5762388683053));
#6694=CARTESIAN_POINT('Ctrl Pts',(-3.82050237163993,-1.4460244217487,59.5822375281063));
#6695=CARTESIAN_POINT('Ctrl Pts',(-3.77686641892775,-1.56131380297785,59.5882488759035));
#6696=CARTESIAN_POINT('Ctrl Pts',(-3.72805648758539,-1.67449811914711,59.5942602237007));
#6697=CARTESIAN_POINT('Ctrl Pts',(-3.67431506519386,-1.78511450660438,59.6002715714979));
#6698=CARTESIAN_POINT('Ctrl Pts',(-3.62627846373096,-1.88398861679892,59.6056447958291));
#6699=CARTESIAN_POINT('Ctrl Pts',(-3.57430252124013,-1.98081123881028,59.6110180201603));
#6700=CARTESIAN_POINT('Ctrl Pts',(-3.51858962983403,-2.07527155255028,59.6163912444915));
#6701=CARTESIAN_POINT('Ctrl Pts',(-3.45806815647434,-2.17788473986254,59.6222282320362));
#6702=CARTESIAN_POINT('Ctrl Pts',(-3.39295931187634,-2.27800909715532,59.628065219581));
#6703=CARTESIAN_POINT('Ctrl Pts',(-3.32349327159169,-2.3752089326383,59.6339022071257));
#6704=CARTESIAN_POINT('Ctrl Pts',(-3.25413214706056,-2.47226196554062,59.6397303789679));
#6705=CARTESIAN_POINT('Ctrl Pts',(-3.1804271623573,-2.56639894232262,59.6455585508101));
#6706=CARTESIAN_POINT('Ctrl Pts',(-3.10265341324178,-2.65721034118474,59.6513867226522));
#6707=CARTESIAN_POINT('Ctrl Pts',(-3.02494795657119,-2.74794199935638,59.657209776828));
#6708=CARTESIAN_POINT('Ctrl Pts',(-2.94318110155858,-2.83535357887629,59.6630328310038));
#6709=CARTESIAN_POINT('Ctrl Pts',(-2.85767008583671,-2.91906606306093,59.6688558851796));
#6710=CARTESIAN_POINT('Ctrl Pts',(-2.77221688508832,-3.00272194827978,59.674675002322));
#6711=CARTESIAN_POINT('Ctrl Pts',(-2.68302484836093,-3.08268342973667,59.6804941194644));
#6712=CARTESIAN_POINT('Ctrl Pts',(-2.59044974432747,-3.15860651587275,59.6863132366068));
#6713=CARTESIAN_POINT('Ctrl Pts',(-2.50112581472979,-3.23186323507023,59.6919279903289));
#6714=CARTESIAN_POINT('Ctrl Pts',(-2.40865271670227,-3.30136019072068,59.697542744051));
#6715=CARTESIAN_POINT('Ctrl Pts',(-2.31338095599003,-3.36682247118298,59.7031574977731));
#6716=CARTESIAN_POINT('Ctrl Pts',(-2.31338095599002,-3.36682247118298,58.4531830718678));
#6717=CARTESIAN_POINT('Ctrl Pts',(-2.21522106941994,-3.434269214864,58.4590037287315));
#6718=CARTESIAN_POINT('Ctrl Pts',(-2.11397617042823,-3.49751096136364,58.4648243855952));
#6719=CARTESIAN_POINT('Ctrl Pts',(-2.01004239296545,-3.55625569644278,58.470645042459));
#6720=CARTESIAN_POINT('Ctrl Pts',(-1.90621654655831,-3.61493942747276,58.4764596548042));
#6721=CARTESIAN_POINT('Ctrl Pts',(-1.79970772942948,-3.66913523793015,58.4822742671494));
#6722=CARTESIAN_POINT('Ctrl Pts',(-1.69094135890495,-3.71859413229579,58.4880888794947));
#6723=CARTESIAN_POINT('Ctrl Pts',(-1.58225969137649,-3.76801451000858,58.4938989636472));
#6724=CARTESIAN_POINT('Ctrl Pts',(-1.4713243386094,-3.8127051437847,58.4997090477997));
#6725=CARTESIAN_POINT('Ctrl Pts',(-1.35858511553482,-3.85246304120458,58.5055191319523));
#6726=CARTESIAN_POINT('Ctrl Pts',(-1.24589412383802,-3.89220392965351,58.5113267304715));
#6727=CARTESIAN_POINT('Ctrl Pts',(-1.13140118013004,-3.92701614223388,58.5171343289908));
#6728=CARTESIAN_POINT('Ctrl Pts',(-1.01557543709463,-3.95674506780132,58.52294192751));
#6729=CARTESIAN_POINT('Ctrl Pts',(-0.899772102726297,-3.98646824174931,
58.5287484024402));
#6730=CARTESIAN_POINT('Ctrl Pts',(-0.78263687664277,-4.01110998312592,58.5345548773704));
#6731=CARTESIAN_POINT('Ctrl Pts',(-0.664652793827197,-4.03056592349731,
58.5403613523005));
#6732=CARTESIAN_POINT('Ctrl Pts',(-0.546663784263447,-4.05002267630472,
58.5461680696959));
#6733=CARTESIAN_POINT('Ctrl Pts',(-0.427826249896556,-4.06429313134262,
58.5519747870913));
#6734=CARTESIAN_POINT('Ctrl Pts',(-0.308631476980936,-4.07332439309915,
58.5577815044867));
#6735=CARTESIAN_POINT('Ctrl Pts',(-0.189403689256998,-4.08235815635276,
58.5635898302384));
#6736=CARTESIAN_POINT('Ctrl Pts',(-0.0698188726936143,-4.0861498095383,
58.5693981559901));
#6737=CARTESIAN_POINT('Ctrl Pts',(0.0496291692062076,-4.08469851342347,
58.5752064817418));
#6738=CARTESIAN_POINT('Ctrl Pts',(0.169205615726446,-4.08324565718991,58.5810210513452));
#6739=CARTESIAN_POINT('Ctrl Pts',(0.288644585880642,-4.07653860439837,58.5868356209487));
#6740=CARTESIAN_POINT('Ctrl Pts',(0.407454694668163,-4.06462860195035,58.5926501905521));
#6741=CARTESIAN_POINT('Ctrl Pts',(0.526337680284906,-4.0527112940363,58.5984683267493));
#6742=CARTESIAN_POINT('Ctrl Pts',(0.644590633258377,-4.03558473806075,58.6042864629465));
#6743=CARTESIAN_POINT('Ctrl Pts',(0.761731344424355,-4.01335151200608,58.6101045991437));
#6744=CARTESIAN_POINT('Ctrl Pts',(0.879043461512295,-3.99108575322583,58.6159312487176));
#6745=CARTESIAN_POINT('Ctrl Pts',(0.995239691297029,-3.96369849841228,58.6217578982915));
#6746=CARTESIAN_POINT('Ctrl Pts',(1.10985173705642,-3.93134253426903,58.6275845478654));
#6747=CARTESIAN_POINT('Ctrl Pts',(1.15930477629944,-3.91738151687404,58.6300986425064));
#6748=CARTESIAN_POINT('Ctrl Pts',(1.20846311401074,-3.90249605722148,58.6326127371474));
#6749=CARTESIAN_POINT('Ctrl Pts',(1.25729032293254,-3.88670117758752,58.6351268317883));
#6750=CARTESIAN_POINT('Ctrl Pts',(1.37045573134724,-3.850093842372,58.6409536761466));
#6751=CARTESIAN_POINT('Ctrl Pts',(1.48220101786181,-3.80848178787127,58.6467805205049));
#6752=CARTESIAN_POINT('Ctrl Pts',(1.59205196469652,-3.7619935594982,58.6526073648632));
#6753=CARTESIAN_POINT('Ctrl Pts',(1.70176552280632,-3.71556347316763,58.6584269216856));
#6754=CARTESIAN_POINT('Ctrl Pts',(1.80958908142062,-3.66426950082316,58.664246478508));
#6755=CARTESIAN_POINT('Ctrl Pts',(1.91506372861185,-3.60828988793241,58.6700660353305));
#6756=CARTESIAN_POINT('Ctrl Pts',(2.02043385696985,-3.55236574736586,58.675879825333));
#6757=CARTESIAN_POINT('Ctrl Pts',(2.12345934641995,-3.49176539371288,58.6816936153356));
#6758=CARTESIAN_POINT('Ctrl Pts',(2.22370197573578,-3.42671482955743,58.6875074053382));
#6759=CARTESIAN_POINT('Ctrl Pts',(2.32706354174668,-3.35964029024326,58.6935020848795));
#6760=CARTESIAN_POINT('Ctrl Pts',(2.42746583767444,-3.28783425661528,58.6994967644208));
#6761=CARTESIAN_POINT('Ctrl Pts',(2.52445626156305,-3.21159548876491,58.705491443962));
#6762=CARTESIAN_POINT('Ctrl Pts',(2.61841597281109,-3.13773899524804,58.7112988044842));
#6763=CARTESIAN_POINT('Ctrl Pts',(2.70917351844038,-3.05972293732472,58.7171061650065));
#6764=CARTESIAN_POINT('Ctrl Pts',(2.79634807355528,-2.97786206052659,58.7229135255287));
#6765=CARTESIAN_POINT('Ctrl Pts',(2.88351016067287,-2.89601289174568,58.7287200554627));
#6766=CARTESIAN_POINT('Ctrl Pts',(2.96708997926215,-2.81032027680275,58.7345265853967));
#6767=CARTESIAN_POINT('Ctrl Pts',(3.0467418741869,-2.72113743718984,58.7403331153308));
#6768=CARTESIAN_POINT('Ctrl Pts',(3.12640111095747,-2.63194637722438,58.7461401804768));
#6769=CARTESIAN_POINT('Ctrl Pts',(3.20213143257101,-2.53926475710069,58.7519472456228));
#6770=CARTESIAN_POINT('Ctrl Pts',(3.27362638703625,-2.44348015709152,58.7577543107688));
#6771=CARTESIAN_POINT('Ctrl Pts',(3.34514474677619,-2.34766420011609,58.7635632769714));
#6772=CARTESIAN_POINT('Ctrl Pts',(3.41242473802761,-2.24874356957999,58.769372243174));
#6773=CARTESIAN_POINT('Ctrl Pts',(3.4752026518956,-2.14713565669656,58.7751812093766));
#6774=CARTESIAN_POINT('Ctrl Pts',(3.53804953997439,-2.04541610701017,58.7809965579011));
#6775=CARTESIAN_POINT('Ctrl Pts',(3.59638426302548,-1.94100372876592,58.7868119064257));
#6776=CARTESIAN_POINT('Ctrl Pts',(3.64998851774923,-1.83434152226318,58.7926272549503));
#6777=CARTESIAN_POINT('Ctrl Pts',(3.70362807252076,-1.72760907542214,58.7984464330604));
#6778=CARTESIAN_POINT('Ctrl Pts',(3.75253078833386,-1.61862422079623,58.8042656111706));
#6779=CARTESIAN_POINT('Ctrl Pts',(3.79652669891199,-1.50784947008926,58.8100847892808));
#6780=CARTESIAN_POINT('Ctrl Pts',(3.84058450163022,-1.39691888475353,58.8159121536378));
#6781=CARTESIAN_POINT('Ctrl Pts',(3.87972158923193,-1.28419376169753,58.8217395179949));
#6782=CARTESIAN_POINT('Ctrl Pts',(3.91381792787329,-1.17015136946363,58.8275668823519));
#6783=CARTESIAN_POINT('Ctrl Pts',(3.92125431490904,-1.14527880540173,58.8288378263443));
#6784=CARTESIAN_POINT('Ctrl Pts',(3.9284511208704,-1.12034361763696,58.8301087703366));
#6785=CARTESIAN_POINT('Ctrl Pts',(3.93540742551294,-1.09535080920115,58.831379714329));
#6786=CARTESIAN_POINT('Ctrl Pts',(3.96729404086616,-0.980787674010631,58.8372055233328));
#6787=CARTESIAN_POINT('Ctrl Pts',(3.99422479012238,-0.864648383214477,58.8430313323366));
#6788=CARTESIAN_POINT('Ctrl Pts',(4.01604524613472,-0.747399211264446,58.8488571413404));
#6789=CARTESIAN_POINT('Ctrl Pts',(4.03783839578895,-0.630296766214877,58.8546756598628));
#6790=CARTESIAN_POINT('Ctrl Pts',(4.05453389821043,-0.512087600206339,58.8604941783853));
#6791=CARTESIAN_POINT('Ctrl Pts',(4.06602722001259,-0.393252649217582,58.8663126969078));
#6792=CARTESIAN_POINT('Ctrl Pts',(4.07750914731762,-0.274535511384376,58.8721254469419));
#6793=CARTESIAN_POINT('Ctrl Pts',(4.08379911534598,-0.155194226590116,58.877938196976));
#6794=CARTESIAN_POINT('Ctrl Pts',(4.08484383610604,-0.035718827339529,58.8837509470102));
#6795=CARTESIAN_POINT('Ctrl Pts',(4.08592132485717,0.0875039549122769,58.8897460157543));
#6796=CARTESIAN_POINT('Ctrl Pts',(4.08141902440324,0.210868969000254,58.8957410844985));
#6797=CARTESIAN_POINT('Ctrl Pts',(4.07133640056975,0.333833661268243,58.9017361532426));
#6798=CARTESIAN_POINT('Ctrl Pts',(4.06157121290607,0.452926996081961,58.9075424763099));
#6799=CARTESIAN_POINT('Ctrl Pts',(4.04657184074196,0.571644401307267,58.9133487993772));
#6800=CARTESIAN_POINT('Ctrl Pts',(4.02639068993385,0.689494751259203,58.9191551224445));
#6801=CARTESIAN_POINT('Ctrl Pts',(4.00621241647675,0.807328298560677,58.9249606176685));
#6802=CARTESIAN_POINT('Ctrl Pts',(3.98085390252483,0.924294634459594,58.9307661128925));
#6803=CARTESIAN_POINT('Ctrl Pts',(3.95041904743944,1.03991074118293,58.9365716081166));
#6804=CARTESIAN_POINT('Ctrl Pts',(3.91998136621631,1.15553758385502,58.9423776424307));
#6805=CARTESIAN_POINT('Ctrl Pts',(3.88446651049147,1.26981355354743,58.9481836767449));
#6806=CARTESIAN_POINT('Ctrl Pts',(3.84402866362447,1.38226937795551,58.953989711059));
#6807=CARTESIAN_POINT('Ctrl Pts',(3.8035775413578,1.49476212065002,58.9597976514446));
#6808=CARTESIAN_POINT('Ctrl Pts',(3.75820035165562,1.60543314600411,58.9656055918302));
#6809=CARTESIAN_POINT('Ctrl Pts',(3.70809972046971,1.71383239059496,58.9714135322158));
#6810=CARTESIAN_POINT('Ctrl Pts',(3.65794392604076,1.8223509880509,58.9772278674276));
#6811=CARTESIAN_POINT('Ctrl Pts',(3.60305448060662,1.92859244153204,58.9830422026393));
#6812=CARTESIAN_POINT('Ctrl Pts',(3.54368041622873,2.03213043568491,58.9888565378511));
#6813=CARTESIAN_POINT('Ctrl Pts',(3.48426718240505,2.13573673450739,58.9946747088166));
#6814=CARTESIAN_POINT('Ctrl Pts',(3.4203636553121,2.23663567827114,59.0004928797821));
#6815=CARTESIAN_POINT('Ctrl Pts',(3.35226180162721,2.33443051157046,59.0063110507475));
#6816=CARTESIAN_POINT('Ctrl Pts',(3.28406393522339,2.43236321993974,59.0121374244033));
#6817=CARTESIAN_POINT('Ctrl Pts',(3.21165617573436,2.52718276057776,59.0179637980591));
#6818=CARTESIAN_POINT('Ctrl Pts',(3.13537033821866,2.6185258910728,59.0237901717148));
#6819=CARTESIAN_POINT('Ctrl Pts',(3.11860046623421,2.63860579915201,59.0250709800998));
#6820=CARTESIAN_POINT('Ctrl Pts',(3.10164332450812,2.65851785412056,59.0263517884847));
#6821=CARTESIAN_POINT('Ctrl Pts',(3.0845026659662,2.67825844601439,59.0276325968696));
#6822=CARTESIAN_POINT('Ctrl Pts',(3.00651290656505,2.7680778662234,59.0334602573142));
#6823=CARTESIAN_POINT('Ctrl Pts',(2.92447268937666,2.85463067025238,59.0392879177588));
#6824=CARTESIAN_POINT('Ctrl Pts',(2.83868600491129,2.9375307258854,59.0451155782034));
#6825=CARTESIAN_POINT('Ctrl Pts',(2.75300667715892,3.02032703724229,59.0509359456925));
#6826=CARTESIAN_POINT('Ctrl Pts',(2.66359049839989,3.09947941171397,59.0567563131816));
#6827=CARTESIAN_POINT('Ctrl Pts',(2.57078120099155,3.17463525725845,59.0625766806707));
#6828=CARTESIAN_POINT('Ctrl Pts',(2.47806395968989,3.24971655688213,59.0683912750273));
#6829=CARTESIAN_POINT('Ctrl Pts',(2.38196061045916,3.32080895886833,59.074205869384));
#6830=CARTESIAN_POINT('Ctrl Pts',(2.28285073276569,3.38759760477999,59.0800204637406));
#6831=CARTESIAN_POINT('Ctrl Pts',(2.18067647926323,3.45645128715029,59.0860148393935));
#6832=CARTESIAN_POINT('Ctrl Pts',(2.07530707447446,3.52073044491613,59.0920092150464));
#6833=CARTESIAN_POINT('Ctrl Pts',(1.96719442957651,3.5801356226047,59.0980035906993));
#6834=CARTESIAN_POINT('Ctrl Pts',(1.86244059479987,3.63769521865695,59.1038117349485));
#6835=CARTESIAN_POINT('Ctrl Pts',(1.75511183269771,3.69067898844718,59.1096198791978));
#6836=CARTESIAN_POINT('Ctrl Pts',(1.64564691528913,3.73885961627331,59.115428023447));
#6837=CARTESIAN_POINT('Ctrl Pts',(1.53619782095155,3.78703327962613,59.1212353281334));
#6838=CARTESIAN_POINT('Ctrl Pts',(1.42461355843513,3.83040501766096,59.1270426328197));
#6839=CARTESIAN_POINT('Ctrl Pts',(1.31135454404858,3.86879493638564,59.1328499375061));
#6840=CARTESIAN_POINT('Ctrl Pts',(1.19808528248824,3.90718832846005,59.1386577676117));
#6841=CARTESIAN_POINT('Ctrl Pts',(1.08314135388968,3.94059887419651,59.1444655977172));
#6842=CARTESIAN_POINT('Ctrl Pts',(0.966999453192039,3.96889620140491,59.1502734278228));
#6843=CARTESIAN_POINT('Ctrl Pts',(0.850819748518538,3.99720273934145,59.1560831483664));
#6844=CARTESIAN_POINT('Ctrl Pts',(0.733441692089495,4.0203926522191,59.1618928689101));
#6845=CARTESIAN_POINT('Ctrl Pts',(0.615352688683319,4.03838656749576,59.1677025894537));
#6846=CARTESIAN_POINT('Ctrl Pts',(0.49713435044164,4.05640019028121,59.1735186729882));
#6847=CARTESIAN_POINT('Ctrl Pts',(0.37820391423102,4.06920639500047,59.1793347565227));
#6848=CARTESIAN_POINT('Ctrl Pts',(0.259054585734492,4.07677761493191,59.1851508400572));
#6849=CARTESIAN_POINT('Ctrl Pts',(0.139827018305857,4.08435380647477,59.1909707426998));
#6850=CARTESIAN_POINT('Ctrl Pts',(0.0203806789546916,4.08668815908609,59.1967906453424));
#6851=CARTESIAN_POINT('Ctrl Pts',(-0.0987921802569579,4.08380522370008,
59.202610547985));
#6852=CARTESIAN_POINT('Ctrl Pts',(-0.218132247600786,4.08091824334742,59.2084386163715));
#6853=CARTESIAN_POINT('Ctrl Pts',(-0.337197663778942,4.07279939271625,59.214266684758));
#6854=CARTESIAN_POINT('Ctrl Pts',(-0.455502130741042,4.059524948672,59.2200947531445));
#6855=CARTESIAN_POINT('Ctrl Pts',(-0.481151558105484,4.0566469348737,59.2213583285664));
#6856=CARTESIAN_POINT('Ctrl Pts',(-0.506765259176913,4.05352676730336,59.2226219039883));
#6857=CARTESIAN_POINT('Ctrl Pts',(-0.53233835602326,4.0501655367042,59.2238854794102));
#6858=CARTESIAN_POINT('Ctrl Pts',(-0.650283495193144,4.03466327613791,59.2297131888927));
#6859=CARTESIAN_POINT('Ctrl Pts',(-0.767737928515811,4.01398013173085,59.2355408983752));
#6860=CARTESIAN_POINT('Ctrl Pts',(-0.884211867592764,3.98815676387076,59.2413686078577));
#6861=CARTESIAN_POINT('Ctrl Pts',(-1.00054039203771,3.96236563580238,59.2471890415991));
#6862=CARTESIAN_POINT('Ctrl Pts',(-1.11589046253476,3.93144713644343,59.2530094753404));
#6863=CARTESIAN_POINT('Ctrl Pts',(-1.22977835674899,3.89549357505204,59.2588299090818));
#6864=CARTESIAN_POINT('Ctrl Pts',(-1.34355361914526,3.85957557068812,59.2646445865833));
#6865=CARTESIAN_POINT('Ctrl Pts',(-1.455869195571,3.81863253291981,59.2704592640848));
#6866=CARTESIAN_POINT('Ctrl Pts',(-1.56625307524593,3.77280748306651,59.2762739415864));
#6867=CARTESIAN_POINT('Ctrl Pts',(-1.68004781323775,3.72556644065275,59.2822682924349));
#6868=CARTESIAN_POINT('Ctrl Pts',(-1.79178910556303,3.67313687184631,59.2882626432834));
#6869=CARTESIAN_POINT('Ctrl Pts',(-1.90097793319669,3.61573061738554,59.2942569941319));
#6870=CARTESIAN_POINT('Ctrl Pts',(-2.00677721407015,3.56010642422207,59.3000652624577));
#6871=CARTESIAN_POINT('Ctrl Pts',(-2.11017977211938,3.49981016210914,59.3058735307836));
#6872=CARTESIAN_POINT('Ctrl Pts',(-2.21075398360769,3.43508250613617,59.3116817991094));
#6873=CARTESIAN_POINT('Ctrl Pts',(-2.31131391457538,3.37036404083555,59.3174892427198));
#6874=CARTESIAN_POINT('Ctrl Pts',(-2.40904595500098,3.30121565361789,59.3232966863303));
#6875=CARTESIAN_POINT('Ctrl Pts',(-2.50354610561273,3.22792222599482,59.3291041299408));
#6876=CARTESIAN_POINT('Ctrl Pts',(-2.59805504383908,3.15462198278055,59.3349121135882));
#6877=CARTESIAN_POINT('Ctrl Pts',(-2.68933117259142,3.07717618261264,59.3407200972356));
#6878=CARTESIAN_POINT('Ctrl Pts',(-2.7770028274467,2.99591059552067,59.3465280808831));
#6879=CARTESIAN_POINT('Ctrl Pts',(-2.86470323586026,2.91461835586011,59.3523379693674));
#6880=CARTESIAN_POINT('Ctrl Pts',(-2.94879652047481,2.82950411467823,59.3581478578516));
#6881=CARTESIAN_POINT('Ctrl Pts',(-3.02894765507416,2.74093070011278,59.3639577463359));
#6882=CARTESIAN_POINT('Ctrl Pts',(-3.10918684988492,2.65225997197029,59.3697740180112));
#6883=CARTESIAN_POINT('Ctrl Pts',(-3.18547497594834,2.56012278692757,59.3755902896866));
#6884=CARTESIAN_POINT('Ctrl Pts',(-3.25751702354118,2.46491538218646,59.381406561362));
#6885=CARTESIAN_POINT('Ctrl Pts',(-3.32960652458181,2.36964526518547,59.3872266641631));
#6886=CARTESIAN_POINT('Ctrl Pts',(-3.39744414603443,2.27130123557681,59.3930467669642));
#6887=CARTESIAN_POINT('Ctrl Pts',(-3.46077888069734,2.17030747566313,59.3988668697653));
#6888=CARTESIAN_POINT('Ctrl Pts',(-3.52420264704673,2.06917174555227,59.4046951540733));
#6889=CARTESIAN_POINT('Ctrl Pts',(-3.583110692876,1.96537920425242,59.4105234383813));
#6890=CARTESIAN_POINT('Ctrl Pts',(-3.63729844346071,1.85937759295907,59.4163517226893));
#6891=CARTESIAN_POINT('Ctrl Pts',(-3.6490337131111,1.83642115947586,59.4176139357765));
#6892=CARTESIAN_POINT('Ctrl Pts',(-3.66054777696709,1.81336118679001,59.4188761488637));
#6893=CARTESIAN_POINT('Ctrl Pts',(-3.67183886052013,1.79020233001028,59.4201383619509));
#6894=CARTESIAN_POINT('Ctrl Pts',(-3.72759460119396,1.67584313615196,59.4263712115471));
#6895=CARTESIAN_POINT('Ctrl Pts',(-3.77806724379518,1.55874737083152,59.4326040611434));
#6896=CARTESIAN_POINT('Ctrl Pts',(-3.82299955405977,1.43940939612703,59.4388369107396));
#6897=CARTESIAN_POINT('Ctrl Pts',(-3.86779625853553,1.32043158363325,59.4450509495851));
#6898=CARTESIAN_POINT('Ctrl Pts',(-3.9070858607795,1.19922535306526,59.4512649884307));
#6899=CARTESIAN_POINT('Ctrl Pts',(-3.94065870003593,1.07630572321767,59.4574790272762));
#6900=CARTESIAN_POINT('Ctrl Pts',(-3.97416997482929,0.953611498226502,59.4636816710782));
#6901=CARTESIAN_POINT('Ctrl Pts',(-4.00198528966692,0.829210439627046,59.4698843148802));
#6902=CARTESIAN_POINT('Ctrl Pts',(-4.02394358429263,0.703635580702222,59.4760869586822));
#6903=CARTESIAN_POINT('Ctrl Pts',(-4.04584137768624,0.578406715572335,59.4822725124689));
#6904=CARTESIAN_POINT('Ctrl Pts',(-4.06191427259615,0.452010811417527,59.4884580662555));
#6905=CARTESIAN_POINT('Ctrl Pts',(-4.07205165169264,0.324992839839935,59.4946436200422));
#6906=CARTESIAN_POINT('Ctrl Pts',(-4.08065104588121,0.217245305074713,59.49989073715));
#6907=CARTESIAN_POINT('Ctrl Pts',(-4.08498010299262,0.109050513921404,59.5051378542579));
#6908=CARTESIAN_POINT('Ctrl Pts',(-4.08499993153545,0.00074790066148241,
59.5103849713657));
#6909=CARTESIAN_POINT('Origin',(0.,0.,46.4896150285955));
#6910=CARTESIAN_POINT('',(-2.31338095599003,-3.36682247118298,57.2030181077425));
#6911=CARTESIAN_POINT('',(-2.31338095599002,-3.36682247118298,57.3074490595572));
#6912=CARTESIAN_POINT('',(-2.31338095599002,-3.36682247118298,46.4896150285955));
#6913=CARTESIAN_POINT('',(-4.08499891745875,-0.00297394700961989,58.3646150286342));
#6914=CARTESIAN_POINT('Ctrl Pts',(-2.31338095599002,-3.36682247118298,57.3074490595572));
#6915=CARTESIAN_POINT('Ctrl Pts',(-2.2136460283599,-3.43535144299583,57.3133350373661));
#6916=CARTESIAN_POINT('Ctrl Pts',(-2.11079358198057,-3.49949301292074,57.3192210151751));
#6917=CARTESIAN_POINT('Ctrl Pts',(-2.00524962729991,-3.55896037238595,57.325106992984));
#6918=CARTESIAN_POINT('Ctrl Pts',(-1.90112271487449,-3.61762931794462,57.3309139451463));
#6919=CARTESIAN_POINT('Ctrl Pts',(-1.79437649443802,-3.67174859926997,57.3367208973086));
#6920=CARTESIAN_POINT('Ctrl Pts',(-1.68544775461599,-3.72108732314359,57.3425278494708));
#6921=CARTESIAN_POINT('Ctrl Pts',(-1.57653124128274,-3.77042050909071,57.3483341498434));
#6922=CARTESIAN_POINT('Ctrl Pts',(-1.46543306721513,-3.81497403657739,57.3541404502159));
#6923=CARTESIAN_POINT('Ctrl Pts',(-1.35261202454224,-3.85456426993555,57.3599467505885));
#6924=CARTESIAN_POINT('Ctrl Pts',(-1.23977710421394,-3.89415937312652,57.3657537651703));
#6925=CARTESIAN_POINT('Ctrl Pts',(-1.12521927870738,-3.92878983321132,57.3715607797521));
#6926=CARTESIAN_POINT('Ctrl Pts',(-1.00941399117484,-3.95832141120709,57.3773677943339));
#6927=CARTESIAN_POINT('Ctrl Pts',(-0.890849090619016,-3.98855671982666,
57.3833131887204));
#6928=CARTESIAN_POINT('Ctrl Pts',(-0.770976956570396,-4.01344694300943,
57.3892585831069));
#6929=CARTESIAN_POINT('Ctrl Pts',(-0.650319266757598,-4.03290340217614,
57.3952039774934));
#6930=CARTESIAN_POINT('Ctrl Pts',(-0.532294865405861,-4.05193523470284,
57.4010196168807));
#6931=CARTESIAN_POINT('Ctrl Pts',(-0.413519261976091,-4.06576806349613,
57.4068352562681));
#6932=CARTESIAN_POINT('Ctrl Pts',(-0.294485206654571,-4.07437154209844,
57.4126508956554));
#6933=CARTESIAN_POINT('Ctrl Pts',(-0.171467428466069,-4.08326295405185,
57.4186611675415));
#6934=CARTESIAN_POINT('Ctrl Pts',(-0.0481740771729017,-4.08656885330446,
57.4246714394275));
#6935=CARTESIAN_POINT('Ctrl Pts',(0.0748529556290137,-4.08431414499835,
57.4306817113135));
#6936=CARTESIAN_POINT('Ctrl Pts',(0.197879988430929,-4.08205943669224,57.4366919831996));
#6937=CARTESIAN_POINT('Ctrl Pts',(0.320640233957287,-4.07424421589866,57.4427022550856));
#6938=CARTESIAN_POINT('Ctrl Pts',(0.442600890991567,-4.06095179130379,57.4487125269716));
#6939=CARTESIAN_POINT('Ctrl Pts',(0.560835448643127,-4.048065472221,57.4545391751309));
#6940=CARTESIAN_POINT('Ctrl Pts',(0.67869492964639,-4.02999076694206,57.4603658232901));
#6941=CARTESIAN_POINT('Ctrl Pts',(0.795688927702892,-4.00675730863887,57.4661924714494));
#6942=CARTESIAN_POINT('Ctrl Pts',(0.912536563359301,-3.98355291596962,57.4720118303269));
#6943=CARTESIAN_POINT('Ctrl Pts',(1.02852047313209,-3.9552026857757,57.4778311892045));
#6944=CARTESIAN_POINT('Ctrl Pts',(1.14315515176311,-3.92178802321052,57.483650548082));
#6945=CARTESIAN_POINT('Ctrl Pts',(1.25767620141708,-3.8884064821577,57.4894641386545));
#6946=CARTESIAN_POINT('Ctrl Pts',(1.37085029127783,-3.84997060923041,57.495277729227));
#6947=CARTESIAN_POINT('Ctrl Pts',(1.48220248464921,-3.80661277180904,57.5010913197995));
#6948=CARTESIAN_POINT('Ctrl Pts',(1.59702463614523,-3.76190381703945,57.5070860735376));
#6949=CARTESIAN_POINT('Ctrl Pts',(1.70990905028883,-3.71196120252409,57.5130808272756));
#6950=CARTESIAN_POINT('Ctrl Pts',(1.82035187681997,-3.65698565003447,57.5190755810136));
#6951=CARTESIAN_POINT('Ctrl Pts',(1.92733859398976,-3.6037304584553,57.5248827397293));
#6952=CARTESIAN_POINT('Ctrl Pts',(2.03203386317524,-3.54575282016584,57.530689898445));
#6953=CARTESIAN_POINT('Ctrl Pts',(2.13400094306043,-3.48328364837221,57.5364970571606));
#6954=CARTESIAN_POINT('Ctrl Pts',(2.23595342963761,-3.42082341703137,57.5423033847683));
#6955=CARTESIAN_POINT('Ctrl Pts',(2.33517815579904,-3.35387314361274,57.548109712376));
#6956=CARTESIAN_POINT('Ctrl Pts',(2.43126501140071,-3.28270855306083,57.5539160399836));
#6957=CARTESIAN_POINT('Ctrl Pts',(2.52736071919643,-3.21153740632845,57.5597229025109));
#6958=CARTESIAN_POINT('Ctrl Pts',(2.62031765393769,-3.13615141324877,57.5655297650381));
#6959=CARTESIAN_POINT('Ctrl Pts',(2.7097571218915,-3.05686789710617,57.5713366275653));
#6960=CARTESIAN_POINT('Ctrl Pts',(2.79922586962693,-2.97755842593396,57.577145391084));
#6961=CARTESIAN_POINT('Ctrl Pts',(2.88517455542489,-2.89434916448145,57.5829541546028));
#6962=CARTESIAN_POINT('Ctrl Pts',(2.96726029135002,-2.8075952990731,57.5887629181215));
#6963=CARTESIAN_POINT('Ctrl Pts',(3.04943623127523,-2.72074609985805,57.5945780648894));
#6964=CARTESIAN_POINT('Ctrl Pts',(3.12774046780224,-2.63034481823913,57.6003932116572));
#6965=CARTESIAN_POINT('Ctrl Pts',(3.20186937860885,-2.53678092911606,57.6062083584251));
#6966=CARTESIAN_POINT('Ctrl Pts',(3.27604711129668,-2.44315541808285,57.6120273350942));
#6967=CARTESIAN_POINT('Ctrl Pts',(3.34604380321781,-2.34636348092971,57.6178463117633));
#6968=CARTESIAN_POINT('Ctrl Pts',(3.41159920560623,-2.24682350448515,57.6236652884323));
#6969=CARTESIAN_POINT('Ctrl Pts',(3.47724685475701,-2.14714345963711,57.6294924533168));
#6970=CARTESIAN_POINT('Ctrl Pts',(3.53844053296473,-2.04470800660846,57.6353196182014));
#6971=CARTESIAN_POINT('Ctrl Pts',(3.5949658918695,-1.93996011203709,57.6411467830859));
#6972=CARTESIAN_POINT('Ctrl Pts',(3.60731319017287,-1.91707916928886,57.6424196585613));
#6973=CARTESIAN_POINT('Ctrl Pts',(3.61943792153851,-1.8940879618285,57.6436925340368));
#6974=CARTESIAN_POINT('Ctrl Pts',(3.63133816117021,-1.87099122371779,57.6449654095123));
#6975=CARTESIAN_POINT('Ctrl Pts',(3.68581231873255,-1.76526433165857,57.65079208371));
#6976=CARTESIAN_POINT('Ctrl Pts',(3.73575195601721,-1.6569881857762,57.6566187579076));
#6977=CARTESIAN_POINT('Ctrl Pts',(3.78091126622735,-1.54658817948253,57.6624454321053));
#6978=CARTESIAN_POINT('Ctrl Pts',(3.82601408348645,-1.43632628030613,57.6682648173072));
#6979=CARTESIAN_POINT('Ctrl Pts',(3.86634831518234,-1.32394617958235,57.6740842025091));
#6980=CARTESIAN_POINT('Ctrl Pts',(3.90171404063422,-1.20989774159545,57.679903587711));
#6981=CARTESIAN_POINT('Ctrl Pts',(3.9370447123089,-1.0959623460666,57.6857172048584));
#6982=CARTESIAN_POINT('Ctrl Pts',(3.96741655501291,-0.980362290389359,57.6915308220058));
#6983=CARTESIAN_POINT('Ctrl Pts',(3.99267798510178,-0.863566735859806,57.6973444391532));
#6984=CARTESIAN_POINT('Ctrl Pts',(4.0187264501716,-0.743132345891777,57.7033391830241));
#6985=CARTESIAN_POINT('Ctrl Pts',(4.03934068463659,-0.621427152793105,57.7093339268949));
#6986=CARTESIAN_POINT('Ctrl Pts',(4.05441017078938,-0.498982130942181,57.7153286707657));
#6987=CARTESIAN_POINT('Ctrl Pts',(4.0690081764639,-0.38036805839366,57.7211358565022));
#6988=CARTESIAN_POINT('Ctrl Pts',(4.07840316568417,-0.261060195461489,57.7269430422388));
#6989=CARTESIAN_POINT('Ctrl Pts',(4.08254682021603,-0.141550205736202,57.7327502279753));
#6990=CARTESIAN_POINT('Ctrl Pts',(4.08668988180302,-0.022057317542035,57.7385565827205));
#6991=CARTESIAN_POINT('Ctrl Pts',(4.08558308906477,0.0976372324661348,57.7443629374657));
#6992=CARTESIAN_POINT('Ctrl Pts',(4.07923019129494,0.217039273929551,57.7501692922109));
#6993=CARTESIAN_POINT('Ctrl Pts',(4.07287670816039,0.336452317260869,57.7559761819616));
#6994=CARTESIAN_POINT('Ctrl Pts',(4.06127618057952,0.45557239121489,57.7617830717123));
#6995=CARTESIAN_POINT('Ctrl Pts',(4.04448438480129,0.573908582527345,57.767589961463));
#6996=CARTESIAN_POINT('Ctrl Pts',(4.02768709176197,0.692283514481301,57.7733987522604));
#6997=CARTESIAN_POINT('Ctrl Pts',(4.00569520778615,0.809873649868988,57.7792075430579));
#6998=CARTESIAN_POINT('Ctrl Pts',(3.97861584184328,0.926197054105497,57.7850163338553));
#6999=CARTESIAN_POINT('Ctrl Pts',(3.95150671879472,1.04264828437166,57.7908315078451));
#7000=CARTESIAN_POINT('Ctrl Pts',(3.91929904742509,1.15782960765195,57.7966466818349));
#7001=CARTESIAN_POINT('Ctrl Pts',(3.8821501965648,1.27127292557966,57.8024618558247));
#7002=CARTESIAN_POINT('Ctrl Pts',(3.84497687931187,1.38479095776354,57.8082808597131));
#7003=CARTESIAN_POINT('Ctrl Pts',(3.80285604487924,1.49656832421439,57.8140998636015));
#7004=CARTESIAN_POINT('Ctrl Pts',(3.7559931034746,1.60615715502912,57.8199188674898));
#7005=CARTESIAN_POINT('Ctrl Pts',(3.70906422052781,1.71590018991832,57.8257460593851));
#7006=CARTESIAN_POINT('Ctrl Pts',(3.65738008911337,1.82344817681897,57.8315732512805));
#7007=CARTESIAN_POINT('Ctrl Pts',(3.60119194136111,1.92837797163206,57.8374004431758));
#7008=CARTESIAN_POINT('Ctrl Pts',(3.5889208588993,1.95129387500959,57.8386730594681));
#7009=CARTESIAN_POINT('Ctrl Pts',(3.57643511834042,1.97408501456058,57.8399456757605));
#7010=CARTESIAN_POINT('Ctrl Pts',(3.56373760472143,1.99674717595753,57.8412182920529));
#7011=CARTESIAN_POINT('Ctrl Pts',(3.50560341422508,2.10050342676706,57.8470448278764));
#7012=CARTESIAN_POINT('Ctrl Pts',(3.44284171951916,2.20188391439461,57.8528713636999));
#7013=CARTESIAN_POINT('Ctrl Pts',(3.37567171959562,2.30044896520709,57.8586978995233));
#7014=CARTESIAN_POINT('Ctrl Pts',(3.30858575265101,2.39889070628534,57.8645171460634));
#7015=CARTESIAN_POINT('Ctrl Pts',(3.23710267775894,2.49452368234317,57.8703363926036));
#7016=CARTESIAN_POINT('Ctrl Pts',(3.16148741778965,2.58693299239809,57.8761556391437));
#7017=CARTESIAN_POINT('Ctrl Pts',(3.0859471094282,2.67925070419134,57.881969117511));
#7018=CARTESIAN_POINT('Ctrl Pts',(3.00628302140393,2.76835079313342,57.8877825958784));
#7019=CARTESIAN_POINT('Ctrl Pts',(2.92280283701968,2.85384802957511,57.8935960742457));
#7020=CARTESIAN_POINT('Ctrl Pts',(2.83671897618786,2.94201185261453,57.8995908700935));
#7021=CARTESIAN_POINT('Ctrl Pts',(2.74657732364043,3.02634403411968,57.9055856659414));
#7022=CARTESIAN_POINT('Ctrl Pts',(2.65275981030388,3.10645946196575,57.9115804617892));
#7023=CARTESIAN_POINT('Ctrl Pts',(2.56188052521919,3.18406579097584,57.9173875093382));
#7024=CARTESIAN_POINT('Ctrl Pts',(2.46755252109992,3.25771526527268,57.9231945568873));
#7025=CARTESIAN_POINT('Ctrl Pts',(2.37015921714246,3.32709637452759,57.9290016044364));
#7026=CARTESIAN_POINT('Ctrl Pts',(2.27277984248461,3.39646756081842,57.9348078214549));
#7027=CARTESIAN_POINT('Ctrl Pts',(2.17233637196149,3.46157135960054,57.9406140384735));
#7028=CARTESIAN_POINT('Ctrl Pts',(2.06924303801145,3.52213830643278,57.9464202554921));
#7029=CARTESIAN_POINT('Ctrl Pts',(1.96614019381764,3.58271084049754,57.9522270081277));
#7030=CARTESIAN_POINT('Ctrl Pts',(1.86038735182497,3.63874548390321,57.9580337607633));
#7031=CARTESIAN_POINT('Ctrl Pts',(1.75242472752776,3.69001796396024,57.9638405133988));
#7032=CARTESIAN_POINT('Ctrl Pts',(1.64442674365151,3.74130723661862,57.9696491678438));
#7033=CARTESIAN_POINT('Ctrl Pts',(1.53421790628161,3.78783106914006,57.9754578222887));
#7034=CARTESIAN_POINT('Ctrl Pts',(1.42225925843097,3.82941295785756,57.9812664767336));
#7035=CARTESIAN_POINT('Ctrl Pts',(1.31017754328291,3.87104055426057,57.9870815161735));
#7036=CARTESIAN_POINT('Ctrl Pts',(1.19634256096252,3.90771522184106,57.9928965556134));
#7037=CARTESIAN_POINT('Ctrl Pts',(1.08123153847864,3.93931001067434,57.9987115950533));
#7038=CARTESIAN_POINT('Ctrl Pts',(0.966044683761101,3.97092561335636,58.0045304652943));
#7039=CARTESIAN_POINT('Ctrl Pts',(0.849580511417873,3.99745458213876,58.0103493355353));
#7040=CARTESIAN_POINT('Ctrl Pts',(0.732325876425768,4.01882119665919,58.0161682057763));
#7041=CARTESIAN_POINT('Ctrl Pts',(0.614906200508081,4.04021788560558,58.0219952663266));
#7042=CARTESIAN_POINT('Ctrl Pts',(0.496694243903159,4.05643766298363,58.0278223268769));
#7043=CARTESIAN_POINT('Ctrl Pts',(0.378181514051322,4.06745666755404,58.0336493874272));
#7044=CARTESIAN_POINT('Ctrl Pts',(0.352271913713808,4.06986567462774,58.0349233164827));
#7045=CARTESIAN_POINT('Ctrl Pts',(0.326347934062307,4.07202630341459,58.0361972455381));
#7046=CARTESIAN_POINT('Ctrl Pts',(0.300414697640057,4.07393863594456,58.0374711745936));
#7047=CARTESIAN_POINT('Ctrl Pts',(0.181800445423052,4.08268532260331,58.0432979113661));
#7048=CARTESIAN_POINT('Ctrl Pts',(0.0626151280544477,4.08626138513636,58.0491246481386));
#7049=CARTESIAN_POINT('Ctrl Pts',(-0.0566535826103796,4.08460712573161,
58.0549513849111));
#7050=CARTESIAN_POINT('Ctrl Pts',(-0.175773077047609,4.08295493595891,58.0607708318951));
#7051=CARTESIAN_POINT('Ctrl Pts',(-0.294975353010617,4.07608544540713,58.0665902788791));
#7052=CARTESIAN_POINT('Ctrl Pts',(-0.413768179883462,4.06399075950179,58.072409725863));
#7053=CARTESIAN_POINT('Ctrl Pts',(-0.53244324554876,4.05190806324982,58.0782234039372));
#7054=CARTESIAN_POINT('Ctrl Pts',(-0.650709266199974,4.03461051768562,58.0840370820113));
#7055=CARTESIAN_POINT('Ctrl Pts',(-0.768075172731697,4.0121422618139,58.0898507600855));
#7056=CARTESIAN_POINT('Ctrl Pts',(-0.889095948495576,3.98897432628638,58.0958454807959));
#7057=CARTESIAN_POINT('Ctrl Pts',(-1.00915919048552,3.96030837484129,58.1018402015062));
#7058=CARTESIAN_POINT('Ctrl Pts',(-1.12773304273466,3.92625052490597,58.1078349222166));
#7059=CARTESIAN_POINT('Ctrl Pts',(-1.24259866302598,3.89325778675668,58.1136421663923));
#7060=CARTESIAN_POINT('Ctrl Pts',(-1.35606624184807,3.85520549333451,58.1194494105681));
#7061=CARTESIAN_POINT('Ctrl Pts',(-1.46766442048272,3.81224161732295,58.1252566547438));
#7062=CARTESIAN_POINT('Ctrl Pts',(-1.57924661033535,3.76928389678863,58.1310630669099));
#7063=CARTESIAN_POINT('Ctrl Pts',(-1.68895955219553,3.7214161396405,58.136869479076));
#7064=CARTESIAN_POINT('Ctrl Pts',(-1.79634995928534,3.66883521349427,58.1426758912421));
#7065=CARTESIAN_POINT('Ctrl Pts',(-1.90375024145776,3.61624945227009,58.1484828373367));
#7066=CARTESIAN_POINT('Ctrl Pts',(-2.0088271979684,3.55894983967916,58.1542897834313));
#7067=CARTESIAN_POINT('Ctrl Pts',(-2.11115090204654,3.49717984507347,58.1600967295259));
#7068=CARTESIAN_POINT('Ctrl Pts',(-2.21350808428251,3.43538964062836,58.1659055755308));
#7069=CARTESIAN_POINT('Ctrl Pts',(-2.31310987362147,3.36912635593796,58.1717144215357));
#7070=CARTESIAN_POINT('Ctrl Pts',(-2.4095546966394,3.29867718394859,58.1775232675406));
#7071=CARTESIAN_POINT('Ctrl Pts',(-2.50610546819611,3.22815062069449,58.1833384947977));
#7072=CARTESIAN_POINT('Ctrl Pts',(-2.59949202165173,3.15342923237338,58.1891537220549));
#7073=CARTESIAN_POINT('Ctrl Pts',(-2.6893451871139,3.07484104703761,58.1949689493121));
#7074=CARTESIAN_POINT('Ctrl Pts',(-2.77925751311814,2.99620111817537,58.2007880053937));
#7075=CARTESIAN_POINT('Ctrl Pts',(-2.86563152368462,2.91368960285899,58.2066070614753));
#7076=CARTESIAN_POINT('Ctrl Pts',(-2.94813546623174,2.82767082114354,58.2124261175569));
#7077=CARTESIAN_POINT('Ctrl Pts',(-3.03075547280752,2.74153103083094,58.218253359709));
#7078=CARTESIAN_POINT('Ctrl Pts',(-3.10949427745213,2.6518744321804,58.2240806018611));
#7079=CARTESIAN_POINT('Ctrl Pts',(-3.18406081488101,2.55909783461659,58.2299078440133));
#7080=CARTESIAN_POINT('Ctrl Pts',(-3.20033848626719,2.53884495685741,58.2311799150536));
#7081=CARTESIAN_POINT('Ctrl Pts',(-3.21641750014398,2.51844350545445,58.2324519860939));
#7082=CARTESIAN_POINT('Ctrl Pts',(-3.23229511105798,2.49789777913963,58.2337240571342));
#7083=CARTESIAN_POINT('Ctrl Pts',(-3.30497237932344,2.40385294637613,58.2395467623731));
#7084=CARTESIAN_POINT('Ctrl Pts',(-3.37366200923957,2.30647812772046,58.245369467612));
#7085=CARTESIAN_POINT('Ctrl Pts',(-3.43804411656929,2.20614542868852,58.2511921728509));
#7086=CARTESIAN_POINT('Ctrl Pts',(-3.50234761952142,2.10593522625831,58.2570077691252));
#7087=CARTESIAN_POINT('Ctrl Pts',(-3.56235383823522,2.00277466344739,58.2628233653995));
#7088=CARTESIAN_POINT('Ctrl Pts',(-3.61778331695694,1.89706849416356,58.2686389616738));
#7089=CARTESIAN_POINT('Ctrl Pts',(-3.67315817556485,1.7914664875587,58.2744488272695));
#7090=CARTESIAN_POINT('Ctrl Pts',(-3.72396507498049,1.68332422195153,58.2802586928651));
#7091=CARTESIAN_POINT('Ctrl Pts',(-3.76996840064677,1.57307446045153,58.2860685584607));
#7092=CARTESIAN_POINT('Ctrl Pts',(-3.8159372266017,1.46290737960325,58.2918740670086));
#7093=CARTESIAN_POINT('Ctrl Pts',(-3.85710948865528,1.35063632196236,58.2976795755566));
#7094=CARTESIAN_POINT('Ctrl Pts',(-3.89329627824057,1.23671706135161,58.3034850841045));
#7095=CARTESIAN_POINT('Ctrl Pts',(-3.92946682042483,1.12284894901713,58.309287986054));
#7096=CARTESIAN_POINT('Ctrl Pts',(-3.96065621842049,1.00733449342105,58.3150908880036));
#7097=CARTESIAN_POINT('Ctrl Pts',(-3.98672452292116,0.890647280543241,58.3208937899532));
#7098=CARTESIAN_POINT('Ctrl Pts',(-4.01278586190416,0.773991246787297,58.3266951413525));
#7099=CARTESIAN_POINT('Ctrl Pts',(-4.03372874412109,0.656163477712639,58.3324964927518));
#7100=CARTESIAN_POINT('Ctrl Pts',(-4.04946387960724,0.537649781694597,58.3382978441512));
#7101=CARTESIAN_POINT('Ctrl Pts',(-4.06520193070151,0.419114125935964,58.3441002704994));
#7102=CARTESIAN_POINT('Ctrl Pts',(-4.07573025238781,0.299892693576237,58.3499026968477));
#7103=CARTESIAN_POINT('Ctrl Pts',(-4.08101122655926,0.180478166815966,58.3557051231959));
#7104=CARTESIAN_POINT('Ctrl Pts',(-4.08371429004001,0.119355912497564,58.3586750916625));
#7105=CARTESIAN_POINT('Ctrl Pts',(-4.08504344081981,0.0581831381100053,
58.361645060129));
#7106=CARTESIAN_POINT('Ctrl Pts',(-4.08499891745933,-0.00297394621324721,
58.3646150285955));
#7107=CARTESIAN_POINT('Ctrl Pts',(-4.08499891745875,-0.00297394700961363,
58.3646150286342));
#7108=CARTESIAN_POINT('Ctrl Pts',(-4.08489785974511,-0.14178632311568,58.3713561672016));
#7109=CARTESIAN_POINT('Ctrl Pts',(-4.07771738177627,-0.28031599001206,58.378097305769));
#7110=CARTESIAN_POINT('Ctrl Pts',(-4.06356739568884,-0.417905516468299,
58.3848384443363));
#7111=CARTESIAN_POINT('Ctrl Pts',(-4.0493356015318,-0.556290516042897,58.3916185567607));
#7112=CARTESIAN_POINT('Ctrl Pts',(-4.02805358644635,-0.693724362004736,
58.398398669185));
#7113=CARTESIAN_POINT('Ctrl Pts',(-3.99988246908372,-0.829557251500295,
58.4051787816093));
#7114=CARTESIAN_POINT('Ctrl Pts',(-3.97153196598098,-0.966255086574672,
58.4120020678797));
#7115=CARTESIAN_POINT('Ctrl Pts',(-3.93620442598652,-1.10133140441473,58.4188253541501));
#7116=CARTESIAN_POINT('Ctrl Pts',(-3.8941124171469,-1.23414483859161,58.4256486404205));
#7117=CARTESIAN_POINT('Ctrl Pts',(-3.88521216960954,-1.26222789932092,58.4270914068386));
#7118=CARTESIAN_POINT('Ctrl Pts',(-3.87600965127867,-1.29020986379836,58.4285341732567));
#7119=CARTESIAN_POINT('Ctrl Pts',(-3.86650714144293,-1.31808479437811,58.4299769396749));
#7120=CARTESIAN_POINT('Ctrl Pts',(-3.82814300626743,-1.4306232314074,58.4358017677306));
#7121=CARTESIAN_POINT('Ctrl Pts',(-3.78480033911442,-1.54166471466195,58.4416265957864));
#7122=CARTESIAN_POINT('Ctrl Pts',(-3.73661489342043,-1.65073745285815,58.4474514238421));
#7123=CARTESIAN_POINT('Ctrl Pts',(-3.68848594587143,-1.75968230166186,58.4532694222012));
#7124=CARTESIAN_POINT('Ctrl Pts',(-3.63552567337794,-1.86666262561796,58.4590874205602));
#7125=CARTESIAN_POINT('Ctrl Pts',(-3.57791929970426,-1.97122258631636,58.4649054189193));
#7126=CARTESIAN_POINT('Ctrl Pts',(-3.52036690180499,-2.07568457686856,58.470717965955));
#7127=CARTESIAN_POINT('Ctrl Pts',(-3.45817725636424,-2.17773035931255,58.4765305129908));
#7128=CARTESIAN_POINT('Ctrl Pts',(-3.39158304093662,-2.27692544375769,58.4823430600265));
#7129=CARTESIAN_POINT('Ctrl Pts',(-3.32503554001746,-2.37605094483762,58.4881515296769));
#7130=CARTESIAN_POINT('Ctrl Pts',(-3.25408984261685,-2.47232938875589,58.4939599993273));
#7131=CARTESIAN_POINT('Ctrl Pts',(-3.17902346303331,-2.56535276745396,58.4997684689777));
#7132=CARTESIAN_POINT('Ctrl Pts',(-3.10398684139246,-2.65833926966502,58.5055746360247));
#7133=CARTESIAN_POINT('Ctrl Pts',(-3.02483304191969,-2.74807295587033,58.5113808030716));
#7134=CARTESIAN_POINT('Ctrl Pts',(-2.94188130048249,-2.83417702585274,58.5171869701185));
#7135=CARTESIAN_POINT('Ctrl Pts',(-2.85894811056118,-2.92026183932533,58.5229918386611));
#7136=CARTESIAN_POINT('Ctrl Pts',(-2.77221895421885,-3.00271836067829,58.5287967072036));
#7137=CARTESIAN_POINT('Ctrl Pts',(-2.6820510311498,-3.08120548914029,58.5346015757461));
#7138=CARTESIAN_POINT('Ctrl Pts',(-2.59186613596601,-3.15970739106613,58.5404075369266));
#7139=CARTESIAN_POINT('Ctrl Pts',(-2.49824148995269,-3.2342381411996,58.5462134981071));
#7140=CARTESIAN_POINT('Ctrl Pts',(-2.40156828346354,-3.30449614614119,58.5520194592876));
#7141=CARTESIAN_POINT('Ctrl Pts',(-2.37244521715133,-3.32566156116347,58.5537685208798));
#7142=CARTESIAN_POINT('Ctrl Pts',(-2.3430456986581,-3.34643949841264,58.555517582472));
#7143=CARTESIAN_POINT('Ctrl Pts',(-2.31338095599002,-3.36682247118299,58.5572666440642));
#7144=CARTESIAN_POINT('',(-4.08499950778543,0.00200534106489888,58.2603849714451));
#7145=CARTESIAN_POINT('Ctrl Pts',(-4.08499950778543,0.00200534106489888,
58.2603849714451));
#7146=CARTESIAN_POINT('Ctrl Pts',(-4.08505725975092,-0.115638861568439,
58.2661416094535));
#7147=CARTESIAN_POINT('Ctrl Pts',(-4.0800287331631,-0.233480689917119,58.271898247462));
#7148=CARTESIAN_POINT('Ctrl Pts',(-4.06988904518043,-0.351038687213156,
58.2776548854704));
#7149=CARTESIAN_POINT('Ctrl Pts',(-4.05976110079072,-0.468460531082006,
58.2834048562506));
#7150=CARTESIAN_POINT('Ctrl Pts',(-4.04453380004621,-0.585598784051002,
58.2891548270309));
#7151=CARTESIAN_POINT('Ctrl Pts',(-4.0242342774865,-0.70197113893855,58.2949047978111));
#7152=CARTESIAN_POINT('Ctrl Pts',(-4.00305659713254,-0.823377764468657,
58.3009035124543));
#7153=CARTESIAN_POINT('Ctrl Pts',(-3.97635795742803,-0.943950276068998,
58.3069022270975));
#7154=CARTESIAN_POINT('Ctrl Pts',(-3.94422954554652,-1.06314547077899,58.3129009417407));
#7155=CARTESIAN_POINT('Ctrl Pts',(-3.91347786077154,-1.17723305991762,58.3186426068577));
#7156=CARTESIAN_POINT('Ctrl Pts',(-3.87775224096607,-1.2900584790373,58.3243842719746));
#7157=CARTESIAN_POINT('Ctrl Pts',(-3.83718484198393,-1.40115576880259,58.3301259370915));
#7158=CARTESIAN_POINT('Ctrl Pts',(-3.79662751282597,-1.51222548149362,58.3358661769862));
#7159=CARTESIAN_POINT('Ctrl Pts',(-3.75123093677261,-1.6215675247441,58.341606416881));
#7160=CARTESIAN_POINT('Ctrl Pts',(-3.70117666229399,-1.72873257460207,58.3473466567757));
#7161=CARTESIAN_POINT('Ctrl Pts',(-3.65112234603474,-1.83589771391142,58.3530869014618));
#7162=CARTESIAN_POINT('Ctrl Pts',(-3.59641050129044,-1.94088547743368,58.3588271461479));
#7163=CARTESIAN_POINT('Ctrl Pts',(-3.53726987536132,-2.04326866291765,58.3645673908341));
#7164=CARTESIAN_POINT('Ctrl Pts',(-3.47811446962349,-2.14567743494004,58.3703090700623));
#7165=CARTESIAN_POINT('Ctrl Pts',(-3.41452829257581,-2.24547997336317,58.3760507492905));
#7166=CARTESIAN_POINT('Ctrl Pts',(-3.346784472902,-2.34227639102265,58.3817924285188));
#7167=CARTESIAN_POINT('Ctrl Pts',(-3.27897005430982,-2.43917368463542,58.3875400914123));
#7168=CARTESIAN_POINT('Ctrl Pts',(-3.20698958588826,-2.53305826224156,58.3932877543059));
#7169=CARTESIAN_POINT('Ctrl Pts',(-3.13115769800021,-2.62356179082064,58.3990354171994));
#7170=CARTESIAN_POINT('Ctrl Pts',(-3.05527922424442,-2.7141209185089,58.4047866110596));
#7171=CARTESIAN_POINT('Ctrl Pts',(-2.97554490342206,-2.80129455509581,58.4105378049197));
#7172=CARTESIAN_POINT('Ctrl Pts',(-2.89230634090281,-2.88475112104552,58.4162889987798));
#7173=CARTESIAN_POINT('Ctrl Pts',(-2.80894935200499,-2.96832642353483,58.4220483750622));
#7174=CARTESIAN_POINT('Ctrl Pts',(-2.72207847987514,-3.0481738209203,58.4278077513445));
#7175=CARTESIAN_POINT('Ctrl Pts',(-2.6320784946416,-3.12400188829091,58.4335671276269));
#7176=CARTESIAN_POINT('Ctrl Pts',(-2.60443580996555,-3.14729179606681,58.4353360681671));
#7177=CARTESIAN_POINT('Ctrl Pts',(-2.57649814378481,-3.17020284775017,58.4371050087074));
#7178=CARTESIAN_POINT('Ctrl Pts',(-2.54827716476554,-3.19272743771442,58.4388739492477));
#7179=CARTESIAN_POINT('Ctrl Pts',(-2.47218313370533,-3.25346193056061,58.4436436567877));
#7180=CARTESIAN_POINT('Ctrl Pts',(-2.3938175737227,-3.31155358153415,58.4484133643277));
#7181=CARTESIAN_POINT('Ctrl Pts',(-2.31338095599002,-3.36682247118298,58.4531830718678));
#7182=CARTESIAN_POINT('Ctrl Pts',(-2.31338095599003,-3.36682247118298,57.2030181077425));
#7183=CARTESIAN_POINT('Ctrl Pts',(-2.21482775942375,-3.43453946251228,57.2088328619545));
#7184=CARTESIAN_POINT('Ctrl Pts',(-2.11336204419633,-3.4978821844165,57.2146476161665));
#7185=CARTESIAN_POINT('Ctrl Pts',(-2.00941524034814,-3.5566100983741,57.2204623703784));
#7186=CARTESIAN_POINT('Ctrl Pts',(-1.90540266148345,-3.61537517393135,57.2262808040259));
#7187=CARTESIAN_POINT('Ctrl Pts',(-1.79890622990321,-3.66951944100108,57.2320992376733));
#7188=CARTESIAN_POINT('Ctrl Pts',(-1.69037935165581,-3.71884964034521,57.2379176713207));
#7189=CARTESIAN_POINT('Ctrl Pts',(-1.58169626272958,-3.76825084425568,57.2437444798655));
#7190=CARTESIAN_POINT('Ctrl Pts',(-1.47097727010335,-3.81282399589916,57.2495712884103));
#7191=CARTESIAN_POINT('Ctrl Pts',(-1.35869317216081,-3.85242493293816,57.2553980969551));
#7192=CARTESIAN_POINT('Ctrl Pts',(-1.32041886367163,-3.86592371423012,57.257384282638));
#7193=CARTESIAN_POINT('Ctrl Pts',(-1.28196280673188,-3.87884519555452,57.2593704683209));
#7194=CARTESIAN_POINT('Ctrl Pts',(-1.24334393029046,-3.89118502143111,57.2613566540038));
#7195=CARTESIAN_POINT('Ctrl Pts',(-1.1300522447437,-3.92738492680728,57.2671832948738));
#7196=CARTESIAN_POINT('Ctrl Pts',(-1.0149980085889,-3.95869061724581,57.2730099357437));
#7197=CARTESIAN_POINT('Ctrl Pts',(-0.898641461870173,-3.98493017793384,
57.2788365766136));
#7198=CARTESIAN_POINT('Ctrl Pts',(-0.782430478763564,-4.01113691257692,
57.2846559282771));
#7199=CARTESIAN_POINT('Ctrl Pts',(-0.664920820055686,-4.03229003468466,
57.2904752799406));
#7200=CARTESIAN_POINT('Ctrl Pts',(-0.546589254619076,-4.0482669362006,57.2962946316041));
#7201=CARTESIAN_POINT('Ctrl Pts',(-0.428374981075478,-4.0642280011896,57.3021082150453));
#7202=CARTESIAN_POINT('Ctrl Pts',(-0.309340823453885,-4.07502299865065,
57.3079217984865));
#7203=CARTESIAN_POINT('Ctrl Pts',(-0.189974570917122,-4.08058018698381,
57.3137353819277));
#7204=CARTESIAN_POINT('Ctrl Pts',(-0.0668884195559605,-4.08631055808772,
57.3197301383701));
#7205=CARTESIAN_POINT('Ctrl Pts',(0.0565504337260151,-4.08647121584311,
57.3257248948125));
#7206=CARTESIAN_POINT('Ctrl Pts',(0.179800033968628,-4.08104115977588,57.3317196512548));
#7207=CARTESIAN_POINT('Ctrl Pts',(0.299192564565407,-4.07578103614163,57.3375268030878));
#7208=CARTESIAN_POINT('Ctrl Pts',(0.418407073487605,-4.06527491997163,57.3433339549208));
#7209=CARTESIAN_POINT('Ctrl Pts',(0.53695069273696,-4.04955663666645,57.3491411067538));
#7210=CARTESIAN_POINT('Ctrl Pts',(0.655477348374434,-4.03384060265026,57.3549474275824));
#7211=CARTESIAN_POINT('Ctrl Pts',(0.773332901105097,-4.01291393846466,57.360753748411));
#7212=CARTESIAN_POINT('Ctrl Pts',(0.890030639190593,-3.98686223254604,57.3665600692396));
#7213=CARTESIAN_POINT('Ctrl Pts',(1.00673913052452,-3.96080812606276,57.3723669250983));
#7214=CARTESIAN_POINT('Ctrl Pts',(1.12228919706243,-3.92962812775035,57.3781737809571));
#7215=CARTESIAN_POINT('Ctrl Pts',(1.2362059608438,-3.89345859389493,57.3839806368159));
#7216=CARTESIAN_POINT('Ctrl Pts',(1.35016001988649,-3.8572772184793,57.3897893937838));
#7217=CARTESIAN_POINT('Ctrl Pts',(1.4624793242187,-3.81610318208682,57.3955981507518));
#7218=CARTESIAN_POINT('Ctrl Pts',(1.57270635715591,-3.77012197603226,57.4014069077197));
#7219=CARTESIAN_POINT('Ctrl Pts',(1.68305452258816,-3.72409023955819,57.4072220481419));
#7220=CARTESIAN_POINT('Ctrl Pts',(1.79130545065884,-3.67324094598739,57.4130371885642));
#7221=CARTESIAN_POINT('Ctrl Pts',(1.89702359857503,-3.61780685864371,57.4188523289864));
#7222=CARTESIAN_POINT('Ctrl Pts',(2.00281137541744,-3.56233626086114,57.4246712994226));
#7223=CARTESIAN_POINT('Ctrl Pts',(2.10606269816485,-3.50227505996777,57.4304902698588));
#7224=CARTESIAN_POINT('Ctrl Pts',(2.20636993423211,-3.43790004411364,57.436309240295));
#7225=CARTESIAN_POINT('Ctrl Pts',(2.30681832211101,-3.37343444007796,57.4421363991556));
#7226=CARTESIAN_POINT('Ctrl Pts',(2.40431402286169,-3.30464313994416,57.4479635580161));
#7227=CARTESIAN_POINT('Ctrl Pts',(2.49848138145923,-3.23184402261334,57.4537907168767));
#7228=CARTESIAN_POINT('Ctrl Pts',(2.51905219304851,-3.21594109246024,57.455063656766));
#7229=CARTESIAN_POINT('Ctrl Pts',(2.53946431287178,-3.19984705051002,57.4563365966552));
#7230=CARTESIAN_POINT('Ctrl Pts',(2.55971406016711,-3.1835654430501,57.4576095365444));
#7231=CARTESIAN_POINT('Ctrl Pts',(2.65240351183048,-3.10903941338426,57.4634361821125));
#7232=CARTESIAN_POINT('Ctrl Pts',(2.74198304034683,-3.03034344430009,57.4692628276806));
#7233=CARTESIAN_POINT('Ctrl Pts',(2.82805536971624,-2.94776658265527,57.4750894732486));
#7234=CARTESIAN_POINT('Ctrl Pts',(2.91402002204039,-2.8652930252028,57.4809088296451));
#7235=CARTESIAN_POINT('Ctrl Pts',(2.99648591045966,-2.77894851193904,57.4867281860416));
#7236=CARTESIAN_POINT('Ctrl Pts',(3.07508776726771,-2.68906307542246,57.4925475424381));
#7237=CARTESIAN_POINT('Ctrl Pts',(3.15361171327372,-2.59926673408423,57.498361130641));
#7238=CARTESIAN_POINT('Ctrl Pts',(3.22827898041083,-2.50593675729864,57.5041747188439));
#7239=CARTESIAN_POINT('Ctrl Pts',(3.29876064887406,-2.40944042911212,57.5099883070468));
#7240=CARTESIAN_POINT('Ctrl Pts',(3.37143870867106,-2.30993702541801,57.5159830617151));
#7241=CARTESIAN_POINT('Ctrl Pts',(3.43966570994165,-2.20706700003783,57.5219778163833));
#7242=CARTESIAN_POINT('Ctrl Pts',(3.50312517674191,-2.10127080503133,57.5279725710516));
#7243=CARTESIAN_POINT('Ctrl Pts',(3.56459876224643,-1.99878536404491,57.5337797276865));
#7244=CARTESIAN_POINT('Ctrl Pts',(3.62159852602436,-1.89355453901573,57.5395868843215));
#7245=CARTESIAN_POINT('Ctrl Pts',(3.67388079862009,-1.78600808439676,57.5453940409564));
#7246=CARTESIAN_POINT('Ctrl Pts',(3.72615558967732,-1.67847701956292,57.5512003665933));
#7247=CARTESIAN_POINT('Ctrl Pts',(3.77371405387893,-1.56863135083147,57.5570066922302));
#7248=CARTESIAN_POINT('Ctrl Pts',(3.81635909262693,-1.45692425201992,57.5628130178671));
#7249=CARTESIAN_POINT('Ctrl Pts',(3.8590080609555,-1.34520685981764,57.5686198785351));
#7250=CARTESIAN_POINT('Ctrl Pts',(3.89674255819498,-1.23162807751074,57.5744267392031));
#7251=CARTESIAN_POINT('Ctrl Pts',(3.9294143584382,-1.11665921377103,57.5802335998712));
#7252=CARTESIAN_POINT('Ctrl Pts',(3.96209685508355,-1.00165271044029,57.5860423616441));
#7253=CARTESIAN_POINT('Ctrl Pts',(3.9897132469091,-0.885255612638544,57.5918511234169));
#7254=CARTESIAN_POINT('Ctrl Pts',(4.01216586793536,-0.767951852771041,57.5976598851898));
#7255=CARTESIAN_POINT('Ctrl Pts',(4.03464316282455,-0.650519184261271,57.6034750303863));
#7256=CARTESIAN_POINT('Ctrl Pts',(4.05194528354712,-0.532178265681518,57.6092901755828));
#7257=CARTESIAN_POINT('Ctrl Pts',(4.06402611460516,-0.41342077815135,57.6151053207793));
#7258=CARTESIAN_POINT('Ctrl Pts',(4.0761149024035,-0.294585073942095,57.6209242959772));
#7259=CARTESIAN_POINT('Ctrl Pts',(4.08297552839478,-0.17533266054159,57.6267432711751));
#7260=CARTESIAN_POINT('Ctrl Pts',(4.08461399380378,-0.0561562251430488,
57.632562246373));
#7261=CARTESIAN_POINT('Ctrl Pts',(4.08625476483559,0.0631879134646265,57.6383894099415));
#7262=CARTESIAN_POINT('Ctrl Pts',(4.08265872117685,0.18245545458868,57.64421657351));
#7263=CARTESIAN_POINT('Ctrl Pts',(4.07388377719373,0.301157716018913,57.6500437370785));
#7264=CARTESIAN_POINT('Ctrl Pts',(4.07196696579233,0.327087208961452,57.6513166310807));
#7265=CARTESIAN_POINT('Ctrl Pts',(4.06980322869673,0.352989764867805,57.6525895250829));
#7266=CARTESIAN_POINT('Ctrl Pts',(4.06739349327876,0.378860357959995,57.6538624190851));
#7267=CARTESIAN_POINT('Ctrl Pts',(4.05636301354315,0.497282094522663,57.6596890469349));
#7268=CARTESIAN_POINT('Ctrl Pts',(4.040138935536,0.615410174995458,57.6655156747847));
#7269=CARTESIAN_POINT('Ctrl Pts',(4.01874319674208,0.732753791282729,57.6713423026346));
#7270=CARTESIAN_POINT('Ctrl Pts',(3.99737422432736,0.849950609006079,57.6771616412885));
#7271=CARTESIAN_POINT('Ctrl Pts',(3.97084653240757,0.966364516798952,57.6829809799425));
#7272=CARTESIAN_POINT('Ctrl Pts',(3.93923390095314,1.08150879496263,57.6888003185965));
#7273=CARTESIAN_POINT('Ctrl Pts',(3.9076526043076,1.19653894077522,57.6946138890541));
#7274=CARTESIAN_POINT('Ctrl Pts',(3.87099650278965,1.31030156956013,57.7004274595118));
#7275=CARTESIAN_POINT('Ctrl Pts',(3.82939049808816,1.42231972957986,57.7062410299694));
#7276=CARTESIAN_POINT('Ctrl Pts',(3.7864877639697,1.53782914631539,57.7122357912884));
#7277=CARTESIAN_POINT('Ctrl Pts',(3.73832160506255,1.65148313922527,57.7182305526075));
#7278=CARTESIAN_POINT('Ctrl Pts',(3.68508481835105,1.76277476767698,57.7242253139265));
#7279=CARTESIAN_POINT('Ctrl Pts',(3.63351422134615,1.87058322260879,57.7300324529223));
#7280=CARTESIAN_POINT('Ctrl Pts',(3.57718584971938,1.97617458602078,57.7358395919181));
#7281=CARTESIAN_POINT('Ctrl Pts',(3.51632373812308,2.0791085514499,57.7416467309139));
#7282=CARTESIAN_POINT('Ctrl Pts',(3.45547033512344,2.18202778833342,57.7474530389817));
#7283=CARTESIAN_POINT('Ctrl Pts',(3.39008468984156,2.2822900325073,57.7532593470495));
#7284=CARTESIAN_POINT('Ctrl Pts',(3.3204360607725,2.3794809027016,57.7590656551173));
#7285=CARTESIAN_POINT('Ctrl Pts',(3.2507810127535,2.47668073019108,57.7648724983056));
#7286=CARTESIAN_POINT('Ctrl Pts',(3.176862437355,2.57080828940431,57.7706793414938));
#7287=CARTESIAN_POINT('Ctrl Pts',(3.09899167892451,2.66147995933779,57.776486184682));
#7288=CARTESIAN_POINT('Ctrl Pts',(3.02109542489957,2.75218131600055,57.7822949290834));
#7289=CARTESIAN_POINT('Ctrl Pts',(2.93924467991378,2.83942422385016,57.7881036734849));
#7290=CARTESIAN_POINT('Ctrl Pts',(2.85378920812506,2.92286026959705,57.7939124178864));
#7291=CARTESIAN_POINT('Ctrl Pts',(2.76823982283651,3.00638800954332,57.7997275459577));
#7292=CARTESIAN_POINT('Ctrl Pts',(2.67907809544267,3.08610025169248,57.8055426740289));
#7293=CARTESIAN_POINT('Ctrl Pts',(2.5866886901372,3.16168730590429,57.8113578021002));
#7294=CARTESIAN_POINT('Ctrl Pts',(2.49423843267743,3.23732414542503,57.8171767602976));
#7295=CARTESIAN_POINT('Ctrl Pts',(2.39855658930083,3.30883014224941,57.822995718495));
#7296=CARTESIAN_POINT('Ctrl Pts',(2.3000574125857,3.37593852118334,57.8288146766923));
#7297=CARTESIAN_POINT('Ctrl Pts',(2.20141962377296,3.44314133779159,57.8346418235673));
#7298=CARTESIAN_POINT('Ctrl Pts',(2.09995693434531,3.50593397156601,57.8404689704423));
#7299=CARTESIAN_POINT('Ctrl Pts',(1.99610889330301,3.56409515670901,57.8462961173172));
#7300=CARTESIAN_POINT('Ctrl Pts',(1.97342112875701,3.57680167732314,57.8475691787534));
#7301=CARTESIAN_POINT('Ctrl Pts',(1.95061958949687,3.58928732321926,57.8488422401896));
#7302=CARTESIAN_POINT('Ctrl Pts',(1.92770898090545,3.60155009474205,57.8501153016258));
#7303=CARTESIAN_POINT('Ctrl Pts',(1.82284989761685,3.65767531617936,57.8559419497759));
#7304=CARTESIAN_POINT('Ctrl Pts',(1.71537077353199,3.70930660615456,57.8617685979261));
#7305=CARTESIAN_POINT('Ctrl Pts',(1.60569308936343,3.75619151572048,57.8675952460762));
#7306=CARTESIAN_POINT('Ctrl Pts',(1.49615261469705,3.8030177711021,57.8734146049451));
#7307=CARTESIAN_POINT('Ctrl Pts',(1.38441942247576,3.84510929777986,57.879233963814));
#7308=CARTESIAN_POINT('Ctrl Pts',(1.2709401812882,3.88225914328077,57.8850533226828));
#7309=CARTESIAN_POINT('Ctrl Pts',(1.1575734237696,3.91937216485794,57.890866913247));
#7310=CARTESIAN_POINT('Ctrl Pts',(1.04246444587559,3.95155312403871,57.8966805038112));
#7311=CARTESIAN_POINT('Ctrl Pts',(0.926079969253856,3.97864309665328,57.9024940943754));
#7312=CARTESIAN_POINT('Ctrl Pts',(0.806068718211667,4.00657724731101,57.9084888481167));
#7313=CARTESIAN_POINT('Ctrl Pts',(0.684701578090561,4.02909774990616,57.914483601858));
#7314=CARTESIAN_POINT('Ctrl Pts',(0.562507729921121,4.0460857694541,57.9204783555993));
#7315=CARTESIAN_POINT('Ctrl Pts',(0.444137718385236,4.06254217949426,57.9262855143077));
#7316=CARTESIAN_POINT('Ctrl Pts',(0.324992401423549,4.07380714096769,57.9320926730161));
#7317=CARTESIAN_POINT('Ctrl Pts',(0.205562620331488,4.07982462970192,57.9378998317245));
#7318=CARTESIAN_POINT('Ctrl Pts',(0.0861499317634045,4.08584125722659,57.9437061593253));
#7319=CARTESIAN_POINT('Ctrl Pts',(-0.0335467327789725,4.08661188510273,
57.9495124869261));
#7320=CARTESIAN_POINT('Ctrl Pts',(-0.153033208793098,4.08213251095631,57.9553188145269));
#7321=CARTESIAN_POINT('Ctrl Pts',(-0.272530692746211,4.07765272413828,57.9611256770477));
#7322=CARTESIAN_POINT('Ctrl Pts',(-0.391817542131322,4.06792198892883,57.9669325395684));
#7323=CARTESIAN_POINT('Ctrl Pts',(-0.51040203308808,4.05298837459714,57.9727394020892));
#7324=CARTESIAN_POINT('Ctrl Pts',(-0.629025345035767,4.03804987144987,57.9785481656018));
#7325=CARTESIAN_POINT('Ctrl Pts',(-0.746945436868593,4.01790515262829,57.9843569291145));
#7326=CARTESIAN_POINT('Ctrl Pts',(-0.863678757197371,3.99265375463062,57.9901656926271));
#7327=CARTESIAN_POINT('Ctrl Pts',(-0.980540355762733,3.96737460787366,57.9959808393896));
#7328=CARTESIAN_POINT('Ctrl Pts',(-1.09621218093062,3.93697766708333,58.001795986152));
#7329=CARTESIAN_POINT('Ctrl Pts',(-1.21022372759133,3.90161293943607,58.0076111329144));
#7330=CARTESIAN_POINT('Ctrl Pts',(-1.32431036315668,3.86622492030001,58.0134301095784));
#7331=CARTESIAN_POINT('Ctrl Pts',(-1.43673415956687,3.82586273569657,58.0192490862424));
#7332=CARTESIAN_POINT('Ctrl Pts',(-1.54704408431669,3.78072474549269,58.0250680629064));
#7333=CARTESIAN_POINT('Ctrl Pts',(-1.65750923249171,3.73552323903257,58.0308952277864));
#7334=CARTESIAN_POINT('Ctrl Pts',(-1.76585420343812,3.68553268467108,58.0367223926664));
#7335=CARTESIAN_POINT('Ctrl Pts',(-1.87165196886338,3.63099764630189,58.0425495575463));
#7336=CARTESIAN_POINT('Ctrl Pts',(-1.89476224471286,3.6190851094434,58.0438224330863));
#7337=CARTESIAN_POINT('Ctrl Pts',(-1.91775108931573,3.60695589583663,58.0450953086263));
#7338=CARTESIAN_POINT('Ctrl Pts',(-1.9406142410025,3.59461282582955,58.0463681841663));
#7339=CARTESIAN_POINT('Ctrl Pts',(-2.04527186694745,3.53811158656426,58.0521948581947));
#7340=CARTESIAN_POINT('Ctrl Pts',(-2.14762643153128,3.47694596369644,58.0580215322231));
#7341=CARTESIAN_POINT('Ctrl Pts',(-2.24723486545104,3.41132825443423,58.0638482062514));
#7342=CARTESIAN_POINT('Ctrl Pts',(-2.34671869217198,3.34579263098163,58.0696675912833));
#7343=CARTESIAN_POINT('Ctrl Pts',(-2.44346288362712,3.27581622138491,58.0754869763151));
#7344=CARTESIAN_POINT('Ctrl Pts',(-2.53704842444072,3.20165742890192,58.081306361347));
#7345=CARTESIAN_POINT('Ctrl Pts',(-2.63054120518579,3.12757214109297,58.0871199783237));
#7346=CARTESIAN_POINT('Ctrl Pts',(-2.72088124599173,3.0493129694803,58.0929335953005));
#7347=CARTESIAN_POINT('Ctrl Pts',(-2.80767852963759,2.96718153711769,58.0987472122773));
#7348=CARTESIAN_POINT('Ctrl Pts',(-2.89718003820848,2.88249124741308,58.1047419562118));
#7349=CARTESIAN_POINT('Ctrl Pts',(-2.98291405199093,2.79368370286021,58.1107367001464));
#7350=CARTESIAN_POINT('Ctrl Pts',(-3.06448954424795,2.70113473066321,58.116731444081));
#7351=CARTESIAN_POINT('Ctrl Pts',(-3.14351277298175,2.61148135074906,58.1225386296466));
#7352=CARTESIAN_POINT('Ctrl Pts',(-3.21863352764701,2.51831749814447,58.1283458152122));
#7353=CARTESIAN_POINT('Ctrl Pts',(-3.28953431352081,2.42202167623851,58.1341530007778));
#7354=CARTESIAN_POINT('Ctrl Pts',(-3.36042495370079,2.32573963398128,58.1399593553522));
#7355=CARTESIAN_POINT('Ctrl Pts',(-3.4270965843326,2.22632684206686,58.1457657099267));
#7356=CARTESIAN_POINT('Ctrl Pts',(-3.48927326829827,2.12419327254822,58.1515720645011));
#7357=CARTESIAN_POINT('Ctrl Pts',(-3.55145568131312,2.02205029229544,58.1573789540814));
#7358=CARTESIAN_POINT('Ctrl Pts',(-3.60914211212391,1.91718638434116,58.1631858436618));
#7359=CARTESIAN_POINT('Ctrl Pts',(-3.66210140227677,1.81003820938745,58.1689927332421));
#7360=CARTESIAN_POINT('Ctrl Pts',(-3.71507803013084,1.70285495648919,58.1748015238697));
#7361=CARTESIAN_POINT('Ctrl Pts',(-3.76332425891592,1.59338631471032,58.1806103144973));
#7362=CARTESIAN_POINT('Ctrl Pts',(-3.80665636654012,1.48209051919225,58.186419105125));
#7363=CARTESIAN_POINT('Ctrl Pts',(-3.85003609117596,1.37067242237198,58.1922342789466));
#7364=CARTESIAN_POINT('Ctrl Pts',(-3.88849076799865,1.25742354435471,58.1980494527683));
#7365=CARTESIAN_POINT('Ctrl Pts',(-3.92188596860426,1.14281907984817,58.20386462659));
#7366=CARTESIAN_POINT('Ctrl Pts',(-3.95530316343759,1.02813913633134,58.209683630311));
#7367=CARTESIAN_POINT('Ctrl Pts',(-3.98365414917503,0.912102223470705,58.215502634032));
#7368=CARTESIAN_POINT('Ctrl Pts',(-4.00685556947186,0.795193967150351,58.221321637753));
#7369=CARTESIAN_POINT('Ctrl Pts',(-4.03008963684286,0.678121207430407,58.2271488294834));
#7370=CARTESIAN_POINT('Ctrl Pts',(-4.04815961548415,0.560175058809684,58.2329760212138));
#7371=CARTESIAN_POINT('Ctrl Pts',(-4.0610339287282,0.441846613338161,58.2388032129441));
#7372=CARTESIAN_POINT('Ctrl Pts',(-4.06384558870313,0.416004508386912,58.2400758308651));
#7373=CARTESIAN_POINT('Ctrl Pts',(-4.06640963620481,0.390144169142279,58.241348448786));
#7374=CARTESIAN_POINT('Ctrl Pts',(-4.06872607274419,0.364270702873046,58.242621066707));
#7375=CARTESIAN_POINT('Ctrl Pts',(-4.0795041068123,0.243885319475625,58.2485423682728));
#7376=CARTESIAN_POINT('Ctrl Pts',(-4.0849401038509,0.123014653272814,58.2544636698387));
#7377=CARTESIAN_POINT('Ctrl Pts',(-4.08499950778502,0.0020053418937903,
58.2603849714045));
#7378=CARTESIAN_POINT('Origin',(0.,0.,46.4896150285955));
#7379=CARTESIAN_POINT('',(-2.31338095599003,-3.36682247118298,55.9532017097085));
#7380=CARTESIAN_POINT('',(-2.31338095599004,-3.36682247118297,56.0572684648156));
#7381=CARTESIAN_POINT('',(-2.31338095599002,-3.36682247118298,46.4896150285955));
#7382=CARTESIAN_POINT('',(-4.08499865687907,0.00331259659223695,57.114615028566));
#7383=CARTESIAN_POINT('Ctrl Pts',(-2.31338095599003,-3.36682247118297,56.0572684648156));
#7384=CARTESIAN_POINT('Ctrl Pts',(-2.21397890120566,-3.43512272238204,56.0631597596061));
#7385=CARTESIAN_POINT('Ctrl Pts',(-2.1116806615307,-3.49892710534314,56.0690510543966));
#7386=CARTESIAN_POINT('Ctrl Pts',(-2.00693994771235,-3.55800745449983,56.0749423491871));
#7387=CARTESIAN_POINT('Ctrl Pts',(-1.90334871876782,-3.61643942190295,56.080768989518));
#7388=CARTESIAN_POINT('Ctrl Pts',(-1.79703864418861,-3.670436550343,56.0865956298489));
#7389=CARTESIAN_POINT('Ctrl Pts',(-1.68842551388699,-3.71973712566566,56.0924222701799));
#7390=CARTESIAN_POINT('Ctrl Pts',(-1.57994825985969,-3.76897602540198,56.0982416213167));
#7391=CARTESIAN_POINT('Ctrl Pts',(-1.46917404899166,-3.81352989142549,56.1040609724536));
#7392=CARTESIAN_POINT('Ctrl Pts',(-1.35654485975385,-3.85318193749989,56.1098803235905));
#7393=CARTESIAN_POINT('Ctrl Pts',(-1.24402730989515,-3.89279467999913,56.115693906518));
#7394=CARTESIAN_POINT('Ctrl Pts',(-1.12965882212408,-3.92751513407801,56.1215074894455));
#7395=CARTESIAN_POINT('Ctrl Pts',(-1.0139024859278,-3.9571740862678,56.127321072373));
#7396=CARTESIAN_POINT('Ctrl Pts',(-0.894538734921794,-3.98775732603343,
56.1333158290128));
#7397=CARTESIAN_POINT('Ctrl Pts',(-0.773699619115147,-4.01295824181281,
56.1393105856525));
#7398=CARTESIAN_POINT('Ctrl Pts',(-0.651911561980285,-4.03264631667053,
56.1453053422923));
#7399=CARTESIAN_POINT('Ctrl Pts',(-0.533934849427476,-4.05171825527315,
56.1511124936465));
#7400=CARTESIAN_POINT('Ctrl Pts',(-0.415068135911994,-4.06561718497902,
56.1569196450007));
#7401=CARTESIAN_POINT('Ctrl Pts',(-0.29580090182949,-4.07427623345262,56.1627267963549));
#7402=CARTESIAN_POINT('Ctrl Pts',(-0.176550734628493,-4.08293404283524,
56.1685331167184));
#7403=CARTESIAN_POINT('Ctrl Pts',(-0.0569005674815752,-4.08635343270106,
56.1743394370819));
#7404=CARTESIAN_POINT('Ctrl Pts',(0.0626556456337905,-4.08451946623715,
56.1801457574454));
#7405=CARTESIAN_POINT('Ctrl Pts',(0.182222875687124,-4.08268533077579,56.1859526128532));
#7406=CARTESIAN_POINT('Ctrl Pts',(0.301695726716485,-4.07559688275356,56.191759468261));
#7407=CARTESIAN_POINT('Ctrl Pts',(0.420581532512456,-4.06329129825927,56.1975663236687));
#7408=CARTESIAN_POINT('Ctrl Pts',(0.539506260688669,-4.05098168500279,56.2033750802003));
#7409=CARTESIAN_POINT('Ctrl Pts',(0.657843155966779,-4.03345158023778,56.2091838367319));
#7410=CARTESIAN_POINT('Ctrl Pts',(0.775106583720403,-4.01078979552323,56.2149925932635));
#7411=CARTESIAN_POINT('Ctrl Pts',(0.892498877004137,-3.98810310685562,56.2208077332729));
#7412=CARTESIAN_POINT('Ctrl Pts',(1.00881494749444,-3.96027355928179,56.2266228732823));
#7413=CARTESIAN_POINT('Ctrl Pts',(1.12358108680821,-3.92744071137514,56.2324380132917));
#7414=CARTESIAN_POINT('Ctrl Pts',(1.23842281457585,-3.89458623876086,56.2382569833284));
#7415=CARTESIAN_POINT('Ctrl Pts',(1.35171219223955,-3.85672203189154,56.244075953365));
#7416=CARTESIAN_POINT('Ctrl Pts',(1.46299390931844,-3.81403642107638,56.2498949234017));
#7417=CARTESIAN_POINT('Ctrl Pts',(1.57443222187445,-3.7712907431292,56.2557220818849));
#7418=CARTESIAN_POINT('Ctrl Pts',(1.68385686272124,-3.72371028227369,56.2615492403681));
#7419=CARTESIAN_POINT('Ctrl Pts',(1.79083549731539,-3.67153009269366,56.2673763988513));
#7420=CARTESIAN_POINT('Ctrl Pts',(1.81420500797559,-3.66013131665518,56.2686493431434));
#7421=CARTESIAN_POINT('Ctrl Pts',(1.83745789961868,-3.64851320605675,56.2699222874356));
#7422=CARTESIAN_POINT('Ctrl Pts',(1.86058984850693,-3.63667848670087,56.2711952317278));
#7423=CARTESIAN_POINT('Ctrl Pts',(1.9664715829446,-3.58250749496832,56.2770218721959));
#7424=CARTESIAN_POINT('Ctrl Pts',(2.07015408541998,-3.52362234382874,56.282848512664));
#7425=CARTESIAN_POINT('Ctrl Pts',(2.17118969993181,-3.4602254676408,56.2886751531321));
#7426=CARTESIAN_POINT('Ctrl Pts',(2.27209891769834,-3.39690790169264,56.2944945044042));
#7427=CARTESIAN_POINT('Ctrl Pts',(2.37036749133301,-3.32909005218638,56.3003138556764));
#7428=CARTESIAN_POINT('Ctrl Pts',(2.46557079210723,-3.25702098075952,56.3061332069485));
#7429=CARTESIAN_POINT('Ctrl Pts',(2.56067972621684,-3.185023345069,56.3119467900092));
#7430=CARTESIAN_POINT('Ctrl Pts',(2.65272910873421,-3.10878311546493,56.3177603730699));
#7431=CARTESIAN_POINT('Ctrl Pts',(2.74132234518034,-3.02859320474292,56.3235739561306));
#7432=CARTESIAN_POINT('Ctrl Pts',(2.83267648640232,-2.94590426907986,56.3295687127197));
#7433=CARTESIAN_POINT('Ctrl Pts',(2.92035516540868,-2.85901568002512,56.3355634693088));
#7434=CARTESIAN_POINT('Ctrl Pts',(3.00395912684207,-2.76829452267316,56.3415582258978));
#7435=CARTESIAN_POINT('Ctrl Pts',(3.08494671345783,-2.68041247183545,56.3473653773794));
#7436=CARTESIAN_POINT('Ctrl Pts',(3.16211051804336,-2.58893447666136,56.3531725288609));
#7437=CARTESIAN_POINT('Ctrl Pts',(3.23512474935081,-2.49423191707144,56.3589796803424));
#7438=CARTESIAN_POINT('Ctrl Pts',(3.3081285324509,-2.39954290925029,56.3647860008308));
#7439=CARTESIAN_POINT('Ctrl Pts',(3.37698367428118,-2.30163057759057,56.3705923213192));
#7440=CARTESIAN_POINT('Ctrl Pts',(3.44140523452848,-2.20089868275665,56.3763986418076));
#7441=CARTESIAN_POINT('Ctrl Pts',(3.50583273110447,-2.10015750566328,56.3822054973378));
#7442=CARTESIAN_POINT('Ctrl Pts',(3.56582561408171,-1.99659659238912,56.388012352868));
#7443=CARTESIAN_POINT('Ctrl Pts',(3.62114312018653,-1.89064737672729,56.3938192083982));
#7444=CARTESIAN_POINT('Ctrl Pts',(3.67647873682983,-1.7846634740833,56.3996279650495));
#7445=CARTESIAN_POINT('Ctrl Pts',(3.72713574371208,-1.67629007528272,56.4054367217009));
#7446=CARTESIAN_POINT('Ctrl Pts',(3.77292032486235,-1.56598123304226,56.4112454783522));
#7447=CARTESIAN_POINT('Ctrl Pts',(3.81875522050688,-1.4555511680349,56.4170606184769));
#7448=CARTESIAN_POINT('Ctrl Pts',(3.85970684631127,-1.34318179103272,56.4228757586015));
#7449=CARTESIAN_POINT('Ctrl Pts',(3.89563029261868,-1.22934520100404,56.4286908987262));
#7450=CARTESIAN_POINT('Ctrl Pts',(3.9315773991796,-1.11543363480088,56.4345098688757));
#7451=CARTESIAN_POINT('Ctrl Pts',(3.96248962543841,-1.00005332399803,56.4403288390251));
#7452=CARTESIAN_POINT('Ctrl Pts',(3.98827289048495,-0.883687926262892,56.4461478091746));
#7453=CARTESIAN_POINT('Ctrl Pts',(4.0140924376858,-0.767158779394006,56.4519749677662));
#7454=CARTESIAN_POINT('Ctrl Pts',(4.03476854853154,-0.649642179103727,56.4578021263577));
#7455=CARTESIAN_POINT('Ctrl Pts',(4.05025878816471,-0.531628393612036,56.4636292849493));
#7456=CARTESIAN_POINT('Ctrl Pts',(4.05364263184212,-0.505848275851416,56.4649022280556));
#7457=CARTESIAN_POINT('Ctrl Pts',(4.05677920100932,-0.480044436119279,56.466175171162));
#7458=CARTESIAN_POINT('Ctrl Pts',(4.05966838410138,-0.45422198441695,56.4674481142684));
#7459=CARTESIAN_POINT('Ctrl Pts',(4.0728930390211,-0.336024901690661,56.4732747554947));
#7460=CARTESIAN_POINT('Ctrl Pts',(4.08097250548031,-0.217061679068132,56.4791013967209));
#7461=CARTESIAN_POINT('Ctrl Pts',(4.08382868912331,-0.097817370100766,56.4849280379471));
#7462=CARTESIAN_POINT('Ctrl Pts',(4.08668129964938,0.0212777629340403,56.4907473899816));
#7463=CARTESIAN_POINT('Ctrl Pts',(4.08432361485388,0.140652878697699,56.496566742016));
#7464=CARTESIAN_POINT('Ctrl Pts',(4.07672913418456,0.259816409202425,56.5023860940504));
#7465=CARTESIAN_POINT('Ctrl Pts',(4.06914218125131,0.378861823453182,56.5081996778766));
#7466=CARTESIAN_POINT('Ctrl Pts',(4.05632878498824,0.497695664977626,56.5140132617028));
#7467=CARTESIAN_POINT('Ctrl Pts',(4.03831448513832,0.615825559003558,56.5198268455289));
#7468=CARTESIAN_POINT('Ctrl Pts',(4.01973879399759,0.737636811408265,56.5258216018323));
#7469=CARTESIAN_POINT('Ctrl Pts',(3.99563272050162,0.858699081083083,56.5318163581356));
#7470=CARTESIAN_POINT('Ctrl Pts',(3.96608220262526,0.97847685819296,56.537811114439));
#7471=CARTESIAN_POINT('Ctrl Pts',(3.93745645911073,1.09450622663358,56.5436182666889));
#7472=CARTESIAN_POINT('Ctrl Pts',(3.90372205868959,1.20932987424057,56.5494254189388));
#7473=CARTESIAN_POINT('Ctrl Pts',(3.86500904691189,1.3224711971492,56.5552325711887));
#7474=CARTESIAN_POINT('Ctrl Pts',(3.82630157489878,1.43559632973149,56.5610388924452));
#7475=CARTESIAN_POINT('Ctrl Pts',(3.78261704040561,1.54703923064694,56.5668452137017));
#7476=CARTESIAN_POINT('Ctrl Pts',(3.73413503207612,1.65633950693145,56.5726515349582));
#7477=CARTESIAN_POINT('Ctrl Pts',(3.68564855622843,1.76564985501351,56.5784583912554));
#7478=CARTESIAN_POINT('Ctrl Pts',(3.63236389294896,1.87281681311143,56.5842652475526));
#7479=CARTESIAN_POINT('Ctrl Pts',(3.57450808220949,1.97740157029851,56.5900721038498));
#7480=CARTESIAN_POINT('Ctrl Pts',(3.51663332993176,2.08202056771409,56.5958808612662));
#7481=CARTESIAN_POINT('Ctrl Pts',(3.45418465111976,2.18405532623511,56.6016896186825));
#7482=CARTESIAN_POINT('Ctrl Pts',(3.38743384960093,2.28309371568007,56.6074983760989));
#7483=CARTESIAN_POINT('Ctrl Pts',(3.32060969306293,2.3822409422145,56.6133135169818));
#7484=CARTESIAN_POINT('Ctrl Pts',(3.24947420514158,2.47838488878098,56.6191286578648));
#7485=CARTESIAN_POINT('Ctrl Pts',(3.17434122017362,2.57114426236776,56.6249437987477));
#7486=CARTESIAN_POINT('Ctrl Pts',(3.09915875042669,2.66396472998802,56.6307627696523));
#7487=CARTESIAN_POINT('Ctrl Pts',(3.01997380978192,2.75339588044843,56.636581740557));
#7488=CARTESIAN_POINT('Ctrl Pts',(2.93713791238661,2.83909244013315,56.6424007114616));
#7489=CARTESIAN_POINT('Ctrl Pts',(2.85418544865644,2.92490959166497,56.6482278707982));
#7490=CARTESIAN_POINT('Ctrl Pts',(2.76757206935306,3.00698138434765,56.6540550301348));
#7491=CARTESIAN_POINT('Ctrl Pts',(2.6776832921065,3.08500197523011,56.6598821894714));
#7492=CARTESIAN_POINT('Ctrl Pts',(2.65804719944135,3.10204547720317,56.6611551252506));
#7493=CARTESIAN_POINT('Ctrl Pts',(2.63825491743007,3.11889581892209,56.6624280610299));
#7494=CARTESIAN_POINT('Ctrl Pts',(2.61831064663882,3.13555008853276,56.6637009968091));
#7495=CARTESIAN_POINT('Ctrl Pts',(2.52701926482561,3.21178207022621,56.6695276358204));
#7496=CARTESIAN_POINT('Ctrl Pts',(2.43225059821607,3.28414515213955,56.6753542748318));
#7497=CARTESIAN_POINT('Ctrl Pts',(2.33436614355047,3.35230662497411,56.6811809138431));
#7498=CARTESIAN_POINT('Ctrl Pts',(2.23660414347771,3.42038282701228,56.6870002636612));
#7499=CARTESIAN_POINT('Ctrl Pts',(2.13573444020168,3.48426764386979,56.6928196134793));
#7500=CARTESIAN_POINT('Ctrl Pts',(2.03215242496763,3.54366780634108,56.6986389632974));
#7501=CARTESIAN_POINT('Ctrl Pts',(1.92867308142941,3.60300909068183,56.7044525449084));
#7502=CARTESIAN_POINT('Ctrl Pts',(1.8224871262917,3.6578743624604,56.7102661265194));
#7503=CARTESIAN_POINT('Ctrl Pts',(1.71401933092749,3.70801331351532,56.7160797081304));
#7504=CARTESIAN_POINT('Ctrl Pts',(1.6021712253028,3.75971480403306,56.7220744652645));
#7505=CARTESIAN_POINT('Ctrl Pts',(1.4878970886374,3.8063903121024,56.7280692223986));
#7506=CARTESIAN_POINT('Ctrl Pts',(1.37169098913703,3.84781611181203,56.7340639795328));
#7507=CARTESIAN_POINT('Ctrl Pts',(1.25912158196543,3.88794548311847,56.7398711295845));
#7508=CARTESIAN_POINT('Ctrl Pts',(1.14473974319271,3.92314868019171,56.7456782796363));
#7509=CARTESIAN_POINT('Ctrl Pts',(1.02901473885685,3.95327126152701,56.751485429688));
#7510=CARTESIAN_POINT('Ctrl Pts',(0.913306294372153,3.98338953242425,56.7572917487565));
#7511=CARTESIAN_POINT('Ctrl Pts',(0.796255461136269,4.0084285307815,56.763098067825));
#7512=CARTESIAN_POINT('Ctrl Pts',(0.67834531354043,4.02828408079641,56.7689043868935));
#7513=CARTESIAN_POINT('Ctrl Pts',(0.560424300506985,4.04814146050319,56.7747112410152));
#7514=CARTESIAN_POINT('Ctrl Pts',(0.441644217837552,4.06281437445065,56.7805180951369));
#7515=CARTESIAN_POINT('Ctrl Pts',(0.322496314391145,4.07225013072676,56.7863249492585));
#7516=CARTESIAN_POINT('Ctrl Pts',(0.203309402536086,4.08168897622078,56.7921337045143));
#7517=CARTESIAN_POINT('Ctrl Pts',(0.0837548367256362,4.08588722180895,56.79794245977));
#7518=CARTESIAN_POINT('Ctrl Pts',(-0.0356736949816792,4.08484423050456,
56.8037512150258));
#7519=CARTESIAN_POINT('Ctrl Pts',(-0.155233472009372,4.08380009301067,56.8095663537808));
#7520=CARTESIAN_POINT('Ctrl Pts',(-0.274666530469003,4.07750322545559,56.8153814925358));
#7521=CARTESIAN_POINT('Ctrl Pts',(-0.393481717726974,4.06600505875419,56.8211966312908));
#7522=CARTESIAN_POINT('Ctrl Pts',(-0.512375160508561,4.05449931898846,56.8270156000842));
#7523=CARTESIAN_POINT('Ctrl Pts',(-0.630649518773443,4.03778551437724,56.8328345688775));
#7524=CARTESIAN_POINT('Ctrl Pts',(-0.747822897738731,4.0159663735666,56.8386535376709));
#7525=CARTESIAN_POINT('Ctrl Pts',(-0.865161163465148,3.99411652878983,56.8444806949362));
#7526=CARTESIAN_POINT('Ctrl Pts',(-0.981394961997653,3.96714710119714,56.8503078522015));
#7527=CARTESIAN_POINT('Ctrl Pts',(-1.09605652968294,3.93521093255995,56.8561350094667));
#7528=CARTESIAN_POINT('Ctrl Pts',(-1.12110462704494,3.92823439911861,56.8574079660944));
#7529=CARTESIAN_POINT('Ctrl Pts',(-1.14607776894025,3.9210210287919,56.8586809227221));
#7530=CARTESIAN_POINT('Ctrl Pts',(-1.17097120922268,3.91357271903456,56.8599538793497));
#7531=CARTESIAN_POINT('Ctrl Pts',(-1.28491471158784,3.87947994235032,56.8657805202186));
#7532=CARTESIAN_POINT('Ctrl Pts',(-1.3975494038024,3.84035259116033,56.8716071610874));
#7533=CARTESIAN_POINT('Ctrl Pts',(-1.50839836353142,3.79630865142651,56.8774338019562));
#7534=CARTESIAN_POINT('Ctrl Pts',(-1.61910864971283,3.75231981125689,56.8832531536185));
#7535=CARTESIAN_POINT('Ctrl Pts',(-1.72803727115572,3.70342676588168,56.8890725052809));
#7536=CARTESIAN_POINT('Ctrl Pts',(-1.83472150462477,3.6497975286949,56.8948918569432));
#7537=CARTESIAN_POINT('Ctrl Pts',(-1.94129999119695,3.59622144955436,56.9007054403831));
#7538=CARTESIAN_POINT('Ctrl Pts',(-2.04563815332672,3.53791870034244,56.9065190238231));
#7539=CARTESIAN_POINT('Ctrl Pts',(-2.1472928939353,3.47510549878057,56.9123326072631));
#7540=CARTESIAN_POINT('Ctrl Pts',(-2.25211557645087,3.41033480293611,56.9183273637059));
#7541=CARTESIAN_POINT('Ctrl Pts',(-2.3540844365402,3.34076808759735,56.9243221201487));
#7542=CARTESIAN_POINT('Ctrl Pts',(-2.45274032310717,3.26669403333158,56.9303168765915));
#7543=CARTESIAN_POINT('Ctrl Pts',(-2.54830879496111,3.19493811063354,56.9361240284231));
#7544=CARTESIAN_POINT('Ctrl Pts',(-2.64076820856344,3.11895301707606,56.9419311802547));
#7545=CARTESIAN_POINT('Ctrl Pts',(-2.72973088313847,3.03904496604444,56.9477383320863));
#7546=CARTESIAN_POINT('Ctrl Pts',(-2.81868082713901,2.95914834986908,56.9535446529134));
#7547=CARTESIAN_POINT('Ctrl Pts',(-2.90413472396558,2.87533016512985,56.9593509737406));
#7548=CARTESIAN_POINT('Ctrl Pts',(-2.98573920162111,2.78793587083759,56.9651572945677));
#7549=CARTESIAN_POINT('Ctrl Pts',(-3.0673511988152,2.70053352349744,56.970964150425));
#7550=CARTESIAN_POINT('Ctrl Pts',(-3.145112793257,2.60955470951155,56.9767710062822));
#7551=CARTESIAN_POINT('Ctrl Pts',(-3.21870904564205,2.51538010636604,56.9825778621395));
#7552=CARTESIAN_POINT('Ctrl Pts',(-3.29232939273705,2.42117467135514,56.9883866191059));
#7553=CARTESIAN_POINT('Ctrl Pts',(-3.3617814346649,2.32377168750201,56.9941953760723));
#7554=CARTESIAN_POINT('Ctrl Pts',(-3.42679230487315,2.22358258206485,57.0000041330387));
#7555=CARTESIAN_POINT('Ctrl Pts',(-3.49187461789024,2.12328337517719,57.0058192734593));
#7556=CARTESIAN_POINT('Ctrl Pts',(-3.55250579538409,2.02019227762957,57.0116344138799));
#7557=CARTESIAN_POINT('Ctrl Pts',(-3.60845779855021,1.91474732434391,57.0174495543005));
#7558=CARTESIAN_POINT('Ctrl Pts',(-3.66444665326855,1.80923292206657,57.023268524735));
#7559=CARTESIAN_POINT('Ctrl Pts',(-3.71575002121323,1.70136194389109,57.0290874951696));
#7560=CARTESIAN_POINT('Ctrl Pts',(-3.76218775725437,1.59159300047635,57.0349064656041));
#7561=CARTESIAN_POINT('Ctrl Pts',(-3.80869084023158,1.48166959078613,57.040733624463));
#7562=CARTESIAN_POINT('Ctrl Pts',(-3.85031448443054,1.36984326617582,57.0465607833219));
#7563=CARTESIAN_POINT('Ctrl Pts',(-3.88692813860055,1.25658849483641,57.0523879421808));
#7564=CARTESIAN_POINT('Ctrl Pts',(-3.89492637282128,1.23184804736342,57.0536608820839));
#7565=CARTESIAN_POINT('Ctrl Pts',(-3.90268572290362,1.20703947378128,57.0549338219871));
#7566=CARTESIAN_POINT('Ctrl Pts',(-3.9102051533923,1.18216777928697,57.0562067618903));
#7567=CARTESIAN_POINT('Ctrl Pts',(-3.95200512607574,1.04390782036895,57.0632829431598));
#7568=CARTESIAN_POINT('Ctrl Pts',(-3.98649403339853,0.903343379381015,57.0703591244293));
#7569=CARTESIAN_POINT('Ctrl Pts',(-4.01345712133074,0.761174707435549,57.0774353056988));
#7570=CARTESIAN_POINT('Ctrl Pts',(-4.04010251102195,0.620681167697328,57.0844281103777));
#7571=CARTESIAN_POINT('Ctrl Pts',(-4.05939836360981,0.478620981810488,57.0914209150566));
#7572=CARTESIAN_POINT('Ctrl Pts',(-4.07118374982388,0.335690147561718,57.0984137197356));
#7573=CARTESIAN_POINT('Ctrl Pts',(-4.08028542363988,0.22530684675577,57.1038141560124));
#7574=CARTESIAN_POINT('Ctrl Pts',(-4.08490857038048,0.114404670593976,57.1092145922892));
#7575=CARTESIAN_POINT('Ctrl Pts',(-4.08499865687907,0.00331259659225328,
57.114615028566));
#7576=CARTESIAN_POINT('Ctrl Pts',(-4.08499865687956,0.00331259598633898,
57.1146150285955));
#7577=CARTESIAN_POINT('Ctrl Pts',(-4.08509496503765,-0.115451870925616,
57.1203884371961));
#7578=CARTESIAN_POINT('Ctrl Pts',(-4.08000768476869,-0.234306500596084,
57.1261618457968));
#7579=CARTESIAN_POINT('Ctrl Pts',(-4.06973999589507,-0.352762477897,57.1319352543974));
#7580=CARTESIAN_POINT('Ctrl Pts',(-4.05947579674755,-0.471178195026294,
57.1377067007634));
#7581=CARTESIAN_POINT('Ctrl Pts',(-4.04403472462242,-0.589195117883106,
57.1434781471294));
#7582=CARTESIAN_POINT('Ctrl Pts',(-4.02347200102888,-0.706327159987976,
57.1492495934954));
#7583=CARTESIAN_POINT('Ctrl Pts',(-4.00291127450329,-0.823447826136383,
57.155020479334));
#7584=CARTESIAN_POINT('Ctrl Pts',(-3.9772299570893,-0.939683375421726,57.1607913651725));
#7585=CARTESIAN_POINT('Ctrl Pts',(-3.94653469569518,-1.0545562553388,57.1665622510111));
#7586=CARTESIAN_POINT('Ctrl Pts',(-3.91583496393095,-1.16944586501366,57.172333977305));
#7587=CARTESIAN_POINT('Ctrl Pts',(-3.88011994338986,-1.28297201157841,57.1781057035989));
#7588=CARTESIAN_POINT('Ctrl Pts',(-3.83954642655221,-1.39467137288686,57.1838774298928));
#7589=CARTESIAN_POINT('Ctrl Pts',(-3.7989314253598,-1.50648494110398,57.1896550574828));
#7590=CARTESIAN_POINT('Ctrl Pts',(-3.75344814687081,-1.61646760411179,57.1954326850729));
#7591=CARTESIAN_POINT('Ctrl Pts',(-3.70330200785827,-1.72417494431188,57.201210312663));
#7592=CARTESIAN_POINT('Ctrl Pts',(-3.65313037236189,-1.83193704762064,57.2069908778509));
#7593=CARTESIAN_POINT('Ctrl Pts',(-3.59829134461344,-1.93742115709853,57.2127714430389));
#7594=CARTESIAN_POINT('Ctrl Pts',(-3.53903603327882,-2.04020806663294,57.2185520082268));
#7595=CARTESIAN_POINT('Ctrl Pts',(-3.47968342473736,-2.14316375224787,57.2243420651013));
#7596=CARTESIAN_POINT('Ctrl Pts',(-3.41590026556235,-2.24341303986314,57.2301321219759));
#7597=CARTESIAN_POINT('Ctrl Pts',(-3.34798098080885,-2.34056581880155,57.2359221788504));
#7598=CARTESIAN_POINT('Ctrl Pts',(-3.28331766470203,-2.43306121061776,57.2414346673773));
#7599=CARTESIAN_POINT('Ctrl Pts',(-3.21490579880504,-2.52274987289102,57.2469471559041));
#7600=CARTESIAN_POINT('Ctrl Pts',(-3.14303145861862,-2.60932524805431,57.252459644431));
#7601=CARTESIAN_POINT('Ctrl Pts',(-3.0670668285439,-2.70082753288646,57.2582858426353));
#7602=CARTESIAN_POINT('Ctrl Pts',(-2.98698217106811,-2.78915537539435,57.2641120408397));
#7603=CARTESIAN_POINT('Ctrl Pts',(-2.9030726580768,-2.87391616821488,57.269938239044));
#7604=CARTESIAN_POINT('Ctrl Pts',(-2.81925555558232,-2.95858361301446,57.2757580207903));
#7605=CARTESIAN_POINT('Ctrl Pts',(-2.73162225463703,-3.03969152919456,57.2815778025366));
#7606=CARTESIAN_POINT('Ctrl Pts',(-2.6405085480883,-3.11687978713851,57.2873975842829));
#7607=CARTESIAN_POINT('Ctrl Pts',(-2.54949195014274,-3.19398577816353,57.2932111633304));
#7608=CARTESIAN_POINT('Ctrl Pts',(-2.45500263837319,-3.26718016273486,57.299024742378));
#7609=CARTESIAN_POINT('Ctrl Pts',(-2.35741300912399,-3.33613982087277,57.3048383214255));
#7610=CARTESIAN_POINT('Ctrl Pts',(-2.342804626218,-3.34646252728015,57.3057085674694));
#7611=CARTESIAN_POINT('Ctrl Pts',(-2.32812683662819,-3.35669041351151,57.3065788135133));
#7612=CARTESIAN_POINT('Ctrl Pts',(-2.31338095599002,-3.36682247118298,57.3074490595572));
#7613=CARTESIAN_POINT('',(-4.0849985609995,-0.00342879453927592,57.0103849714486));
#7614=CARTESIAN_POINT('Ctrl Pts',(-4.0849985609995,-0.00342879453927238,
57.0103849714486));
#7615=CARTESIAN_POINT('Ctrl Pts',(-4.08487555327701,-0.14997778241887,57.0175132393231));
#7616=CARTESIAN_POINT('Ctrl Pts',(-4.07686266535297,-0.296190803989647,
57.0246415071976));
#7617=CARTESIAN_POINT('Ctrl Pts',(-4.06109046469521,-0.441326678959767,
57.031769775072));
#7618=CARTESIAN_POINT('Ctrl Pts',(-4.04508411276519,-0.588617215191905,
57.0390038679375));
#7619=CARTESIAN_POINT('Ctrl Pts',(-4.02108639579918,-0.734798457853202,
57.0462379608029));
#7620=CARTESIAN_POINT('Ctrl Pts',(-3.98928273098583,-0.879117905777264,
57.0534720536683));
#7621=CARTESIAN_POINT('Ctrl Pts',(-3.9722369976399,-0.956468451394702,57.0573492929333));
#7622=CARTESIAN_POINT('Ctrl Pts',(-3.95294974235968,-1.03328454509797,57.0612265321982));
#7623=CARTESIAN_POINT('Ctrl Pts',(-3.93145514333248,-1.10945277320155,57.0651037714632));
#7624=CARTESIAN_POINT('Ctrl Pts',(-3.89916052089188,-1.22389194768726,57.0709291408043));
#7625=CARTESIAN_POINT('Ctrl Pts',(-3.86181362482941,-1.3371019646882,57.0767545101455));
#7626=CARTESIAN_POINT('Ctrl Pts',(-3.81952486936604,-1.4486044222956,57.0825798794866));
#7627=CARTESIAN_POINT('Ctrl Pts',(-3.77728515920383,-1.55997756250988,57.0883984927294));
#7628=CARTESIAN_POINT('Ctrl Pts',(-3.73011512835958,-1.66964670315502,57.0942171059721));
#7629=CARTESIAN_POINT('Ctrl Pts',(-3.67817543772244,-1.77714671575965,57.1000357192149));
#7630=CARTESIAN_POINT('Ctrl Pts',(-3.62628376199816,-1.88454735149711,57.1058489535228));
#7631=CARTESIAN_POINT('Ctrl Pts',(-3.56963137148317,-1.98978248202845,57.1116621878308));
#7632=CARTESIAN_POINT('Ctrl Pts',(-3.50842745286672,-2.09240574649639,57.1174754221388));
#7633=CARTESIAN_POINT('Ctrl Pts',(-3.44726571223187,-2.19495828931354,57.1232846503227));
#7634=CARTESIAN_POINT('Ctrl Pts',(-3.38155889132315,-2.29490219765928,57.1290938785066));
#7635=CARTESIAN_POINT('Ctrl Pts',(-3.31156236831528,-2.39181514351718,57.1349031066906));
#7636=CARTESIAN_POINT('Ctrl Pts',(-3.24158781145911,-2.48869767637199,57.1407105118355));
#7637=CARTESIAN_POINT('Ctrl Pts',(-3.16732646374444,-2.58255080514865,57.1465179169805));
#7638=CARTESIAN_POINT('Ctrl Pts',(-3.08907710604279,-2.67298103863875,57.1523253221255));
#7639=CARTESIAN_POINT('Ctrl Pts',(-3.01084488953364,-2.76339146261111,57.1581314551086));
#7640=CARTESIAN_POINT('Ctrl Pts',(-2.92862667062261,-2.85038017715329,57.1639375880917));
#7641=CARTESIAN_POINT('Ctrl Pts',(-2.84276106384955,-2.93358731485207,57.1697437210748));
#7642=CARTESIAN_POINT('Ctrl Pts',(-2.75686116856737,-3.01682767945981,57.1755521726073));
#7643=CARTESIAN_POINT('Ctrl Pts',(-2.66731126677953,-3.09628316419446,57.1813606241397));
#7644=CARTESIAN_POINT('Ctrl Pts',(-2.57448627963979,-3.17163134616028,57.1871690756721));
#7645=CARTESIAN_POINT('Ctrl Pts',(-2.49005837374548,-3.24016342370037,57.1924520863623));
#7646=CARTESIAN_POINT('Ctrl Pts',(-2.40292172968864,-3.30529801528073,57.1977350970524));
#7647=CARTESIAN_POINT('Ctrl Pts',(-2.31338095599003,-3.36682247118298,57.2030181077425));
#7648=CARTESIAN_POINT('Ctrl Pts',(-2.31338095599003,-3.36682247118298,55.9532017097085));
#7649=CARTESIAN_POINT('Ctrl Pts',(-2.21490120219679,-3.43448899917066,55.9590093245328));
#7650=CARTESIAN_POINT('Ctrl Pts',(-2.1133988742849,-3.49786634484393,55.9648169393572));
#7651=CARTESIAN_POINT('Ctrl Pts',(-2.00928649021487,-3.55668283661054,55.9706245541816));
#7652=CARTESIAN_POINT('Ctrl Pts',(-1.90519567776754,-3.61548714186179,55.976430965694));
#7653=CARTESIAN_POINT('Ctrl Pts',(-1.79849623950041,-3.66973227196316,55.9822373772064));
#7654=CARTESIAN_POINT('Ctrl Pts',(-1.68962721947816,-3.71919142545776,55.9880437887188));
#7655=CARTESIAN_POINT('Ctrl Pts',(-1.58075514551467,-3.76865196635667,55.9938503631099));
#7656=CARTESIAN_POINT('Ctrl Pts',(-1.46971374017094,-3.8133260951914,55.999656937501));
#7657=CARTESIAN_POINT('Ctrl Pts',(-1.35696345988667,-3.85303454027243,56.0054635118921));
#7658=CARTESIAN_POINT('Ctrl Pts',(-1.24418349287064,-3.89275344044018,56.0112716151327));
#7659=CARTESIAN_POINT('Ctrl Pts',(-1.12969414064907,-3.92750392128263,56.0170797183733));
#7660=CARTESIAN_POINT('Ctrl Pts',(-1.01397188971186,-3.95715630306337,56.0228878216139));
#7661=CARTESIAN_POINT('Ctrl Pts',(-0.898125969859754,-3.9868403734593,56.0287021318011));
#7662=CARTESIAN_POINT('Ctrl Pts',(-0.781044916144667,-4.01141536569325,
56.0345164419883));
#7663=CARTESIAN_POINT('Ctrl Pts',(-0.663216499412574,-4.03080251003531,
56.0403307521755));
#7664=CARTESIAN_POINT('Ctrl Pts',(-0.545317251504739,-4.05020130873262,
56.0461485575673));
#7665=CARTESIAN_POINT('Ctrl Pts',(-0.42667015005983,-4.06440599917684,56.0519663629591));
#7666=CARTESIAN_POINT('Ctrl Pts',(-0.307767521396112,-4.07338976195179,
56.0577841683509));
#7667=CARTESIAN_POINT('Ctrl Pts',(-0.18868894942546,-4.08238681823379,56.0636105825004));
#7668=CARTESIAN_POINT('Ctrl Pts',(-0.0693545020969998,-4.08614750752744,
56.0694369966499));
#7669=CARTESIAN_POINT('Ctrl Pts',(0.0497437624093115,-4.08469711950609,
56.0752634107994));
#7670=CARTESIAN_POINT('Ctrl Pts',(0.108177674612077,-4.0839855067328,56.0781220601196));
#7671=CARTESIAN_POINT('Ctrl Pts',(0.166554807916021,-4.08202025660109,56.0809807094398));
#7672=CARTESIAN_POINT('Ctrl Pts',(0.224817716291339,-4.07880889408189,56.08383935876));
#7673=CARTESIAN_POINT('Ctrl Pts',(0.343572058871225,-4.07226333610362,56.0896659992445));
#7674=CARTESIAN_POINT('Ctrl Pts',(0.462229299207039,-4.0605167693811,56.0954926397291));
#7675=CARTESIAN_POINT('Ctrl Pts',(0.580298148961136,-4.04357256127701,56.1013192802136));
#7676=CARTESIAN_POINT('Ctrl Pts',(0.698219293221433,-4.02664955057282,56.1071386315037));
#7677=CARTESIAN_POINT('Ctrl Pts',(0.815553110801814,-4.00454188929853,56.1129579827937));
#7678=CARTESIAN_POINT('Ctrl Pts',(0.931810439003805,-3.97730490480219,56.1187773340838));
#7679=CARTESIAN_POINT('Ctrl Pts',(1.04795253156214,-3.95009491792818,56.1245909171638));
#7680=CARTESIAN_POINT('Ctrl Pts',(1.16301986270179,-3.91776581515896,56.1304045002437));
#7681=CARTESIAN_POINT('Ctrl Pts',(1.27653109809025,-3.88042437828757,56.1362180833237));
#7682=CARTESIAN_POINT('Ctrl Pts',(1.39357977807922,-3.84191923930526,56.1422128399061));
#7683=CARTESIAN_POINT('Ctrl Pts',(1.50897334874723,-3.79808430442617,56.1482075964884));
#7684=CARTESIAN_POINT('Ctrl Pts',(1.62219794591353,-3.7490930668995,56.1542023530708));
#7685=CARTESIAN_POINT('Ctrl Pts',(1.73187919496825,-3.7016350033767,56.1600095045749));
#7686=CARTESIAN_POINT('Ctrl Pts',(1.83952479976645,-3.64933872967957,56.165816656079));
#7687=CARTESIAN_POINT('Ctrl Pts',(1.94468629728686,-3.59241147492109,56.1716238075831));
#7688=CARTESIAN_POINT('Ctrl Pts',(2.04983274640438,-3.53549236634049,56.1774301280952));
#7689=CARTESIAN_POINT('Ctrl Pts',(2.15249543666421,-3.47394378873973,56.1832364486074));
#7690=CARTESIAN_POINT('Ctrl Pts',(2.25225010197143,-3.40801914287019,56.1890427691195));
#7691=CARTESIAN_POINT('Ctrl Pts',(2.35201395950751,-3.34208842215263,56.1948496246746));
#7692=CARTESIAN_POINT('Ctrl Pts',(2.44886891906241,-3.27178105626694,56.2006564802296));
#7693=CARTESIAN_POINT('Ctrl Pts',(2.54241986169742,-3.19739366466603,56.2064633357847));
#7694=CARTESIAN_POINT('Ctrl Pts',(2.63600143223026,-3.12298191917445,56.212272092462));
#7695=CARTESIAN_POINT('Ctrl Pts',(2.72627651549295,-3.04448774504516,56.2180808491394));
#7696=CARTESIAN_POINT('Ctrl Pts',(2.81288372255131,-2.96224748517167,56.2238896058167));
#7697=CARTESIAN_POINT('Ctrl Pts',(2.89958610573034,-2.87991684819028,56.2297047459688));
#7698=CARTESIAN_POINT('Ctrl Pts',(2.98261227131772,-2.79383218936243,56.235519886121));
#7699=CARTESIAN_POINT('Ctrl Pts',(3.06163820637459,-2.70436619067525,56.2413350262731));
#7700=CARTESIAN_POINT('Ctrl Pts',(3.14071619028187,-2.61484126699872,56.247153996451));
#7701=CARTESIAN_POINT('Ctrl Pts',(3.21578844081482,-2.52193088457491,56.2529729666288));
#7702=CARTESIAN_POINT('Ctrl Pts',(3.2865727106159,-2.42603891515261,56.2587919368066));
#7703=CARTESIAN_POINT('Ctrl Pts',(3.35745658789958,-2.33001200674313,56.2646190954276));
#7704=CARTESIAN_POINT('Ctrl Pts',(3.42404021489688,-2.23099547466168,56.2704462540486));
#7705=CARTESIAN_POINT('Ctrl Pts',(3.48608586470021,-2.12942018961438,56.2762734126696));
#7706=CARTESIAN_POINT('Ctrl Pts',(3.49963973771141,-2.10723106726703,56.2775463555466));
#7707=CARTESIAN_POINT('Ctrl Pts',(3.51297723549247,-2.08491992389572,56.2788192984236));
#7708=CARTESIAN_POINT('Ctrl Pts',(3.52609618252348,-2.0624913846107,56.2800922413006));
#7709=CARTESIAN_POINT('Ctrl Pts',(3.58614553017031,-1.9598292464411,56.2859188818971));
#7710=CARTESIAN_POINT('Ctrl Pts',(3.64180322194183,-1.85437904773052,56.2917455224936));
#7711=CARTESIAN_POINT('Ctrl Pts',(3.69280105526522,-1.74655242298422,56.2975721630902));
#7712=CARTESIAN_POINT('Ctrl Pts',(3.74373508971591,-1.6388606905786,56.3033915144927));
#7713=CARTESIAN_POINT('Ctrl Pts',(3.79002068806166,-1.52879881092131,56.3092108658952));
#7714=CARTESIAN_POINT('Ctrl Pts',(3.83143415942334,-1.41680530843302,56.3150302172977));
#7715=CARTESIAN_POINT('Ctrl Pts',(3.8728065812636,-1.30492281522571,56.3208438004905));
#7716=CARTESIAN_POINT('Ctrl Pts',(3.9093163431132,-1.19111288862575,56.3266573836832));
#7717=CARTESIAN_POINT('Ctrl Pts',(3.94078698993878,-1.07583590752924,56.332470966876));
#7718=CARTESIAN_POINT('Ctrl Pts',(3.97323838172722,-0.956966457578475,56.3384657234162));
#7719=CARTESIAN_POINT('Ctrl Pts',(4.00033124895871,-0.836537416436334,56.3444604799564));
#7720=CARTESIAN_POINT('Ctrl Pts',(4.02192683516748,-0.715073095955729,56.3504552364966));
#7721=CARTESIAN_POINT('Ctrl Pts',(4.04284659104576,-0.597409981474317,56.3562623881136));
#7722=CARTESIAN_POINT('Ctrl Pts',(4.05860793115304,-0.478775850041155,56.3620695397305));
#7723=CARTESIAN_POINT('Ctrl Pts',(4.06913631512704,-0.359659073171202,56.3678766913475));
#7724=CARTESIAN_POINT('Ctrl Pts',(4.07966319250976,-0.24055934168033,56.3736830119723));
#7725=CARTESIAN_POINT('Ctrl Pts',(4.08495856713286,-0.120977508233191,56.3794893325971));
#7726=CARTESIAN_POINT('Ctrl Pts',(4.08499975761303,-0.00140723185226689,
56.385295653222));
#7727=CARTESIAN_POINT('Ctrl Pts',(4.08504095188883,0.118174062727738,56.3911025088895));
#7728=CARTESIAN_POINT('Ctrl Pts',(4.07982699924621,0.237743390297444,56.396909364557));
#7729=CARTESIAN_POINT('Ctrl Pts',(4.06938734499027,0.356807562185923,56.4027162202245));
#7730=CARTESIAN_POINT('Ctrl Pts',(4.05894427286833,0.475910714808278,56.4085249770138));
#7731=CARTESIAN_POINT('Ctrl Pts',(4.04327213216008,0.594507976797068,56.4143337338031));
#7732=CARTESIAN_POINT('Ctrl Pts',(4.02245210756335,0.712112380428253,56.4201424905924));
#7733=CARTESIAN_POINT('Ctrl Pts',(4.00160920301424,0.82984602421194,56.4259576308554));
#7734=CARTESIAN_POINT('Ctrl Pts',(3.97560719379228,0.946584230022544,56.4317727711183));
#7735=CARTESIAN_POINT('Ctrl Pts',(3.94457819240187,1.06185115907436,56.4375879113813));
#7736=CARTESIAN_POINT('Ctrl Pts',(3.91352875438408,1.17719400636953,56.4434068816694));
#7737=CARTESIAN_POINT('Ctrl Pts',(3.87744585313556,1.29106325917657,56.4492258519575));
#7738=CARTESIAN_POINT('Ctrl Pts',(3.8365106554235,1.40300070948734,56.4550448222456));
#7739=CARTESIAN_POINT('Ctrl Pts',(3.79551785379579,1.51509567791955,56.4608719809752));
#7740=CARTESIAN_POINT('Ctrl Pts',(3.74965928412593,1.62525304328815,56.4666991397049));
#7741=CARTESIAN_POINT('Ctrl Pts',(3.69916319162955,1.73303683795039,56.4725262984345));
#7742=CARTESIAN_POINT('Ctrl Pts',(3.68813232908199,1.7565821889864,56.4737992402368));
#7743=CARTESIAN_POINT('Ctrl Pts',(3.67688033094081,1.78001437548934,56.475072182039));
#7744=CARTESIAN_POINT('Ctrl Pts',(3.66540985485052,1.80332903153159,56.4763451238413));
#7745=CARTESIAN_POINT('Ctrl Pts',(3.6129060102169,1.91004727660646,56.4821717641731));
#7746=CARTESIAN_POINT('Ctrl Pts',(3.55565409674372,2.01464048979338,56.487998404505));
#7747=CARTESIAN_POINT('Ctrl Pts',(3.49384950354949,2.11665789549162,56.4938250448369));
#7748=CARTESIAN_POINT('Ctrl Pts',(3.43212222861171,2.21854767624277,56.4996443959747));
#7749=CARTESIAN_POINT('Ctrl Pts',(3.36585381195152,2.31786771313676,56.5054637471126));
#7750=CARTESIAN_POINT('Ctrl Pts',(3.29528662535605,2.41418952378423,56.5112830982504));
#7751=CARTESIAN_POINT('Ctrl Pts',(3.22478938578709,2.51041585911848,56.5170966811789));
#7752=CARTESIAN_POINT('Ctrl Pts',(3.15000209294918,2.6036495534604,56.5229102641074));
#7753=CARTESIAN_POINT('Ctrl Pts',(3.07121140404016,2.69348946752974,56.5287238470358));
#7754=CARTESIAN_POINT('Ctrl Pts',(2.98996529277377,2.7861291405128,56.5347186036752));
#7755=CARTESIAN_POINT('Ctrl Pts',(2.90446240423398,2.87515966400845,56.5407133603147));
#7756=CARTESIAN_POINT('Ctrl Pts',(2.81506351709993,2.96017607494774,56.5467081169541));
#7757=CARTESIAN_POINT('Ctrl Pts',(2.72846235882188,3.0425319061668,56.5525152683092));
#7758=CARTESIAN_POINT('Ctrl Pts',(2.63820573231969,3.12112081890557,56.5583224196644));
#7759=CARTESIAN_POINT('Ctrl Pts',(2.54465986263442,3.19561123785378,56.5641295710195));
#7760=CARTESIAN_POINT('Ctrl Pts',(2.45112737915943,3.27009099738522,56.5699358913839));
#7761=CARTESIAN_POINT('Ctrl Pts',(2.35430690753955,3.34047317556109,56.5757422117484));
#7762=CARTESIAN_POINT('Ctrl Pts',(2.25459769021904,3.4064665351738,56.5815485321128));
#7763=CARTESIAN_POINT('Ctrl Pts',(2.15487928483334,3.47246597598247,56.5873553875215));
#7764=CARTESIAN_POINT('Ctrl Pts',(2.0522719445747,3.53407556904849,56.5931622429303));
#7765=CARTESIAN_POINT('Ctrl Pts',(1.9472032744155,3.59104781478966,56.598969098339));
#7766=CARTESIAN_POINT('Ctrl Pts',(1.84210020551024,3.64803871284469,56.6047778548715));
#7767=CARTESIAN_POINT('Ctrl Pts',(1.73453456238059,3.7003890498009,56.610586611404));
#7768=CARTESIAN_POINT('Ctrl Pts',(1.62495730238763,3.74789791288625,56.6163953679365));
#7769=CARTESIAN_POINT('Ctrl Pts',(1.51525962350574,3.79545898538537,56.6222105079468));
#7770=CARTESIAN_POINT('Ctrl Pts',(1.40354628961632,3.83816780190019,56.6280256479571));
#7771=CARTESIAN_POINT('Ctrl Pts',(1.29028706908165,3.87587206694967,56.6338407879674));
#7772=CARTESIAN_POINT('Ctrl Pts',(1.17695325259555,3.91360116516956,56.639659758005));
#7773=CARTESIAN_POINT('Ctrl Pts',(1.06207191299317,3.94631903595772,56.6454787280426));
#7774=CARTESIAN_POINT('Ctrl Pts',(0.946125173030944,3.97392402506102,56.6512976980801));
#7775=CARTESIAN_POINT('Ctrl Pts',(0.830015272978565,4.00156785986634,56.6571248565642));
#7776=CARTESIAN_POINT('Ctrl Pts',(0.712837379361212,4.02408437672899,56.6629520150482));
#7777=CARTESIAN_POINT('Ctrl Pts',(0.59508103460896,4.04142345742793,56.6687791735323));
#7778=CARTESIAN_POINT('Ctrl Pts',(0.569357130535747,4.04521118410674,56.6700521178155));
#7779=CARTESIAN_POINT('Ctrl Pts',(0.543605629490371,4.04875203824814,56.6713250620987));
#7780=CARTESIAN_POINT('Ctrl Pts',(0.5178316391104,4.05204582816338,56.6725980063819));
#7781=CARTESIAN_POINT('Ctrl Pts',(0.399856502752466,4.06712247359762,56.6784246468506));
#7782=CARTESIAN_POINT('Ctrl Pts',(0.281034631442562,4.07706657969223,56.6842512873192));
#7783=CARTESIAN_POINT('Ctrl Pts',(0.161849794244976,4.08179245480498,56.6900779277879));
#7784=CARTESIAN_POINT('Ctrl Pts',(0.0428140586837499,4.08651241779225,56.6958972790606));
#7785=CARTESIAN_POINT('Ctrl Pts',(-0.0765833356078236,4.08602711839325,
56.7017166303334));
#7786=CARTESIAN_POINT('Ctrl Pts',(-0.195851296802997,4.08030235026041,56.7075359816061));
#7787=CARTESIAN_POINT('Ctrl Pts',(-0.315001038150048,4.0745832565871,56.7133495646674));
#7788=CARTESIAN_POINT('Ctrl Pts',(-0.434021196577892,4.06363504565181,56.7191631477287));
#7789=CARTESIAN_POINT('Ctrl Pts',(-0.552419057446783,4.04747553234971,56.7249767307899));
#7790=CARTESIAN_POINT('Ctrl Pts',(-0.674506649396676,4.030812426685,56.7309714873788));
#7791=CARTESIAN_POINT('Ctrl Pts',(-0.795932080920315,4.00860787223188,56.7369662439677));
#7792=CARTESIAN_POINT('Ctrl Pts',(-0.916158560141836,3.98093939826755,56.7429610005565));
#7793=CARTESIAN_POINT('Ctrl Pts',(-1.03262256775463,3.9541368055003,56.7487681520386));
#7794=CARTESIAN_POINT('Ctrl Pts',(-1.14796111953944,3.92220727662307,56.7545753035208));
#7795=CARTESIAN_POINT('Ctrl Pts',(-1.2616956309075,3.88527336682362,56.7603824550029));
#7796=CARTESIAN_POINT('Ctrl Pts',(-1.37541386706858,3.84834474220119,56.7661887754919));
#7797=CARTESIAN_POINT('Ctrl Pts',(-1.48752813154241,3.8064132868009,56.771995095981));
#7798=CARTESIAN_POINT('Ctrl Pts',(-1.59757527168778,3.75965134703894,56.77780141647));
#7799=CARTESIAN_POINT('Ctrl Pts',(-1.70763255247513,3.71288509825006,56.7836082720008));
#7800=CARTESIAN_POINT('Ctrl Pts',(-1.81562195486502,3.66128763958747,56.7894151275316));
#7801=CARTESIAN_POINT('Ctrl Pts',(-1.92110116144567,3.60507910141957,56.7952219830624));
#7802=CARTESIAN_POINT('Ctrl Pts',(-2.02661490113119,3.54885216099584,56.8010307397144));
#7803=CARTESIAN_POINT('Ctrl Pts',(-2.12961645085554,3.48801133037091,56.8068394963664));
#7804=CARTESIAN_POINT('Ctrl Pts',(-2.22968946866473,3.42282191668302,56.8126482530184));
#7805=CARTESIAN_POINT('Ctrl Pts',(-2.32987246068705,3.35756086375977,56.8184633931437));
#7806=CARTESIAN_POINT('Ctrl Pts',(-2.42712015516095,3.28794191184065,56.824278533269));
#7807=CARTESIAN_POINT('Ctrl Pts',(-2.52104638436984,3.2142728770059,56.8300936733943));
#7808=CARTESIAN_POINT('Ctrl Pts',(-2.6150344761951,3.14055532154725,56.8359126435444));
#7809=CARTESIAN_POINT('Ctrl Pts',(-2.70569643715789,3.0627826355294,56.8417316136945));
#7810=CARTESIAN_POINT('Ctrl Pts',(-2.79268152359938,2.98130087507897,56.8475505838445));
#7811=CARTESIAN_POINT('Ctrl Pts',(-2.87978901526491,2.89970445367284,56.8533777424367));
#7812=CARTESIAN_POINT('Ctrl Pts',(-2.96320902182736,2.81438883135466,56.8592049010289));
#7813=CARTESIAN_POINT('Ctrl Pts',(-3.04262969218861,2.7257346819183,56.8650320596211));
#7814=CARTESIAN_POINT('Ctrl Pts',(-3.05997914179986,2.70636817831818,56.8663050027216));
#7815=CARTESIAN_POINT('Ctrl Pts',(-3.0771379021545,2.68684247351958,56.867577945822));
#7816=CARTESIAN_POINT('Ctrl Pts',(-3.09410299583021,2.66716172197985,56.8688508889225));
#7817=CARTESIAN_POINT('Ctrl Pts',(-3.17269838390856,2.57598531384996,56.8747481423593));
#7818=CARTESIAN_POINT('Ctrl Pts',(-3.24739993934555,2.48116956296244,56.880645395796));
#7819=CARTESIAN_POINT('Ctrl Pts',(-3.31785016116441,2.38308524985181,56.8865426492328));
#7820=CARTESIAN_POINT('Ctrl Pts',(-3.38677126205226,2.28712985517905,56.8923119028786));
#7821=CARTESIAN_POINT('Ctrl Pts',(-3.45162340496512,2.18804667540133,56.8980811565243));
#7822=CARTESIAN_POINT('Ctrl Pts',(-3.51210959684272,2.08621935082706,56.9038504101701));
#7823=CARTESIAN_POINT('Ctrl Pts',(-3.57254048409481,1.98448513051142,56.909614388787));
#7824=CARTESIAN_POINT('Ctrl Pts',(-3.62861314476093,1.88001210781938,56.9153783674039));
#7825=CARTESIAN_POINT('Ctrl Pts',(-3.68007284767165,1.77321426675681,56.9211423460207));
#7826=CARTESIAN_POINT('Ctrl Pts',(-3.73149813955135,1.66648784126047,56.9269024702732));
#7827=CARTESIAN_POINT('Ctrl Pts',(-3.77831642767281,1.5574400615493,56.9326625945256));
#7828=CARTESIAN_POINT('Ctrl Pts',(-3.82031842436584,1.44651033057178,56.9384227187781));
#7829=CARTESIAN_POINT('Ctrl Pts',(-3.86404662310433,1.33102159898496,56.9444195731636));
#7830=CARTESIAN_POINT('Ctrl Pts',(-3.90255395563487,1.21349332845696,56.9504164275492));
#7831=CARTESIAN_POINT('Ctrl Pts',(-3.93565938354699,1.09444516386089,56.9564132819347));
#7832=CARTESIAN_POINT('Ctrl Pts',(-3.96744507222734,0.980142823233796,56.9621710732874));
#7833=CARTESIAN_POINT('Ctrl Pts',(-3.99425118915626,0.864439880713943,56.9679288646401));
#7834=CARTESIAN_POINT('Ctrl Pts',(-4.01596853363508,0.747811297623225,56.9736866559928));
#7835=CARTESIAN_POINT('Ctrl Pts',(-4.03768679329499,0.631177799738453,56.9794446899821));
#7836=CARTESIAN_POINT('Ctrl Pts',(-4.0543157853813,0.51361899341479,56.9852027239713));
#7837=CARTESIAN_POINT('Ctrl Pts',(-4.06579771086683,0.395618470638135,56.9909607579606));
#7838=CARTESIAN_POINT('Ctrl Pts',(-4.07728567533725,0.27755588480637,56.996721820421));
#7839=CARTESIAN_POINT('Ctrl Pts',(-4.08362114071097,0.159051533025043,57.0024828828815));
#7840=CARTESIAN_POINT('Ctrl Pts',(-4.08479831537712,0.0405921506234354,
57.0082439453419));
#7841=CARTESIAN_POINT('Ctrl Pts',(-4.08494414274014,0.0259175064454967,
57.0089576206961));
#7842=CARTESIAN_POINT('Ctrl Pts',(-4.0850108764124,0.0112435507115259,57.0096712960503));
#7843=CARTESIAN_POINT('Ctrl Pts',(-4.08499856100026,-0.00342879363290059,
57.0103849714045));
#7844=CARTESIAN_POINT('Origin',(0.,0.,46.4896150285955));
#7845=CARTESIAN_POINT('',(-2.31338095599002,-3.36682247118298,54.7030792959875));
#7846=CARTESIAN_POINT('',(-2.31338095599002,-3.36682247118299,54.8073227890241));
#7847=CARTESIAN_POINT('',(-2.31338095599002,-3.36682247118298,46.4896150285955));
#7848=CARTESIAN_POINT('',(-4.08499967473006,-0.00163017032924335,55.8646150285584));
#7849=CARTESIAN_POINT('Ctrl Pts',(-2.31338095599002,-3.36682247118299,54.8073227890241));
#7850=CARTESIAN_POINT('Ctrl Pts',(-2.21482319399213,-3.43454259947083,54.8131297128475));
#7851=CARTESIAN_POINT('Ctrl Pts',(-2.11330224758641,-3.49792266475831,54.8189366366709));
#7852=CARTESIAN_POINT('Ctrl Pts',(-2.00924159562139,-3.55670819866134,54.8247435604943));
#7853=CARTESIAN_POINT('Ctrl Pts',(-1.90070329685815,-3.61802322716865,54.830800351615));
#7854=CARTESIAN_POINT('Ctrl Pts',(-1.7894022638471,-3.67433924177659,54.8368571427358));
#7855=CARTESIAN_POINT('Ctrl Pts',(-1.67584634546039,-3.7254213219993,54.8429139338566));
#7856=CARTESIAN_POINT('Ctrl Pts',(-1.56681507205789,-3.7744680324998,54.8487293916329));
#7857=CARTESIAN_POINT('Ctrl Pts',(-1.45570556469748,-3.81868979941789,54.8545448494092));
#7858=CARTESIAN_POINT('Ctrl Pts',(-1.34298565883407,-3.85792878630049,54.8603603071855));
#7859=CARTESIAN_POINT('Ctrl Pts',(-1.23018920423639,-3.89719442060405,54.8661797142725));
#7860=CARTESIAN_POINT('Ctrl Pts',(-1.11578056277697,-3.93147041932827,54.8719991213595));
#7861=CARTESIAN_POINT('Ctrl Pts',(-1.00024049472196,-3.96064943572621,54.8778185284466));
#7862=CARTESIAN_POINT('Ctrl Pts',(-0.884540722147535,-3.98986878463277,
54.8836459793718));
#7863=CARTESIAN_POINT('Ctrl Pts',(-0.767706799903252,-4.01397701072238,
54.889473430297));
#7864=CARTESIAN_POINT('Ctrl Pts',(-0.65022742237105,-4.03291821132002,54.8953008812222));
#7865=CARTESIAN_POINT('Ctrl Pts',(-0.635953228717375,-4.03521963963062,
54.8960089387959));
#7866=CARTESIAN_POINT('Ctrl Pts',(-0.621669508882911,-4.03744484934028,
54.8967169963696));
#7867=CARTESIAN_POINT('Ctrl Pts',(-0.607377140913246,-4.03959379253608,
54.8974250539433));
#7868=CARTESIAN_POINT('Ctrl Pts',(-0.489764544025958,-4.05727755147362,
54.9032516944387));
#7869=CARTESIAN_POINT('Ctrl Pts',(-0.371191835800804,-4.06984876630172,
54.9090783349341));
#7870=CARTESIAN_POINT('Ctrl Pts',(-0.252140770467798,-4.07721106050054,
54.9149049754295));
#7871=CARTESIAN_POINT('Ctrl Pts',(-0.133238639387124,-4.08456414438461,
54.9207243267306));
#7872=CARTESIAN_POINT('Ctrl Pts',(-0.0138597450321857,-4.08672124412869,
54.9265436780317));
#7873=CARTESIAN_POINT('Ctrl Pts',(0.10550569802293,-4.08363729384536,54.9323630293328));
#7874=CARTESIAN_POINT('Ctrl Pts',(0.224752824638586,-4.08055640041005,54.938176612424));
#7875=CARTESIAN_POINT('Ctrl Pts',(0.34398612108893,-4.0722448025657,54.9439901955153));
#7876=CARTESIAN_POINT('Ctrl Pts',(0.462712599148696,-4.05870940701463,54.9498037786065));
#7877=CARTESIAN_POINT('Ctrl Pts',(0.585139048412051,-4.04475219676319,54.9557985351847));
#7878=CARTESIAN_POINT('Ctrl Pts',(0.707026132368672,-4.02524024113901,54.961793291763));
#7879=CARTESIAN_POINT('Ctrl Pts',(0.827835474876989,-4.00023917116654,54.9677880483412));
#7880=CARTESIAN_POINT('Ctrl Pts',(0.944864106033258,-3.97602050615627,54.973595199857));
#7881=CARTESIAN_POINT('Ctrl Pts',(1.06088101671545,-3.94665125407904,54.9794023513727));
#7882=CARTESIAN_POINT('Ctrl Pts',(1.1754050273745,-3.91224334897802,54.9852095028885));
#7883=CARTESIAN_POINT('Ctrl Pts',(1.28991264987605,-3.87784036757959,54.9910158234124));
#7884=CARTESIAN_POINT('Ctrl Pts',(1.40292740676158,-3.83840028444088,54.9968221439364));
#7885=CARTESIAN_POINT('Ctrl Pts',(1.51398244476487,-3.79408515415031,55.0026284644603));
#7886=CARTESIAN_POINT('Ctrl Pts',(1.62504771631026,-3.74976594029218,55.0084353200273));
#7887=CARTESIAN_POINT('Ctrl Pts',(1.7341525311439,-3.70057093725805,55.0142421755943));
#7888=CARTESIAN_POINT('Ctrl Pts',(1.84084980866215,-3.64671043297223,55.0200490311613));
#7889=CARTESIAN_POINT('Ctrl Pts',(1.94758201809453,-3.59283229514829,55.0258577878507));
#7890=CARTESIAN_POINT('Ctrl Pts',(2.05190475874801,-3.53428580193233,55.0316665445401));
#7891=CARTESIAN_POINT('Ctrl Pts',(2.15339591934824,-3.47132698179447,55.0374753012294));
#7892=CARTESIAN_POINT('Ctrl Pts',(2.25499861264177,-3.40829897369252,55.0432904413937));
#7893=CARTESIAN_POINT('Ctrl Pts',(2.35376316806692,-3.34084917529051,55.049105581558));
#7894=CARTESIAN_POINT('Ctrl Pts',(2.44929670046909,-3.26927678134955,55.0549207217223));
#7895=CARTESIAN_POINT('Ctrl Pts',(2.5448931541213,-3.19765724768306,55.0607396919123));
#7896=CARTESIAN_POINT('Ctrl Pts',(2.63725403199957,-3.12190996881854,55.0665586621023));
#7897=CARTESIAN_POINT('Ctrl Pts',(2.72602101807498,-3.04237315413699,55.0723776322923));
#7898=CARTESIAN_POINT('Ctrl Pts',(2.81491291687529,-2.96272441540922,55.0782047909255));
#7899=CARTESIAN_POINT('Ctrl Pts',(2.9002005399884,-2.87927578204997,55.0840319495588));
#7900=CARTESIAN_POINT('Ctrl Pts',(2.98156368832814,-2.79240093332657,55.089859108192));
#7901=CARTESIAN_POINT('Ctrl Pts',(2.99933746753225,-2.77342312321095,55.091132050956));
#7902=CARTESIAN_POINT('Ctrl Pts',(3.01692412742201,-2.75428193099485,55.0924049937199));
#7903=CARTESIAN_POINT('Ctrl Pts',(3.03432059936808,-2.73498144422417,55.0936779364839));
#7904=CARTESIAN_POINT('Ctrl Pts',(3.11394946468215,-2.64663733248,55.0995045769786));
#7905=CARTESIAN_POINT('Ctrl Pts',(3.18984365620379,-2.55467215284154,55.1053312174733));
#7906=CARTESIAN_POINT('Ctrl Pts',(3.26165703567637,-2.45943456542816,55.111157857968));
#7907=CARTESIAN_POINT('Ctrl Pts',(3.33338057578459,-2.36431612133292,55.1169772092684));
#7908=CARTESIAN_POINT('Ctrl Pts',(3.40103321478146,-2.26593373506231,55.1227965605687));
#7909=CARTESIAN_POINT('Ctrl Pts',(3.46430694490073,-2.1646714280723,55.1286159118691));
#7910=CARTESIAN_POINT('Ctrl Pts',(3.52751795734966,-2.06350949347974,55.1344294949596));
#7911=CARTESIAN_POINT('Ctrl Pts',(3.5863584810659,-1.95947366116699,55.14024307805));
#7912=CARTESIAN_POINT('Ctrl Pts',(3.6405623278751,-1.85297893589125,55.1460566611405));
#7913=CARTESIAN_POINT('Ctrl Pts',(3.69645537389905,-1.7431654275973,55.152051417719));
#7914=CARTESIAN_POINT('Ctrl Pts',(3.74741775007967,-1.63073761136662,55.1580461742975));
#7915=CARTESIAN_POINT('Ctrl Pts',(3.79320721189438,-1.51618074372169,55.164040930876));
#7916=CARTESIAN_POINT('Ctrl Pts',(3.83756369894471,-1.40520891713023,55.1698480823909));
#7917=CARTESIAN_POINT('Ctrl Pts',(3.87706605204126,-1.29223971501255,55.1756552339059));
#7918=CARTESIAN_POINT('Ctrl Pts',(3.91154219895384,-1.17773622929898,55.1814623854208));
#7919=CARTESIAN_POINT('Ctrl Pts',(3.94601341239839,-1.06324912880639,55.1872687059438));
#7920=CARTESIAN_POINT('Ctrl Pts',(3.97545973254368,-0.94722857175979,55.1930750264669));
#7921=CARTESIAN_POINT('Ctrl Pts',(3.99975879488763,-0.830153348917576,55.19888134699));
#7922=CARTESIAN_POINT('Ctrl Pts',(4.02406009635076,-0.713067337783471,55.2046882025561));
#7923=CARTESIAN_POINT('Ctrl Pts',(4.04321311408866,-0.594926866941737,55.2104950581222));
#7924=CARTESIAN_POINT('Ctrl Pts',(4.0571466216387,-0.476220842178967,55.2163019136883));
#7925=CARTESIAN_POINT('Ctrl Pts',(4.07108469091791,-0.357475953925963,55.2221106703767));
#7926=CARTESIAN_POINT('Ctrl Pts',(4.07979980394908,-0.238165548319194,55.2279194270652));
#7927=CARTESIAN_POINT('Ctrl Pts',(4.08327265976366,-0.118782936597042,55.2337281837536));
#7928=CARTESIAN_POINT('Ctrl Pts',(4.0867493320383,0.000730869448708649,
55.2395433239169));
#7929=CARTESIAN_POINT('Ctrl Pts',(4.08497223630873,0.120316632144369,55.2453584640803));
#7930=CARTESIAN_POINT('Ctrl Pts',(4.07797419813884,0.239481605376798,55.2511736042436));
#7931=CARTESIAN_POINT('Ctrl Pts',(4.07097155085113,0.358725064234697,55.2569925744327));
#7932=CARTESIAN_POINT('Ctrl Pts',(4.05874115441113,0.477546776967526,55.2628115446217));
#7933=CARTESIAN_POINT('Ctrl Pts',(4.0413674454453,0.595461309318171,55.2686305148108));
#7934=CARTESIAN_POINT('Ctrl Pts',(4.0239692882311,0.713541770762001,55.274457673443));
#7935=CARTESIAN_POINT('Ctrl Pts',(4.00141345024314,0.830712105038716,55.2802848320752));
#7936=CARTESIAN_POINT('Ctrl Pts',(3.97383497965204,0.946499104328078,55.2861119907074));
#7937=CARTESIAN_POINT('Ctrl Pts',(3.96781046289726,0.971792773710525,55.2873849334798));
#7938=CARTESIAN_POINT('Ctrl Pts',(3.96154645001124,0.997020496498459,55.2886578762522));
#7939=CARTESIAN_POINT('Ctrl Pts',(3.95504465760098,1.02217745836129,55.2899308190246));
#7940=CARTESIAN_POINT('Ctrl Pts',(3.9252840054547,1.13732841117781,55.2957574595355));
#7941=CARTESIAN_POINT('Ctrl Pts',(3.89044289746043,1.25136182665304,55.3015841000464));
#7942=CARTESIAN_POINT('Ctrl Pts',(3.85062120473652,1.36379666286198,55.3074107405574));
#7943=CARTESIAN_POINT('Ctrl Pts',(3.81084932940806,1.47609084179809,55.313230091874));
#7944=CARTESIAN_POINT('Ctrl Pts',(3.76610939759966,1.5867900381358,55.3190494431907));
#7945=CARTESIAN_POINT('Ctrl Pts',(3.71655180890724,1.69542550756685,55.3248687945073));
#7946=CARTESIAN_POINT('Ctrl Pts',(3.66704334228296,1.80395329623552,55.3306823776141));
#7947=CARTESIAN_POINT('Ctrl Pts',(3.61272688731292,1.91042105863624,55.3364959607209));
#7948=CARTESIAN_POINT('Ctrl Pts',(3.55380175544378,2.01437784017911,55.3423095438277));
#7949=CARTESIAN_POINT('Ctrl Pts',(3.49304029128945,2.12157431229471,55.3483043004001));
#7950=CARTESIAN_POINT('Ctrl Pts',(3.42737834431585,2.22610032020434,55.3542990569725));
#7951=CARTESIAN_POINT('Ctrl Pts',(3.35708703013771,2.32748612715117,55.3602938135449));
#7952=CARTESIAN_POINT('Ctrl Pts',(3.2889954724853,2.42569907991174,55.3661009650761));
#7953=CARTESIAN_POINT('Ctrl Pts',(3.21656022671052,2.52096508523289,55.3719081166074));
#7954=CARTESIAN_POINT('Ctrl Pts',(3.14007263065266,2.61288516284702,55.3777152681386));
#7955=CARTESIAN_POINT('Ctrl Pts',(3.06359597981802,2.70479208688044,55.383521588678));
#7956=CARTESIAN_POINT('Ctrl Pts',(2.98306839275632,2.79335372204194,55.3893279092173));
#7957=CARTESIAN_POINT('Ctrl Pts',(2.89882172194849,2.87820388860129,55.3951342297567));
#7958=CARTESIAN_POINT('Ctrl Pts',(2.81456728794737,2.96306187396508,55.400941085339));
#7959=CARTESIAN_POINT('Ctrl Pts',(2.72659337616108,3.0442074213325,55.4067479409213));
#7960=CARTESIAN_POINT('Ctrl Pts',(2.63526848534855,3.1213114247266,55.4125547965037));
#7961=CARTESIAN_POINT('Ctrl Pts',(2.54391369543131,3.19844067141034,55.4183635532083));
#7962=CARTESIAN_POINT('Ctrl Pts',(2.44920605602495,3.27152547963709,55.4241723099129));
#7963=CARTESIAN_POINT('Ctrl Pts',(2.3515463842728,3.34027762358363,55.4299810666175));
#7964=CARTESIAN_POINT('Ctrl Pts',(2.25377939040739,3.40910532200673,55.4357962067968));
#7965=CARTESIAN_POINT('Ctrl Pts',(2.15305422253278,3.47359061754456,55.4416113469761));
#7966=CARTESIAN_POINT('Ctrl Pts',(2.04979998118545,3.53348907414925,55.4474264871554));
#7967=CARTESIAN_POINT('Ctrl Pts',(1.94647773349962,3.59342698167298,55.4532454573603));
#7968=CARTESIAN_POINT('Ctrl Pts',(1.84062345546751,3.64877184515063,55.4590644275653));
#7969=CARTESIAN_POINT('Ctrl Pts',(1.73268861931165,3.69932631008781,55.4648833977702));
#7970=CARTESIAN_POINT('Ctrl Pts',(1.62460189747605,3.74995191516421,55.4707105564181));
#7971=CARTESIAN_POINT('Ctrl Pts',(1.5144291493792,3.79577351179383,55.4765377150659));
#7972=CARTESIAN_POINT('Ctrl Pts',(1.40263956837634,3.83664270439991,55.4823648737138));
#7973=CARTESIAN_POINT('Ctrl Pts',(1.37821913804122,3.8455705781958,55.4836378163309));
#7974=CARTESIAN_POINT('Ctrl Pts',(1.35372159872691,3.85426231320738,55.4849107589481));
#7975=CARTESIAN_POINT('Ctrl Pts',(1.32915191293776,3.86271668548625,55.4861837015652));
#7976=CARTESIAN_POINT('Ctrl Pts',(1.21668908557449,3.9014148853014,55.4920103420451));
#7977=CARTESIAN_POINT('Ctrl Pts',(1.10235582985559,3.93525907455255,55.4978369825249));
#7978=CARTESIAN_POINT('Ctrl Pts',(0.986608468599427,3.96406719540523,55.5036636230047));
#7979=CARTESIAN_POINT('Ctrl Pts',(0.871005908623315,3.99283927696742,55.5094829742903));
#7980=CARTESIAN_POINT('Ctrl Pts',(0.753993154183893,4.01658772381757,55.5153023255759));
#7981=CARTESIAN_POINT('Ctrl Pts',(0.636044144039981,4.03517940701928,55.5211216768615));
#7982=CARTESIAN_POINT('Ctrl Pts',(0.518212046349538,4.05375266192477,55.5269352599373));
#7983=CARTESIAN_POINT('Ctrl Pts',(0.399445939794447,4.06717925897552,55.532748843013));
#7984=CARTESIAN_POINT('Ctrl Pts',(0.280231906400479,4.07537667935556,55.5385624260888));
#7985=CARTESIAN_POINT('Ctrl Pts',(0.157302707267462,4.08382956274173,55.5445571826729));
#7986=CARTESIAN_POINT('Ctrl Pts',(0.033897634179829,4.08672190161919,55.5505519392569));
#7987=CARTESIAN_POINT('Ctrl Pts',(-0.0894419552695308,4.08402070717541,
55.556546695841));
#7988=CARTESIAN_POINT('Ctrl Pts',(-0.208921649216648,4.08140404624055,55.5623538473415));
#7989=CARTESIAN_POINT('Ctrl Pts',(-0.32833945943321,4.07353873827955,55.5681609988421));
#7990=CARTESIAN_POINT('Ctrl Pts',(-0.447201890102587,4.06044769323392,55.5739681503426));
#7991=CARTESIAN_POINT('Ctrl Pts',(-0.56604731179769,4.04735852149046,55.5797744708515));
#7992=CARTESIAN_POINT('Ctrl Pts',(-0.684337106748181,4.02904514450999,55.5855807913604));
#7993=CARTESIAN_POINT('Ctrl Pts',(-0.801582788375328,4.00558235883129,55.5913871118693));
#7994=CARTESIAN_POINT('Ctrl Pts',(-0.918839274005289,3.98211741109426,55.5971939674214));
#7995=CARTESIAN_POINT('Ctrl Pts',(-1.0350510551185,3.95350219124539,55.6030008229734));
#7996=CARTESIAN_POINT('Ctrl Pts',(-1.14974035252565,3.91986251312137,55.6088076785255));
#7997=CARTESIAN_POINT('Ctrl Pts',(-1.26446719837932,3.88621182161002,55.6146164352001));
#7998=CARTESIAN_POINT('Ctrl Pts',(-1.37767017808778,3.84753351500041,55.6204251918747));
#7999=CARTESIAN_POINT('Ctrl Pts',(-1.48888778213046,3.80400291432888,55.6262339485492));
#8000=CARTESIAN_POINT('Ctrl Pts',(-1.60022760764993,3.76042447613788,55.632049088699));
#8001=CARTESIAN_POINT('Ctrl Pts',(-1.70957732261405,3.71198324906251,55.6378642288488));
#8002=CARTESIAN_POINT('Ctrl Pts',(-1.81649633988437,3.6589023008529,55.6436793689986));
#8003=CARTESIAN_POINT('Ctrl Pts',(-1.9234857772298,3.60578639193701,55.6494983391743));
#8004=CARTESIAN_POINT('Ctrl Pts',(-2.02804097239212,3.54802487264844,55.65531730935));
#8005=CARTESIAN_POINT('Ctrl Pts',(-2.12974826733999,3.48588544243243,55.6611362795257));
#8006=CARTESIAN_POINT('Ctrl Pts',(-2.23159868459564,3.42365856973098,55.666963438145));
#8007=CARTESIAN_POINT('Ctrl Pts',(-2.33059286620757,3.35704171751783,55.6727905967642));
#8008=CARTESIAN_POINT('Ctrl Pts',(-2.42634821453776,3.28634437358738,55.6786177553834));
#8009=CARTESIAN_POINT('Ctrl Pts',(-2.44726597214082,3.2709005375061,55.6798906982909));
#8010=CARTESIAN_POINT('Ctrl Pts',(-2.46802930543698,3.25526212365175,55.6811636411984));
#8011=CARTESIAN_POINT('Ctrl Pts',(-2.48863445605986,3.23943259601302,55.6824365841059));
#8012=CARTESIAN_POINT('Ctrl Pts',(-2.58202114796586,3.16768998914392,55.6882058176967));
#8013=CARTESIAN_POINT('Ctrl Pts',(-2.67246630657159,3.09178020599366,55.6939750512874));
#8014=CARTESIAN_POINT('Ctrl Pts',(-2.75957065685742,3.01197523061056,55.6997442848782));
#8015=CARTESIAN_POINT('Ctrl Pts',(-2.84656550524162,2.93227058083157,55.7055062657651));
#8016=CARTESIAN_POINT('Ctrl Pts',(-2.93022759101167,2.84868075368061,55.7112682466521));
#8017=CARTESIAN_POINT('Ctrl Pts',(-3.01018835185631,2.76151970594971,55.7170302275391));
#8018=CARTESIAN_POINT('Ctrl Pts',(-3.09007044606037,2.67444440861365,55.7227865396997));
#8019=CARTESIAN_POINT('Ctrl Pts',(-3.16625817678164,2.58380518314649,55.7285428518602));
#8020=CARTESIAN_POINT('Ctrl Pts',(-3.23841823802157,2.48995427983112,55.7342991640208));
#8021=CARTESIAN_POINT('Ctrl Pts',(-3.31052828810567,2.39616842069765,55.7400514867193));
#8022=CARTESIAN_POINT('Ctrl Pts',(-3.37861596748438,2.29917564034009,55.7458038094178));
#8023=CARTESIAN_POINT('Ctrl Pts',(-3.44238730437894,2.19936232727822,55.7515561321163));
#8024=CARTESIAN_POINT('Ctrl Pts',(-3.50613594230349,2.0995845420806,55.757306407315));
#8025=CARTESIAN_POINT('Ctrl Pts',(-3.56557106751066,1.99698857059399,55.7630566825137));
#8026=CARTESIAN_POINT('Ctrl Pts',(-3.62044158917792,1.89199040678087,55.7688069577124));
#8027=CARTESIAN_POINT('Ctrl Pts',(-3.67530614804565,1.78700365315637,55.7745566080266));
#8028=CARTESIAN_POINT('Ctrl Pts',(-3.72560689704342,1.67961559585343,55.7803062583408));
#8029=CARTESIAN_POINT('Ctrl Pts',(-3.7711387042501,1.57026681596055,55.786055908655));
#8030=CARTESIAN_POINT('Ctrl Pts',(-3.81667682252701,1.46090287945799,55.7918063559164));
#8031=CARTESIAN_POINT('Ctrl Pts',(-3.85744452577761,1.34957806530178,55.7975568031778));
#8032=CARTESIAN_POINT('Ctrl Pts',(-3.89328511616352,1.23675220002213,55.8033072504393));
#8033=CARTESIAN_POINT('Ctrl Pts',(-3.92915895699138,1.12382166264189,55.8090630325713));
#8034=CARTESIAN_POINT('Ctrl Pts',(-3.96009643240574,1.00938769160976,55.8148188147034));
#8035=CARTESIAN_POINT('Ctrl Pts',(-3.98599095802731,0.893924539614254,55.8205745968354));
#8036=CARTESIAN_POINT('Ctrl Pts',(-4.01189878447341,0.77840207951838,55.8263333354475));
#8037=CARTESIAN_POINT('Ctrl Pts',(-4.03275842980724,0.661849795739136,55.8320920740596));
#8038=CARTESIAN_POINT('Ctrl Pts',(-4.04851488777089,0.544749670488611,55.8378508126716));
#8039=CARTESIAN_POINT('Ctrl Pts',(-4.06429355947626,0.427484455346497,55.8436176700584));
#8040=CARTESIAN_POINT('Ctrl Pts',(-4.07495464172175,0.309670271146827,55.8493845274452));
#8041=CARTESIAN_POINT('Ctrl Pts',(-4.08049517445832,0.191791895611725,55.855151384832));
#8042=CARTESIAN_POINT('Ctrl Pts',(-4.08352591976477,0.127310851934067,55.8583059327408));
#8043=CARTESIAN_POINT('Ctrl Pts',(-4.08502539061802,0.0628105767807092,
55.8614604806496));
#8044=CARTESIAN_POINT('Ctrl Pts',(-4.08499967473006,-0.00163017032923469,
55.8646150285584));
#8045=CARTESIAN_POINT('Ctrl Pts',(-4.08499967472976,-0.00163017108645733,
55.8646150285955));
#8046=CARTESIAN_POINT('Ctrl Pts',(-4.0849614297524,-0.0974671794700561,
55.8693065079458));
#8047=CARTESIAN_POINT('Ctrl Pts',(-4.0815508193244,-0.193231850126992,55.8739979872961));
#8048=CARTESIAN_POINT('Ctrl Pts',(-4.07478160324302,-0.288755754699795,
55.8786894666465));
#8049=CARTESIAN_POINT('Ctrl Pts',(-4.06637398885077,-0.407399944105821,
55.884516455892));
#8050=CARTESIAN_POINT('Ctrl Pts',(-4.05276690521363,-0.525865457260426,
55.8903434451375));
#8051=CARTESIAN_POINT('Ctrl Pts',(-4.03397142744041,-0.64366103081852,55.896170434383));
#8052=CARTESIAN_POINT('Ctrl Pts',(-4.01519973360685,-0.761307544967347,
55.9019900501123));
#8053=CARTESIAN_POINT('Ctrl Pts',(-3.99125276903905,-0.878285406458357,
55.9078096658415));
#8054=CARTESIAN_POINT('Ctrl Pts',(-3.96219353843484,-0.994106314226605,
55.9136292815708));
#8055=CARTESIAN_POINT('Ctrl Pts',(-3.93230866040702,-1.11321799164401,55.9196142475393));
#8056=CARTESIAN_POINT('Ctrl Pts',(-3.89701666828244,-1.23110555139611,55.9255992135079));
#8057=CARTESIAN_POINT('Ctrl Pts',(-3.85644311636423,-1.34724589078867,55.9315841794764));
#8058=CARTESIAN_POINT('Ctrl Pts',(-3.81706128616502,-1.45997496943716,55.9373933557101));
#8059=CARTESIAN_POINT('Ctrl Pts',(-3.77270395398662,-1.57105761236674,55.9432025319438));
#8060=CARTESIAN_POINT('Ctrl Pts',(-3.7235369860474,-1.68002896211257,55.9490117081776));
#8061=CARTESIAN_POINT('Ctrl Pts',(-3.67438965859307,-1.78895678161364,55.9548185638485));
#8062=CARTESIAN_POINT('Ctrl Pts',(-3.620436684292,-1.89577461433207,55.9606254195194));
#8063=CARTESIAN_POINT('Ctrl Pts',(-3.56189215523888,-2.00003731826376,55.9664322751903));
#8064=CARTESIAN_POINT('Ctrl Pts',(-3.50335724029384,-2.10428290030686,55.9722381772667));
#8065=CARTESIAN_POINT('Ctrl Pts',(-3.44023247092876,-2.20597383334425,55.9780440793431));
#8066=CARTESIAN_POINT('Ctrl Pts',(-3.37277770636757,-2.30468990179372,55.9838499814196));
#8067=CARTESIAN_POINT('Ctrl Pts',(-3.30531815114227,-2.40341298109748,55.9896562958335));
#8068=CARTESIAN_POINT('Ctrl Pts',(-3.2335282204974,-2.4991604400003,55.9954626102474));
#8069=CARTESIAN_POINT('Ctrl Pts',(-3.15771050668699,-2.59154188774919,56.0012689246613));
#8070=CARTESIAN_POINT('Ctrl Pts',(-3.08183801886284,-2.68399007587354,56.0070794338093));
#8071=CARTESIAN_POINT('Ctrl Pts',(-3.00193219750778,-2.77306708261564,56.0128899429572));
#8072=CARTESIAN_POINT('Ctrl Pts',(-2.91833523262634,-2.85841642697697,56.0187004521052));
#8073=CARTESIAN_POINT('Ctrl Pts',(-2.83470157435502,-2.94380323390375,56.024513511672));
#8074=CARTESIAN_POINT('Ctrl Pts',(-2.74737384114757,-3.02545883912275,56.0303265712389));
#8075=CARTESIAN_POINT('Ctrl Pts',(-2.65672926697682,-3.10306535573919,56.0361396308057));
#8076=CARTESIAN_POINT('Ctrl Pts',(-2.56598553605099,-3.18075676668529,56.0419590493204));
#8077=CARTESIAN_POINT('Ctrl Pts',(-2.47191804151851,-3.25438999591718,56.0477784678351));
#8078=CARTESIAN_POINT('Ctrl Pts',(-2.37493505628005,-3.32368898642037,56.0535978863499));
#8079=CARTESIAN_POINT('Ctrl Pts',(-2.35454449341646,-3.3382590207286,56.0548214125051));
#8080=CARTESIAN_POINT('Ctrl Pts',(-2.33402514682412,-3.35263761934235,56.0560449386604));
#8081=CARTESIAN_POINT('Ctrl Pts',(-2.31338095599003,-3.36682247118297,56.0572684648156));
#8082=CARTESIAN_POINT('',(-4.08499907904467,0.00274302828863158,55.7603849713635));
#8083=CARTESIAN_POINT('Ctrl Pts',(-4.08499907904524,0.00274302744451809,
55.7603849714045));
#8084=CARTESIAN_POINT('Ctrl Pts',(-4.08507962007017,-0.117201092451769,
55.7662069774139));
#8085=CARTESIAN_POINT('Ctrl Pts',(-4.07987312568528,-0.237187977077858,
55.7720289834232));
#8086=CARTESIAN_POINT('Ctrl Pts',(-4.06939496226397,-0.356720676581326,
55.7778509894326));
#8087=CARTESIAN_POINT('Ctrl Pts',(-4.05891733800245,-0.476247225462436,
55.7836726958673));
#8088=CARTESIAN_POINT('Ctrl Pts',(-4.0431686192454,-0.595319232855506,55.7894944023021));
#8089=CARTESIAN_POINT('Ctrl Pts',(-4.02221613371006,-0.713444022837443,
55.7953161087369));
#8090=CARTESIAN_POINT('Ctrl Pts',(-4.00125990646559,-0.831589907624846,
55.8011388548159));
#8091=CARTESIAN_POINT('Ctrl Pts',(-3.97509813425175,-0.94878784029879,55.806961600895));
#8092=CARTESIAN_POINT('Ctrl Pts',(-3.94384932198535,-1.06455508334501,55.812784346974));
#8093=CARTESIAN_POINT('Ctrl Pts',(-3.9125877409405,-1.18036963079005,55.8186094723229));
#8094=CARTESIAN_POINT('Ctrl Pts',(-3.87623508960262,-1.29475193540395,55.8244345976717));
#8095=CARTESIAN_POINT('Ctrl Pts',(-3.83495963376548,-1.40723473784202,55.8302597230206));
#8096=CARTESIAN_POINT('Ctrl Pts',(-3.79363389169115,-1.51985457903035,55.8360919451689));
#8097=CARTESIAN_POINT('Ctrl Pts',(-3.74737351197248,-1.63056991855327,55.8419241673173));
#8098=CARTESIAN_POINT('Ctrl Pts',(-3.69639488000267,-1.73893354993515,55.8477563894657));
#8099=CARTESIAN_POINT('Ctrl Pts',(-3.64537959984465,-1.84737508318697,55.8535928043584));
#8100=CARTESIAN_POINT('Ctrl Pts',(-3.58963949908449,-1.9534611839262,55.8594292192512));
#8101=CARTESIAN_POINT('Ctrl Pts',(-3.52943605806971,-2.05677079714716,55.865265634144));
#8102=CARTESIAN_POINT('Ctrl Pts',(-3.46914148721096,-2.16023678995,55.8711108836079));
#8103=CARTESIAN_POINT('Ctrl Pts',(-3.40437030766645,-2.2609175670037,55.8769561330717));
#8104=CARTESIAN_POINT('Ctrl Pts',(-3.33542639573551,-2.35842230286071,55.8828013825356));
#8105=CARTESIAN_POINT('Ctrl Pts',(-3.31661322220324,-2.38502905412446,55.8843964137635));
#8106=CARTESIAN_POINT('Ctrl Pts',(-3.29748956415988,-2.41139951163461,55.8859914449914));
#8107=CARTESIAN_POINT('Ctrl Pts',(-3.27806208721923,-2.43752619521019,55.8875864762193));
#8108=CARTESIAN_POINT('Ctrl Pts',(-3.20710690365541,-2.53294896342057,55.893412025976));
#8109=CARTESIAN_POINT('Ctrl Pts',(-3.13186879950885,-2.62542279303147,55.8992375757327));
#8110=CARTESIAN_POINT('Ctrl Pts',(-3.05262143677735,-2.71453999118218,55.9050631254894));
#8111=CARTESIAN_POINT('Ctrl Pts',(-2.97346095662305,-2.80355948599514,55.9108822884244));
#8112=CARTESIAN_POINT('Ctrl Pts',(-2.89030022290519,-2.88922936187276,55.9167014513595));
#8113=CARTESIAN_POINT('Ctrl Pts',(-2.80345518295529,-2.97117216552005,55.9225206142945));
#8114=CARTESIAN_POINT('Ctrl Pts',(-2.71670129106433,-3.05302896624189,55.9283336697373));
#8115=CARTESIAN_POINT('Ctrl Pts',(-2.6262710829065,-3.13116620091211,55.9341467251801));
#8116=CARTESIAN_POINT('Ctrl Pts',(-2.53251903752131,-3.20524138320223,55.9399597806229));
#8117=CARTESIAN_POINT('Ctrl Pts',(-2.46133111986253,-3.26148824113224,55.9443737569847));
#8118=CARTESIAN_POINT('Ctrl Pts',(-2.38822877536372,-3.31539370669703,55.9487877333466));
#8119=CARTESIAN_POINT('Ctrl Pts',(-2.31338095599003,-3.36682247118298,55.9532017097085));
#8120=CARTESIAN_POINT('Ctrl Pts',(-2.31338095599002,-3.36682247118298,54.7030792959875));
#8121=CARTESIAN_POINT('Ctrl Pts',(-2.27413470222594,-3.39378900619601,54.7054092576502));
#8122=CARTESIAN_POINT('Ctrl Pts',(-2.23443999392367,-3.42005333803004,54.7077392193128));
#8123=CARTESIAN_POINT('Ctrl Pts',(-2.19432454529482,-3.44560078794928,54.7100691809754));
#8124=CARTESIAN_POINT('Ctrl Pts',(-2.09400602881825,-3.50948845126245,54.7158958214701));
#8125=CARTESIAN_POINT('Ctrl Pts',(-1.99073541405492,-3.5690930039375,54.7217224619647));
#8126=CARTESIAN_POINT('Ctrl Pts',(-1.88491390154344,-3.62413087288087,54.7275491024594));
#8127=CARTESIAN_POINT('Ctrl Pts',(-1.77922477296197,-3.67909988881679,54.7333684537597));
#8128=CARTESIAN_POINT('Ctrl Pts',(-1.67099145276118,-3.72951339782278,54.73918780506));
#8129=CARTESIAN_POINT('Ctrl Pts',(-1.56064369498213,-3.77513129007622,54.7450071563604));
#8130=CARTESIAN_POINT('Ctrl Pts',(-1.4504053152065,-3.82070396533499,54.7508207394508));
#8131=CARTESIAN_POINT('Ctrl Pts',(-1.3380570422053,-3.86149032568069,54.7566343225413));
#8132=CARTESIAN_POINT('Ctrl Pts',(-1.22405225467107,-3.8972966371364,54.7624479056317));
#8133=CARTESIAN_POINT('Ctrl Pts',(-1.10649464184963,-3.93421881022855,54.7684426622102));
#8134=CARTESIAN_POINT('Ctrl Pts',(-0.987175968270247,-3.96584525144488,
54.7744374187888));
#8135=CARTESIAN_POINT('Ctrl Pts',(-0.866614925145773,-3.99201748136385,
54.7804321753673));
#8136=CARTESIAN_POINT('Ctrl Pts',(-0.749826822901344,-4.01737065503029,
54.7862393268822));
#8137=CARTESIAN_POINT('Ctrl Pts',(-0.631873378760497,-4.03760581114111,
54.7920464783971));
#8138=CARTESIAN_POINT('Ctrl Pts',(-0.513239797011675,-4.05262999924289,
54.7978536299121));
#8139=CARTESIAN_POINT('Ctrl Pts',(-0.394623191492106,-4.06765203741327,
54.8036599504352));
#8140=CARTESIAN_POINT('Ctrl Pts',(-0.275327046402772,-4.07746453936188,
54.8094662709583));
#8141=CARTESIAN_POINT('Ctrl Pts',(-0.155843810341062,-4.08202617664051,
54.8152725914814));
#8142=CARTESIAN_POINT('Ctrl Pts',(-0.0363495640925718,-4.08658823426664,
54.8210794470476));
#8143=CARTESIAN_POINT('Ctrl Pts',(0.0833313998760015,-4.08589844963655,
54.8268863026137));
#8144=CARTESIAN_POINT('Ctrl Pts',(0.202705132280273,-4.07996760150706,54.8326931581799));
#8145=CARTESIAN_POINT('Ctrl Pts',(0.322117946777565,-4.07403481166096,54.8385019148684));
#8146=CARTESIAN_POINT('Ctrl Pts',(0.441222922575412,-4.06285756596303,54.8443106715569));
#8147=CARTESIAN_POINT('Ctrl Pts',(0.559530370828998,-4.04649858076337,54.8501194282454));
#8148=CARTESIAN_POINT('Ctrl Pts',(0.677967831866507,-4.03012161802096,54.8559345684088));
#8149=CARTESIAN_POINT('Ctrl Pts',(0.795605611801294,-4.00855160548719,54.8617497085722));
#8150=CARTESIAN_POINT('Ctrl Pts',(0.911963217393696,-3.98190257165101,54.8675648487356));
#8151=CARTESIAN_POINT('Ctrl Pts',(1.02839745959529,-3.95523598596181,54.8733838189247));
#8152=CARTESIAN_POINT('Ctrl Pts',(1.14354945602695,-3.92348382490905,54.8792027891139));
#8153=CARTESIAN_POINT('Ctrl Pts',(1.25695447707683,-3.88680980272466,54.885021759303));
#8154=CARTESIAN_POINT('Ctrl Pts',(1.37051908144492,-3.85008417292979,54.8908489179353));
#8155=CARTESIAN_POINT('Ctrl Pts',(1.48233142331655,-3.8084230007567,54.8966760765677));
#8156=CARTESIAN_POINT('Ctrl Pts',(1.59194721769772,-3.76203788604853,54.9025032352));
#8157=CARTESIAN_POINT('Ctrl Pts',(1.61589278739337,-3.75190505798889,54.903776177972));
#8158=CARTESIAN_POINT('Ctrl Pts',(1.63973363355421,-3.74154697378309,54.9050491207441));
#8159=CARTESIAN_POINT('Ctrl Pts',(1.66346529288866,-3.73096612412319,54.9063220635161));
#8160=CARTESIAN_POINT('Ctrl Pts',(1.77209220868144,-3.68253440475525,54.9121487040117));
#8161=CARTESIAN_POINT('Ctrl Pts',(1.87877511718031,-3.62927767174078,54.9179753445073));
#8162=CARTESIAN_POINT('Ctrl Pts',(1.98305617814506,-3.57137413250428,54.923801985003));
#8163=CARTESIAN_POINT('Ctrl Pts',(2.0872067823021,-3.51354303126193,54.9296213363042));
#8164=CARTESIAN_POINT('Ctrl Pts',(2.18896116201644,-3.45107688279009,54.9354406876055));
#8165=CARTESIAN_POINT('Ctrl Pts',(2.28788197809559,-3.38420168641076,54.9412600389068));
#8166=CARTESIAN_POINT('Ctrl Pts',(2.38670474269078,-3.31739277751777,54.9470736219982));
#8167=CARTESIAN_POINT('Ctrl Pts',(2.48269919537037,-3.24618374230914,54.9528872050896));
#8168=CARTESIAN_POINT('Ctrl Pts',(2.57545364624933,-3.17084586759133,54.958700788181));
#8169=CARTESIAN_POINT('Ctrl Pts',(2.67109868061442,-3.09316017652104,54.9646955447591));
#8170=CARTESIAN_POINT('Ctrl Pts',(2.7632980775166,-3.01108430395582,54.9706903013373));
#8171=CARTESIAN_POINT('Ctrl Pts',(2.85163352382441,-2.92496346059242,54.9766850579154));
#8172=CARTESIAN_POINT('Ctrl Pts',(2.93720452478794,-2.84153775688623,54.9824922094312));
#8173=CARTESIAN_POINT('Ctrl Pts',(3.01914949873876,-2.75431678592284,54.988299360947));
#8174=CARTESIAN_POINT('Ctrl Pts',(3.09712326188684,-2.66365397540285,54.9941065124628));
#8175=CARTESIAN_POINT('Ctrl Pts',(3.1750858671444,-2.57300413855084,54.9999128329868));
#8176=CARTESIAN_POINT('Ctrl Pts',(3.24907812593549,-2.47891375078002,55.0057191535108));
#8177=CARTESIAN_POINT('Ctrl Pts',(3.31879391547839,-2.38177075861294,55.0115254740347));
#8178=CARTESIAN_POINT('Ctrl Pts',(3.38851612921808,-2.28461881487686,55.0173323296017));
#8179=CARTESIAN_POINT('Ctrl Pts',(3.45396085241963,-2.1844140387996,55.0231391851687));
#8180=CARTESIAN_POINT('Ctrl Pts',(3.51486459638405,-2.0815743727011,55.0289460407357));
#8181=CARTESIAN_POINT('Ctrl Pts',(3.57578827979171,-1.97870103764317,55.034754797425));
#8182=CARTESIAN_POINT('Ctrl Pts',(3.6321678195309,-1.87319144763098,55.0405635541142));
#8183=CARTESIAN_POINT('Ctrl Pts',(3.68378539754664,-1.76548864194085,55.0463723108035));
#8184=CARTESIAN_POINT('Ctrl Pts',(3.73545970018174,-1.65766747733323,55.0521874509677));
#8185=CARTESIAN_POINT('Ctrl Pts',(3.78236141935878,-1.5476486541637,55.0580025911319));
#8186=CARTESIAN_POINT('Ctrl Pts',(3.82432060838779,-1.43589584728854,55.063817731296));
#8187=CARTESIAN_POINT('Ctrl Pts',(3.86630743299707,-1.32406943666324,55.0696367014859));
#8188=CARTESIAN_POINT('Ctrl Pts',(3.90334511813548,-1.21050715464037,55.0754556716758));
#8189=CARTESIAN_POINT('Ctrl Pts',(3.93531385506652,-1.09568693618272,55.0812746418656));
#8190=CARTESIAN_POINT('Ctrl Pts',(3.96732757833984,-0.980705142944693,55.0871018004987));
#8191=CARTESIAN_POINT('Ctrl Pts',(3.99425802551269,-0.864462276144644,55.0929289591317));
#8192=CARTESIAN_POINT('Ctrl Pts',(4.01603660652882,-0.747445633488134,55.0987561177647));
#8193=CARTESIAN_POINT('Ctrl Pts',(4.02079413740465,-0.721883348690442,55.1000290605287));
#8194=CARTESIAN_POINT('Ctrl Pts',(4.02530601614962,-0.696284153471523,55.1013020032927));
#8195=CARTESIAN_POINT('Ctrl Pts',(4.02957185811376,-0.67065314455208,55.1025749460567));
#8196=CARTESIAN_POINT('Ctrl Pts',(4.04909789515259,-0.553332335738597,55.1084015865575));
#8197=CARTESIAN_POINT('Ctrl Pts',(4.06352707368852,-0.434971356480761,55.1142282270584));
#8198=CARTESIAN_POINT('Ctrl Pts',(4.07275547397121,-0.316050390345526,55.1200548675592));
#8199=CARTESIAN_POINT('Ctrl Pts',(4.08197232941901,-0.197278195706544,55.1258742188658));
#8200=CARTESIAN_POINT('Ctrl Pts',(4.08600131651674,-0.0779478107034862,
55.1316935701723));
#8201=CARTESIAN_POINT('Ctrl Pts',(4.08478968715762,0.0414513171170837,55.1375129214789));
#8202=CARTESIAN_POINT('Ctrl Pts',(4.08357925877985,0.160732095109789,55.1433265045756));
#8203=CARTESIAN_POINT('Ctrl Pts',(4.07713855234978,0.280081074856549,55.1491400876723));
#8204=CARTESIAN_POINT('Ctrl Pts',(4.06546674246128,0.399005220443617,55.154953670769));
#8205=CARTESIAN_POINT('Ctrl Pts',(4.05343119434556,0.521635497153633,55.1609484273451));
#8206=CARTESIAN_POINT('Ctrl Pts',(4.03583312540292,0.643813586859018,55.1669431839213));
#8207=CARTESIAN_POINT('Ctrl Pts',(4.01272971553403,0.765000150372641,55.1729379404975));
#8208=CARTESIAN_POINT('Ctrl Pts',(3.99034932359311,0.882394197606358,55.1787450920187));
#8209=CARTESIAN_POINT('Ctrl Pts',(3.96280311173274,0.998857422566529,55.18455224354));
#8210=CARTESIAN_POINT('Ctrl Pts',(3.93019545416052,1.11390694947826,55.1903593950612));
#8211=CARTESIAN_POINT('Ctrl Pts',(3.89759246267913,1.22894001303194,55.1961657155906));
#8212=CARTESIAN_POINT('Ctrl Pts',(3.85992957711822,1.34255938861216,55.20197203612));
#8213=CARTESIAN_POINT('Ctrl Pts',(3.81736151073809,1.45429573895251,55.2077783566494));
#8214=CARTESIAN_POINT('Ctrl Pts',(3.77478952177962,1.56604238561646,55.2135852122218));
#8215=CARTESIAN_POINT('Ctrl Pts',(3.72731159849809,1.67590528093854,55.2193920677943));
#8216=CARTESIAN_POINT('Ctrl Pts',(3.6751309916417,1.7834341014668,55.2251989233667));
#8217=CARTESIAN_POINT('Ctrl Pts',(3.62293330123368,1.89099812614978,55.2310076800615));
#8218=CARTESIAN_POINT('Ctrl Pts',(3.56603004317143,1.99622618957287,55.2368164367562));
#8219=CARTESIAN_POINT('Ctrl Pts',(3.50467059470403,2.09869221721931,55.242625193451));
#8220=CARTESIAN_POINT('Ctrl Pts',(3.4432437158866,2.20127084887839,55.2484403336206));
#8221=CARTESIAN_POINT('Ctrl Pts',(3.37735108160713,2.30108103616106,55.2542554737903));
#8222=CARTESIAN_POINT('Ctrl Pts',(3.30728568843415,2.39772525012327,55.2600706139599));
#8223=CARTESIAN_POINT('Ctrl Pts',(3.23717414809192,2.49443311686321,55.2658895841552));
#8224=CARTESIAN_POINT('Ctrl Pts',(3.16288462843217,2.58797053885086,55.2717085543506));
#8225=CARTESIAN_POINT('Ctrl Pts',(3.08474967797375,2.67797394017209,55.2775275245459));
#8226=CARTESIAN_POINT('Ctrl Pts',(3.00650477617087,2.76810399409786,55.2833546831844));
#8227=CARTESIAN_POINT('Ctrl Pts',(2.9244039231842,2.85468980720146,55.2891818418228));
#8228=CARTESIAN_POINT('Ctrl Pts',(2.83881573082375,2.9374053595695,55.2950090004613));
#8229=CARTESIAN_POINT('Ctrl Pts',(2.82011899156167,2.95547457067085,55.2962819431733));
#8230=CARTESIAN_POINT('Ctrl Pts',(2.80125595581707,2.97335924771464,55.2975548858854));
#8231=CARTESIAN_POINT('Ctrl Pts',(2.78223066250909,2.99105625834658,55.2988278285974));
#8232=CARTESIAN_POINT('Ctrl Pts',(2.69514619014679,3.07206078260409,55.3046544690928));
#8233=CARTESIAN_POINT('Ctrl Pts',(2.6043825263909,3.14938787953511,55.3104811095882));
#8234=CARTESIAN_POINT('Ctrl Pts',(2.51028286019059,3.22268598560787,55.3163077500836));
#8235=CARTESIAN_POINT('Ctrl Pts',(2.41630091375526,3.29589239490668,55.3221271013848));
#8236=CARTESIAN_POINT('Ctrl Pts',(2.31899158486167,3.3650795903048,55.3279464526859));
#8237=CARTESIAN_POINT('Ctrl Pts',(2.21873401742616,3.42993357951958,55.333765803987));
#8238=CARTESIAN_POINT('Ctrl Pts',(2.11857582647777,3.49472328469287,55.3395793870783));
#8239=CARTESIAN_POINT('Ctrl Pts',(2.01547555129439,3.55518810833686,55.3453929701695));
#8240=CARTESIAN_POINT('Ctrl Pts',(1.90984397111666,3.61105538672413,55.3512065532608));
#8241=CARTESIAN_POINT('Ctrl Pts',(1.80092050684368,3.66866370320681,55.357201309839));
#8242=CARTESIAN_POINT('Ctrl Pts',(1.68930573118877,3.7213829549389,55.3631960664172));
#8243=CARTESIAN_POINT('Ctrl Pts',(1.57548104201319,3.76896331718114,55.3691908229954));
#8244=CARTESIAN_POINT('Ctrl Pts',(1.46521848044732,3.81505465869113,55.3749979745112));
#8245=CARTESIAN_POINT('Ctrl Pts',(1.3528826643103,3.8563237869193,55.3808051260269));
#8246=CARTESIAN_POINT('Ctrl Pts',(1.2389339300701,3.89259138838397,55.3866122775427));
#8247=CARTESIAN_POINT('Ctrl Pts',(1.12500150166655,3.92885380002719,55.3924185980667));
#8248=CARTESIAN_POINT('Ctrl Pts',(1.00945700268923,3.96011598466009,55.3982249185907));
#8249=CARTESIAN_POINT('Ctrl Pts',(0.892777246042168,3.98624808422022,55.4040312391146));
#8250=CARTESIAN_POINT('Ctrl Pts',(0.776086737544239,4.01238259181106,55.4098380946817));
#8251=CARTESIAN_POINT('Ctrl Pts',(0.658261161350215,4.03338598529941,55.4156449502487));
#8252=CARTESIAN_POINT('Ctrl Pts',(0.539788246117744,4.04917937974513,55.4214518058157));
#8253=CARTESIAN_POINT('Ctrl Pts',(0.421276543713065,4.06497794483351,55.427260562505));
#8254=CARTESIAN_POINT('Ctrl Pts',(0.302117484790072,4.07556306466938,55.4330693191944));
#8255=CARTESIAN_POINT('Ctrl Pts',(0.182804017234988,4.08090770433279,55.4388780758838));
#8256=CARTESIAN_POINT('Ctrl Pts',(0.0633594313408508,4.08625821743439,55.4446932160481));
#8257=CARTESIAN_POINT('Ctrl Pts',(-0.0562394942678495,4.08635673707916,
55.4505083562124));
#8258=CARTESIAN_POINT('Ctrl Pts',(-0.175499559289298,4.08122835733181,55.4563234963767));
#8259=CARTESIAN_POINT('Ctrl Pts',(-0.294838172566923,4.07609659987972,55.4621424665667));
#8260=CARTESIAN_POINT('Ctrl Pts',(-0.413837075458972,4.06573112215777,55.4679614367567));
#8261=CARTESIAN_POINT('Ctrl Pts',(-0.53200956923297,4.05020873761397,55.4737804069468));
#8262=CARTESIAN_POINT('Ctrl Pts',(-0.650348355103284,4.03466451000176,55.47960756558));
#8263=CARTESIAN_POINT('Ctrl Pts',(-0.767858010762216,4.01394896287395,55.4854347242132));
#8264=CARTESIAN_POINT('Ctrl Pts',(-0.884063268697977,3.98818970673902,55.4912618828465));
#8265=CARTESIAN_POINT('Ctrl Pts',(-0.909448306504777,3.9825625974113,55.4925348256103));
#8266=CARTESIAN_POINT('Ctrl Pts',(-0.934771161712084,3.97669498720446,55.4938077683742));
#8267=CARTESIAN_POINT('Ctrl Pts',(-0.96002699366087,3.97058851701388,55.495080711138));
#8268=CARTESIAN_POINT('Ctrl Pts',(-1.07563050494179,3.94263737301693,55.5009073516327));
#8269=CARTESIAN_POINT('Ctrl Pts',(-1.19019629028253,3.90958887226335,55.5067339921275));
#8270=CARTESIAN_POINT('Ctrl Pts',(-1.30324180069416,3.87153532967522,55.5125606326222));
#8271=CARTESIAN_POINT('Ctrl Pts',(-1.416145889871,3.83352939250691,55.5183799839226));
#8272=CARTESIAN_POINT('Ctrl Pts',(-1.52753310387075,3.79053099661766,55.524199335223));
#8273=CARTESIAN_POINT('Ctrl Pts',(-1.63693239739873,3.74268317205003,55.5300186865233));
#8274=CARTESIAN_POINT('Ctrl Pts',(-1.74622325305185,3.69488277481255,55.5358322696138));
#8275=CARTESIAN_POINT('Ctrl Pts',(-1.85352973679054,3.64224267428103,55.5416458527043));
#8276=CARTESIAN_POINT('Ctrl Pts',(-1.95839782379331,3.58495508531999,55.5474594357948));
#8277=CARTESIAN_POINT('Ctrl Pts',(-2.06653400154259,3.52588219594273,55.5534541923733));
#8278=CARTESIAN_POINT('Ctrl Pts',(-2.17207689503155,3.46186754697634,55.5594489489518));
#8279=CARTESIAN_POINT('Ctrl Pts',(-2.27455257351142,3.39317485407584,55.5654437055303));
#8280=CARTESIAN_POINT('Ctrl Pts',(-2.37382129005347,3.32663188933334,55.5712508570452));
#8281=CARTESIAN_POINT('Ctrl Pts',(-2.47021154122054,3.25569955532869,55.5770580085602));
#8282=CARTESIAN_POINT('Ctrl Pts',(-2.56331982692313,3.18066289708651,55.5828651600751));
#8283=CARTESIAN_POINT('Ctrl Pts',(-2.65641478901527,3.10563697644085,55.5886714805982));
#8284=CARTESIAN_POINT('Ctrl Pts',(-2.74622840222356,3.02650815545822,55.5944778011213));
#8285=CARTESIAN_POINT('Ctrl Pts',(-2.83238932759356,2.94360250321508,55.6002841216444));
#8286=CARTESIAN_POINT('Ctrl Pts',(-2.91855819255312,2.86068921135052,55.6060909772106));
#8287=CARTESIAN_POINT('Ctrl Pts',(-3.00107340657881,2.77399867903235,55.6118978327767));
#8288=CARTESIAN_POINT('Ctrl Pts',(-3.07960012520711,2.68389419851535,55.6177046883428));
#8289=CARTESIAN_POINT('Ctrl Pts',(-3.15815255291268,2.59376021844594,55.6235134450313));
#8290=CARTESIAN_POINT('Ctrl Pts',(-3.23271362042647,2.5002103745522,55.6293222017198));
#8291=CARTESIAN_POINT('Ctrl Pts',(-3.30298885158018,2.40364091459956,55.6351309584082));
#8292=CARTESIAN_POINT('Ctrl Pts',(-3.37334131099423,2.30696533060761,55.6409460985716));
#8293=CARTESIAN_POINT('Ctrl Pts',(-3.43939829295682,2.20726383692335,55.646761238735));
#8294=CARTESIAN_POINT('Ctrl Pts',(-3.50090866213717,2.10496164795773,55.6525763788983));
#8295=CARTESIAN_POINT('Ctrl Pts',(-3.56245954389156,2.00259207970209,55.6583953490874));
#8296=CARTESIAN_POINT('Ctrl Pts',(-3.61945765488474,1.89761876234378,55.6642143192765));
#8297=CARTESIAN_POINT('Ctrl Pts',(-3.67169858470686,1.79049001758224,55.6700332894656));
#8298=CARTESIAN_POINT('Ctrl Pts',(-3.72401302786043,1.68321052146639,55.6758604480978));
#8299=CARTESIAN_POINT('Ctrl Pts',(-3.77155676736374,1.57376991704553,55.68168760673));
#8300=CARTESIAN_POINT('Ctrl Pts',(-3.81417406779311,1.4626350127679,55.6875147653623));
#8301=CARTESIAN_POINT('Ctrl Pts',(-3.82348381684447,1.43835759352155,55.6887877081344));
#8302=CARTESIAN_POINT('Ctrl Pts',(-3.8325586653512,1.41399937152597,55.6900606509065));
#8303=CARTESIAN_POINT('Ctrl Pts',(-3.84139731169079,1.38956528948256,55.6913335936786));
#8304=CARTESIAN_POINT('Ctrl Pts',(-3.887911547906,1.26097855569982,55.698032578853));
#8305=CARTESIAN_POINT('Ctrl Pts',(-3.92800186419981,1.12995375257658,55.7047315640274));
#8306=CARTESIAN_POINT('Ctrl Pts',(-3.96144195472371,0.997097106281418,55.7114305492018));
#8307=CARTESIAN_POINT('Ctrl Pts',(-3.99475499066144,0.864745244690844,55.7181040817899));
#8308=CARTESIAN_POINT('Ctrl Pts',(-4.02146813859723,0.73057557588834,55.724777614378));
#8309=CARTESIAN_POINT('Ctrl Pts',(-4.04140466040663,0.595208678400749,55.7314511469661));
#8310=CARTESIAN_POINT('Ctrl Pts',(-4.06120264161761,0.460782457083427,55.7380783046044));
#8311=CARTESIAN_POINT('Ctrl Pts',(-4.07431776582529,0.325175745336553,55.7447054622427));
#8312=CARTESIAN_POINT('Ctrl Pts',(-4.0806247467514,0.189015015805715,55.751332619881));
#8313=CARTESIAN_POINT('Ctrl Pts',(-4.08349641568564,0.127018865565581,55.7543500703752));
#8314=CARTESIAN_POINT('Ctrl Pts',(-4.08495733593587,0.0649081039118598,
55.7573675208694));
#8315=CARTESIAN_POINT('Ctrl Pts',(-4.08499907904467,0.00274302828863158,
55.7603849713635));
#8316=CARTESIAN_POINT('Origin',(0.,0.,46.4896150285955));
#8317=CARTESIAN_POINT('',(-2.31338095599002,-3.36682247118299,53.4530632234442));
#8318=CARTESIAN_POINT('',(-2.31338095599001,-3.36682247118299,53.5574546183695));
#8319=CARTESIAN_POINT('',(-2.31338095599002,-3.36682247118298,46.4896150285955));
#8320=CARTESIAN_POINT('',(-4.08499981754213,-0.00122093438978996,54.6146150286217));
#8321=CARTESIAN_POINT('Ctrl Pts',(-2.31338095599001,-3.36682247118299,53.5574546183695));
#8322=CARTESIAN_POINT('Ctrl Pts',(-2.21507323877183,-3.43437079093728,53.5632685315697));
#8323=CARTESIAN_POINT('Ctrl Pts',(-2.11370279085638,-3.49767973840142,53.5690824447699));
#8324=CARTESIAN_POINT('Ctrl Pts',(-2.00967227144596,-3.55646486857121,53.5748963579702));
#8325=CARTESIAN_POINT('Ctrl Pts',(-1.90155797433677,-3.61755764273785,53.5809384996672));
#8326=CARTESIAN_POINT('Ctrl Pts',(-1.79057083243497,-3.67376387503014,53.5869806413643));
#8327=CARTESIAN_POINT('Ctrl Pts',(-1.67719615426145,-3.72481382892227,53.5930227830613));
#8328=CARTESIAN_POINT('Ctrl Pts',(-1.56822916280103,-3.7738791050442,53.5988300233844));
#8329=CARTESIAN_POINT('Ctrl Pts',(-1.45705721270963,-3.81818134763452,53.6046372637075));
#8330=CARTESIAN_POINT('Ctrl Pts',(-1.34413539373244,-3.85752835936636,53.6104445040305));
#8331=CARTESIAN_POINT('Ctrl Pts',(-1.23123125071837,-3.89686921200216,53.6162508353303));
#8332=CARTESIAN_POINT('Ctrl Pts',(-1.11657816855113,-3.93125624223149,53.6220571666301));
#8333=CARTESIAN_POINT('Ctrl Pts',(-1.00064911336343,-3.96054621888509,53.6278634979298));
#8334=CARTESIAN_POINT('Ctrl Pts',(-0.884710932964752,-3.98983850106266,
53.6336702862677));
#8335=CARTESIAN_POINT('Ctrl Pts',(-0.767496975267442,-4.0140328321037,53.6394770746056));
#8336=CARTESIAN_POINT('Ctrl Pts',(-0.649492567833327,-4.03303662323184,
53.6452838629435));
#8337=CARTESIAN_POINT('Ctrl Pts',(-0.53145111195188,-4.05204638075539,53.65109247437));
#8338=CARTESIAN_POINT('Ctrl Pts',(-0.41261911520761,-4.06586229259228,53.6569010857965));
#8339=CARTESIAN_POINT('Ctrl Pts',(-0.293488597444497,-4.07444345195391,
53.6627096972231));
#8340=CARTESIAN_POINT('Ctrl Pts',(-0.174227900411427,-4.08303398833396,
53.6685246559803));
#8341=CARTESIAN_POINT('Ctrl Pts',(-0.0546684382242412,-4.08637832452129,
53.6743396147375));
#8342=CARTESIAN_POINT('Ctrl Pts',(0.0646960231269892,-4.08448765753938,
53.6801545734947));
#8343=CARTESIAN_POINT('Ctrl Pts',(0.184137663127862,-4.08259576809039,53.6859732920868));
#8344=CARTESIAN_POINT('Ctrl Pts',(0.303383644970468,-4.0754621583867,53.6917920106789));
#8345=CARTESIAN_POINT('Ctrl Pts',(0.421945228617589,-4.06314991405029,53.697610729271));
#8346=CARTESIAN_POINT('Ctrl Pts',(0.540675418571428,-4.05082016048381,53.7034377226569));
#8347=CARTESIAN_POINT('Ctrl Pts',(0.658718865578198,-4.03329713211679,53.7092647160428));
#8348=CARTESIAN_POINT('Ctrl Pts',(0.77559677164338,-4.01069503301066,53.7150917094286));
#8349=CARTESIAN_POINT('Ctrl Pts',(0.80779689710556,-4.00446810397481,53.7166970591855));
#8350=CARTESIAN_POINT('Ctrl Pts',(0.839908645801648,-3.9978559574552,53.7183024089425));
#8351=CARTESIAN_POINT('Ctrl Pts',(0.871922226930701,-3.99086164007025,53.7199077586994));
#8352=CARTESIAN_POINT('Ctrl Pts',(0.988115989079898,-3.96547566255819,53.7257343991827));
#8353=CARTESIAN_POINT('Ctrl Pts',(1.10338508462331,-3.93497061164439,53.731561039666));
#8354=CARTESIAN_POINT('Ctrl Pts',(1.21724503980884,-3.89942810076821,53.7373876801494));
#8355=CARTESIAN_POINT('Ctrl Pts',(1.33096255487992,-3.86393005398222,53.7432070314384));
#8356=CARTESIAN_POINT('Ctrl Pts',(1.44327405004653,-3.82340720250275,53.7490263827274));
#8357=CARTESIAN_POINT('Ctrl Pts',(1.55370543010105,-3.77799211704769,53.7548457340164));
#8358=CARTESIAN_POINT('Ctrl Pts',(1.66402734926497,-3.73262204756271,53.7606593170956));
#8359=CARTESIAN_POINT('Ctrl Pts',(1.77247248578099,-3.68236954563469,53.7664729001747));
#8360=CARTESIAN_POINT('Ctrl Pts',(1.87858267227964,-3.62741673142344,53.7722864832539));
#8361=CARTESIAN_POINT('Ctrl Pts',(1.98799965838778,-3.57075137715763,53.7782812398366));
#8362=CARTESIAN_POINT('Ctrl Pts',(2.0949333571339,-3.50908808380912,53.7842759964194));
#8363=CARTESIAN_POINT('Ctrl Pts',(2.19890411777047,-3.44268001429876,53.7902707530021));
#8364=CARTESIAN_POINT('Ctrl Pts',(2.29962112781829,-3.37835017614829,53.7960779045059));
#8365=CARTESIAN_POINT('Ctrl Pts',(2.3975575147714,-3.30956834288976,53.8018850560097));
#8366=CARTESIAN_POINT('Ctrl Pts',(2.49230356927486,-3.23661056022806,53.8076922075135));
#8367=CARTESIAN_POINT('Ctrl Pts',(2.58703606580779,-3.16366321767886,53.8134985280255));
#8368=CARTESIAN_POINT('Ctrl Pts',(2.67857881480949,-3.08654136292323,53.8193048485376));
#8369=CARTESIAN_POINT('Ctrl Pts',(2.76655335231605,-3.00556276740128,53.8251111690496));
#8370=CARTESIAN_POINT('Ctrl Pts',(2.85453599653532,-2.92457670983146,53.8309180246048));
#8371=CARTESIAN_POINT('Ctrl Pts',(2.93894947545509,-2.83973348108884,53.83672488016));
#8372=CARTESIAN_POINT('Ctrl Pts',(3.01945098691094,-2.75138887430377,53.8425317357151));
#8373=CARTESIAN_POINT('Ctrl Pts',(3.09997885397798,-2.66301534413496,53.8483404923927));
#8374=CARTESIAN_POINT('Ctrl Pts',(3.17659193188125,-2.57113845736897,53.8541492490703));
#8375=CARTESIAN_POINT('Ctrl Pts',(3.24898704755551,-2.47614784793165,53.8599580057479));
#8376=CARTESIAN_POINT('Ctrl Pts',(3.32146172111921,-2.38105284951265,53.8657731459006));
#8377=CARTESIAN_POINT('Ctrl Pts',(3.38970893300221,-2.28283762297132,53.8715882860533));
#8378=CARTESIAN_POINT('Ctrl Pts',(3.45346819932686,-2.18192172092357,53.8774034262061));
#8379=CARTESIAN_POINT('Ctrl Pts',(3.51726945941804,-2.08093935263376,53.8832223963846));
#8380=CARTESIAN_POINT('Ctrl Pts',(3.57657668506128,-1.97725311948707,53.8890413665632));
#8381=CARTESIAN_POINT('Ctrl Pts',(3.63117559448954,-1.87130670975753,53.8948603367418));
#8382=CARTESIAN_POINT('Ctrl Pts',(3.68585133539594,-1.76521121244823,53.9006874953638));
#8383=CARTESIAN_POINT('Ctrl Pts',(3.73580536663856,-1.65684955979108,53.9065146539857));
#8384=CARTESIAN_POINT('Ctrl Pts',(3.78087166040175,-1.54668499946528,53.9123418126077));
#8385=CARTESIAN_POINT('Ctrl Pts',(3.79071639286584,-1.52261954981614,53.9136147554852));
#8386=CARTESIAN_POINT('Ctrl Pts',(3.80032807045,-1.49846811881181,53.9148876983626));
#8387=CARTESIAN_POINT('Ctrl Pts',(3.80970528246749,-1.47423561913939,53.9161606412401));
#8388=CARTESIAN_POINT('Ctrl Pts',(3.85262758802718,-1.3633162164988,53.9219872817217));
#8389=CARTESIAN_POINT('Ctrl Pts',(3.89077006661586,-1.25034421188072,53.9278139222034));
#8390=CARTESIAN_POINT('Ctrl Pts',(3.92393353880419,-1.13576871899502,53.9336405626851));
#8391=CARTESIAN_POINT('Ctrl Pts',(3.95705552310549,-1.02133656137529,53.9394599139721));
#8392=CARTESIAN_POINT('Ctrl Pts',(3.98521077794245,-0.905305293834171,53.9452792652592));
#8393=CARTESIAN_POINT('Ctrl Pts',(4.0082483518158,-0.788143483235101,53.9510986165463));
#8394=CARTESIAN_POINT('Ctrl Pts',(4.03126309057218,-0.671097804814871,53.9569121996232));
#8395=CARTESIAN_POINT('Ctrl Pts',(4.04917016199053,-0.552924210630184,53.9627257827001));
#8396=CARTESIAN_POINT('Ctrl Pts',(4.06186872942208,-0.434105315497335,53.968539365777));
#8397=CARTESIAN_POINT('Ctrl Pts',(4.07496303283255,-0.311583568682053,53.9745341223605));
#8398=CARTESIAN_POINT('Ctrl Pts',(4.08251875788642,-0.188376066085167,53.980528878944));
#8399=CARTESIAN_POINT('Ctrl Pts',(4.0844824727802,-0.0650225311052865,53.9865236355275));
#8400=CARTESIAN_POINT('Ctrl Pts',(4.0863847334865,0.0544706719653243,53.9923307870283));
#8401=CARTESIAN_POINT('Ctrl Pts',(4.08303975986409,0.174100465976518,53.9981379385291));
#8402=CARTESIAN_POINT('Ctrl Pts',(4.07445178836443,0.293372841779753,54.0039450900299));
#8403=CARTESIAN_POINT('Ctrl Pts',(4.06586504578666,0.412628149939694,54.0097514105388));
#8404=CARTESIAN_POINT('Ctrl Pts',(4.05203682673918,0.531525734957949,54.0155577310476));
#8405=CARTESIAN_POINT('Ctrl Pts',(4.03302340655613,0.649574631717078,54.0213640515564));
#8406=CARTESIAN_POINT('Ctrl Pts',(4.01400823431782,0.767634406487022,54.027170907108));
#8407=CARTESIAN_POINT('Ctrl Pts',(3.98980697579756,0.884844934869403,54.0329777626597));
#8408=CARTESIAN_POINT('Ctrl Pts',(3.96052729195874,1.00072402272053,54.0387846182114));
#8409=CARTESIAN_POINT('Ctrl Pts',(3.93123802216488,1.11664104854028,54.0445933748852));
#8410=CARTESIAN_POINT('Ctrl Pts',(3.89686712022224,1.231225371725,54.050402131559));
#8411=CARTESIAN_POINT('Ctrl Pts',(3.85757233399246,1.34400918449836,54.0562108882329));
#8412=CARTESIAN_POINT('Ctrl Pts',(3.81823436515222,1.45691693990942,54.0620260283815));
#8413=CARTESIAN_POINT('Ctrl Pts',(3.7739618456986,1.56801985017223,54.0678411685301));
#8414=CARTESIAN_POINT('Ctrl Pts',(3.7249610270647,1.676869209822,54.0736563086787));
#8415=CARTESIAN_POINT('Ctrl Pts',(3.67592793502284,1.78579026092283,54.0794752788529));
#8416=CARTESIAN_POINT('Ctrl Pts',(3.62216052476994,1.89245444210414,54.0852942490271));
#8417=CARTESIAN_POINT('Ctrl Pts',(3.56391066560922,1.99643827040979,54.0911132192014));
#8418=CARTESIAN_POINT('Ctrl Pts',(3.50557883736368,2.10056842454979,54.0969403778187));
#8419=CARTESIAN_POINT('Ctrl Pts',(3.44275218512514,2.20201035260932,54.1027675364361));
#8420=CARTESIAN_POINT('Ctrl Pts',(3.37572551094116,2.30037002996932,54.1085946950534));
#8421=CARTESIAN_POINT('Ctrl Pts',(3.36108353271044,2.32185670333062,54.1098676379625));
#8422=CARTESIAN_POINT('Ctrl Pts',(3.3462412776424,2.34319641899314,54.1111405808716));
#8423=CARTESIAN_POINT('Ctrl Pts',(3.33120206516043,2.36438529031773,54.1124135237807));
#8424=CARTESIAN_POINT('Ctrl Pts',(3.2623630904796,2.46137309326144,54.1182401642909));
#8425=CARTESIAN_POINT('Ctrl Pts',(3.18917535426923,2.55550639195625,54.1240668048011));
#8426=CARTESIAN_POINT('Ctrl Pts',(3.11190358208296,2.64637130724682,54.1298934453113));
#8427=CARTESIAN_POINT('Ctrl Pts',(3.0347284777701,2.73712254948601,54.1357127966274));
#8428=CARTESIAN_POINT('Ctrl Pts',(2.95347976177254,2.8246132331025,54.1415321479435));
#8429=CARTESIAN_POINT('Ctrl Pts',(2.86846498941049,2.90845897418655,54.1473514992596));
#8430=CARTESIAN_POINT('Ctrl Pts',(2.78353448469444,2.99222160638221,54.153165082366));
#8431=CARTESIAN_POINT('Ctrl Pts',(2.69484563885741,3.0723461989703,54.1589786654723));
#8432=CARTESIAN_POINT('Ctrl Pts',(2.60274536947073,3.14848241883271,54.1647922485787));
#8433=CARTESIAN_POINT('Ctrl Pts',(2.50777490372805,3.22699133426121,54.1707870051513));
#8434=CARTESIAN_POINT('Ctrl Pts',(2.40917719148304,3.30125888272042,54.1767817617239));
#8435=CARTESIAN_POINT('Ctrl Pts',(2.30737293390592,3.37094276781413,54.1827765182965));
#8436=CARTESIAN_POINT('Ctrl Pts',(2.20875462587246,3.43844590578392,54.1885836698277));
#8437=CARTESIAN_POINT('Ctrl Pts',(2.10712783743867,3.5016477449496,54.1943908213588));
#8438=CARTESIAN_POINT('Ctrl Pts',(2.00290695190488,3.56027930674141,54.2001979728899));
#8439=CARTESIAN_POINT('Ctrl Pts',(1.89870098017042,3.61890247847453,54.2060042934293));
#8440=CARTESIAN_POINT('Ctrl Pts',(1.79190200493657,3.67295647360696,54.2118106139687));
#8441=CARTESIAN_POINT('Ctrl Pts',(1.68295057692418,3.72221739768523,54.2176169345081));
#8442=CARTESIAN_POINT('Ctrl Pts',(1.57398910921333,3.77148286107823,54.2234237900906));
#8443=CARTESIAN_POINT('Ctrl Pts',(1.46287516597445,3.81595420724559,54.2292306456731));
#8444=CARTESIAN_POINT('Ctrl Pts',(1.35007032822716,3.85545524015525,54.2350375012555));
#8445=CARTESIAN_POINT('Ctrl Pts',(1.23722855899427,3.89496920541655,54.2408462579604));
#8446=CARTESIAN_POINT('Ctrl Pts',(1.12269517896059,3.92950948642712,54.2466550146653));
#8447=CARTESIAN_POINT('Ctrl Pts',(1.00694739929703,3.95894959996322,54.2524637713702));
#8448=CARTESIAN_POINT('Ctrl Pts',(0.891072419772218,3.98842206641674,54.25827891155));
#8449=CARTESIAN_POINT('Ctrl Pts',(0.773980772256783,4.01278307757026,54.2640940517297));
#8450=CARTESIAN_POINT('Ctrl Pts',(0.656160491151446,4.0319571438511,54.2699091919095));
#8451=CARTESIAN_POINT('Ctrl Pts',(0.53826261007532,4.05114383874705,54.275728162115));
#8452=CARTESIAN_POINT('Ctrl Pts',(0.419635543697051,4.06513673733663,54.2815471323205));
#8453=CARTESIAN_POINT('Ctrl Pts',(0.300771453023509,4.07391231288133,54.2873661025261));
#8454=CARTESIAN_POINT('Ctrl Pts',(0.181740097042269,4.08270023739817,54.2931932611747));
#8455=CARTESIAN_POINT('Ctrl Pts',(0.0624714571839893,4.08625617385383,54.2990204198233));
#8456=CARTESIAN_POINT('Ctrl Pts',(-0.0565431931913263,4.08460865534309,
54.3048475784719));
#8457=CARTESIAN_POINT('Ctrl Pts',(-0.0825419396795343,4.08424875497822,
54.3061205210884));
#8458=CARTESIAN_POINT('Ctrl Pts',(-0.108528590220755,4.08364073970447,54.3073934637049));
#8459=CARTESIAN_POINT('Ctrl Pts',(-0.134498071919463,4.08278523420593,54.3086664063214));
#8460=CARTESIAN_POINT('Ctrl Pts',(-0.253368185723169,4.07886932871536,54.314493046816));
#8461=CARTESIAN_POINT('Ctrl Pts',(-0.372256320073657,4.06975153930717,54.3203196873106));
#8462=CARTESIAN_POINT('Ctrl Pts',(-0.490671232428501,4.05542436024482,54.3261463278052));
#8463=CARTESIAN_POINT('Ctrl Pts',(-0.608938006365209,4.04111510464835,54.3319656791055));
#8464=CARTESIAN_POINT('Ctrl Pts',(-0.726732334459119,4.0216094705717,54.3377850304058));
#8465=CARTESIAN_POINT('Ctrl Pts',(-0.843563949405264,3.99695194657927,54.3436043817061));
#8466=CARTESIAN_POINT('Ctrl Pts',(-0.960279759471247,3.97231886341659,54.3494179647965));
#8467=CARTESIAN_POINT('Ctrl Pts',(-1.07603435803646,3.94254413340492,54.3552315478869));
#8468=CARTESIAN_POINT('Ctrl Pts',(-1.19034416555116,3.90772386019513,54.3610451309773));
#8469=CARTESIAN_POINT('Ctrl Pts',(-1.3082163039442,3.87181845407204,54.3670398875558));
#8470=CARTESIAN_POINT('Ctrl Pts',(-1.42455168744414,3.83054792954459,54.3730346441343));
#8471=CARTESIAN_POINT('Ctrl Pts',(-1.53883273829007,3.78407436549107,54.3790294007129));
#8472=CARTESIAN_POINT('Ctrl Pts',(-1.64953737972976,3.73905518508553,54.3848365522278));
#8473=CARTESIAN_POINT('Ctrl Pts',(-1.75831394566974,3.68915393029484,54.3906437037427));
#8474=CARTESIAN_POINT('Ctrl Pts',(-1.864709496909,3.63456785493646,54.3964508552576));
#8475=CARTESIAN_POINT('Ctrl Pts',(-1.97108982315693,3.57998959073666,54.4022571757807));
#8476=CARTESIAN_POINT('Ctrl Pts',(-2.07508944957714,3.52072802535044,54.4080634963038));
#8477=CARTESIAN_POINT('Ctrl Pts',(-2.17627860618468,3.45702710840729,54.4138698168269));
#8478=CARTESIAN_POINT('Ctrl Pts',(-2.27747708720895,3.39332032152792,54.419676672393));
#8479=CARTESIAN_POINT('Ctrl Pts',(-2.37586423837257,3.32517358701314,54.4254835279591));
#8480=CARTESIAN_POINT('Ctrl Pts',(-2.47103847327306,3.25287470764005,54.4312903835252));
#8481=CARTESIAN_POINT('Ctrl Pts',(-2.56624386752803,3.18055215813803,54.4370991402137));
#8482=CARTESIAN_POINT('Ctrl Pts',(-2.65823392895141,3.10407500677429,54.4429078969023));
#8483=CARTESIAN_POINT('Ctrl Pts',(-2.74663991379978,3.02377151648763,54.4487166535908));
#8484=CARTESIAN_POINT('Ctrl Pts',(-2.83514305151773,2.94337977748647,54.4545317937542));
#8485=CARTESIAN_POINT('Ctrl Pts',(-2.92005394894313,2.85915358080764,54.4603469339175));
#8486=CARTESIAN_POINT('Ctrl Pts',(-3.00104042498547,2.77145834671983,54.4661620740809));
#8487=CARTESIAN_POINT('Ctrl Pts',(-3.08208024115021,2.68370535392035,54.47198104427));
#8488=CARTESIAN_POINT('Ctrl Pts',(-3.15919022558717,2.59247908405389,54.4778000144592));
#8489=CARTESIAN_POINT('Ctrl Pts',(-3.23207926232517,2.49817706379023,54.4836189846483));
#8490=CARTESIAN_POINT('Ctrl Pts',(-3.30507086836956,2.4037423419127,54.4894461432806));
#8491=CARTESIAN_POINT('Ctrl Pts',(-3.37382943801791,2.30622356340577,54.4952733019129));
#8492=CARTESIAN_POINT('Ctrl Pts',(-3.43810776735536,2.20604623252795,54.5011004605452));
#8493=CARTESIAN_POINT('Ctrl Pts',(-3.45214936805756,2.18416249513002,54.5023734033175));
#8494=CARTESIAN_POINT('Ctrl Pts',(-3.46597734689685,2.1621519781996,54.5036463460897));
#8495=CARTESIAN_POINT('Ctrl Pts',(-3.47958942653237,2.14001925756852,54.504919288862));
#8496=CARTESIAN_POINT('Ctrl Pts',(-3.54356996194138,2.03598935516193,54.5109024716155));
#8497=CARTESIAN_POINT('Ctrl Pts',(-3.60297137049294,1.92894186180992,54.516885654369));
#8498=CARTESIAN_POINT('Ctrl Pts',(-3.65750670425542,1.81930473212342,54.5228688371224));
#8499=CARTESIAN_POINT('Ctrl Pts',(-3.71196228215891,1.70982794258433,54.5288432696979));
#8500=CARTESIAN_POINT('Ctrl Pts',(-3.76156578514888,1.59776939164976,54.5348177022733));
#8501=CARTESIAN_POINT('Ctrl Pts',(-3.80607433331058,1.48358456763152,54.5407921348488));
#8502=CARTESIAN_POINT('Ctrl Pts',(-3.85190504303721,1.36600779326105,54.546944042661));
#8503=CARTESIAN_POINT('Ctrl Pts',(-3.89233313914355,1.24617677374807,54.5530959504732));
#8504=CARTESIAN_POINT('Ctrl Pts',(-3.92714445344491,1.12461613085394,54.5592478582854));
#8505=CARTESIAN_POINT('Ctrl Pts',(-3.96086078617512,1.00687914892803,54.5652062593078));
#8506=CARTESIAN_POINT('Ctrl Pts',(-3.98930823046686,0.887520109317343,54.5711646603301));
#8507=CARTESIAN_POINT('Ctrl Pts',(-4.01234118947697,0.767035318108995,54.5771230613525));
#8508=CARTESIAN_POINT('Ctrl Pts',(-4.03649618624754,0.640681177450641,54.5833717225597));
#8509=CARTESIAN_POINT('Ctrl Pts',(-4.05469572660276,0.513089233302163,54.5896203837668));
#8510=CARTESIAN_POINT('Ctrl Pts',(-4.06683129097684,0.384848347705532,54.595869044974));
#8511=CARTESIAN_POINT('Ctrl Pts',(-4.07896685535091,0.256607462108901,54.6021177061812));
#8512=CARTESIAN_POINT('Ctrl Pts',(-4.08503835513097,0.127718109681303,54.6083663673883));
#8513=CARTESIAN_POINT('Ctrl Pts',(-4.08499981754229,-0.00122093384916138,
54.6146150285955));
#8514=CARTESIAN_POINT('Ctrl Pts',(-4.08499981754213,-0.00122093438980094,
54.6146150286217));
#8515=CARTESIAN_POINT('Ctrl Pts',(-4.0849613114778,-0.130054446722099,54.6208585755618));
#8516=CARTESIAN_POINT('Ctrl Pts',(-4.0788238307835,-0.258718368127277,54.6271021225019));
#8517=CARTESIAN_POINT('Ctrl Pts',(-4.06666054896851,-0.386648392552093,
54.633345669442));
#8518=CARTESIAN_POINT('Ctrl Pts',(-4.05445122125751,-0.515062714939471,
54.6396128522493));
#8519=CARTESIAN_POINT('Ctrl Pts',(-4.03617046827928,-0.642737277144754,
54.6458800350566));
#8520=CARTESIAN_POINT('Ctrl Pts',(-4.01194308905835,-0.769114848482948,
54.6521472178638));
#8521=CARTESIAN_POINT('Ctrl Pts',(-3.98766880109497,-0.895737110461865,
54.6584265351105));
#8522=CARTESIAN_POINT('Ctrl Pts',(-3.95742496150907,-1.02105707251704,54.6647058523571));
#8523=CARTESIAN_POINT('Ctrl Pts',(-3.92138638497742,-1.14453214009642,54.6709851696037));
#8524=CARTESIAN_POINT('Ctrl Pts',(-3.88523988384411,-1.26837697803763,54.6772832915002));
#8525=CARTESIAN_POINT('Ctrl Pts',(-3.8432640256831,-1.39036558117875,54.6835814133967));
#8526=CARTESIAN_POINT('Ctrl Pts',(-3.79568276842705,-1.5099726227538,54.6898795352932));
#8527=CARTESIAN_POINT('Ctrl Pts',(-3.76724477624178,-1.58145842009854,54.6936437473296));
#8528=CARTESIAN_POINT('Ctrl Pts',(-3.73680536935565,-1.65209393914338,54.6974079593661));
#8529=CARTESIAN_POINT('Ctrl Pts',(-3.70442010209234,-1.72177138645471,54.7011721714026));
#8530=CARTESIAN_POINT('Ctrl Pts',(-3.65429334650934,-1.82961994433828,54.7069985163014));
#8531=CARTESIAN_POINT('Ctrl Pts',(-3.59937314424357,-1.93544927103489,54.7128248612001));
#8532=CARTESIAN_POINT('Ctrl Pts',(-3.53984483140051,-2.03880444614168,54.7186512060989));
#8533=CARTESIAN_POINT('Ctrl Pts',(-3.4803877596237,-2.14203592997411,54.7244705782648));
#8534=CARTESIAN_POINT('Ctrl Pts',(-3.41633374565396,-2.24279880006085,54.7302899504308));
#8535=CARTESIAN_POINT('Ctrl Pts',(-3.34791561976592,-2.34065930945265,54.7361093225967));
#8536=CARTESIAN_POINT('Ctrl Pts',(-3.27814446330158,-2.44045509929389,54.7420437781323));
#8537=CARTESIAN_POINT('Ctrl Pts',(-3.20383491891496,-2.53723212144727,54.7479782336679));
#8538=CARTESIAN_POINT('Ctrl Pts',(-3.12528286286086,-2.63055736054324,54.7539126892035));
#8539=CARTESIAN_POINT('Ctrl Pts',(-3.04838984166705,-2.72191155224996,54.759721807872));
#8540=CARTESIAN_POINT('Ctrl Pts',(-2.96743201131959,-2.80995798811599,54.7655309265405));
#8541=CARTESIAN_POINT('Ctrl Pts',(-2.8827296257502,-2.89432114749246,54.7713400452091));
#8542=CARTESIAN_POINT('Ctrl Pts',(-2.79528594698747,-2.98141462140509,54.7773371691782));
#8543=CARTESIAN_POINT('Ctrl Pts',(-2.70385149272671,-3.06458200391232,54.7833342931474));
#8544=CARTESIAN_POINT('Ctrl Pts',(-2.60882163596673,-3.14344948610787,54.7893314171166));
#8545=CARTESIAN_POINT('Ctrl Pts',(-2.51379177920677,-3.22231696830342,54.7953285410857));
#8546=CARTESIAN_POINT('Ctrl Pts',(-2.41516688168822,-3.29688423591414,54.8013256650549));
#8547=CARTESIAN_POINT('Ctrl Pts',(-2.31338095599002,-3.36682247118299,54.8073227890241));
#8548=CARTESIAN_POINT('',(-4.08499997893751,-0.000414825933522758,54.5103849713796));
#8549=CARTESIAN_POINT('Ctrl Pts',(-4.08499997893746,-0.000414826442725132,
54.5103849714045));
#8550=CARTESIAN_POINT('Ctrl Pts',(-4.08499760796101,-0.0237629974469017,
54.5115287470813));
#8551=CARTESIAN_POINT('Ctrl Pts',(-4.08479506611947,-0.0471099734563326,
54.5126725227581));
#8552=CARTESIAN_POINT('Ctrl Pts',(-4.08439240353752,-0.0704534876710844,
54.5138162984348));
#8553=CARTESIAN_POINT('Ctrl Pts',(-4.08234110579074,-0.189373149582664,
54.5196430739379));
#8554=CARTESIAN_POINT('Ctrl Pts',(-4.07508860521704,-0.308392412691008,
54.5254698494409));
#8555=CARTESIAN_POINT('Ctrl Pts',(-4.06261969266714,-0.427020178391096,
54.531296624944));
#8556=CARTESIAN_POINT('Ctrl Pts',(-4.05016644986693,-0.54549886393775,54.5371160779068));
#8557=CARTESIAN_POINT('Ctrl Pts',(-4.03250987681782,-0.663586628572482,
54.5429355308697));
#8558=CARTESIAN_POINT('Ctrl Pts',(-4.00968677161816,-0.780792541915143,
54.5487549838325));
#8559=CARTESIAN_POINT('Ctrl Pts',(-3.98688641878641,-0.897881612609194,
54.554568635379));
#8560=CARTESIAN_POINT('Ctrl Pts',(-3.95892985829082,-1.01409018293799,54.5603822869256));
#8561=CARTESIAN_POINT('Ctrl Pts',(-3.92590560378646,-1.12893320890038,54.5661959384721));
#8562=CARTESIAN_POINT('Ctrl Pts',(-3.89290572395898,-1.24369147105227,54.5720052990549));
#8563=CARTESIAN_POINT('Ctrl Pts',(-3.85484570588691,-1.35708580391272,54.5778146596377));
#8564=CARTESIAN_POINT('Ctrl Pts',(-3.81186484778546,-1.46864270066532,54.5836240202205));
#8565=CARTESIAN_POINT('Ctrl Pts',(-3.76890092317954,-1.58015564649891,54.5894310920454));
#8566=CARTESIAN_POINT('Ctrl Pts',(-3.72102016028149,-1.68983221586267,54.5952381638702));
#8567=CARTESIAN_POINT('Ctrl Pts',(-3.66841113396372,-1.79721583350776,54.601045235695));
#8568=CARTESIAN_POINT('Ctrl Pts',(-3.61581045826974,-1.90458240616543,54.6068513857641));
#8569=CARTESIAN_POINT('Ctrl Pts',(-3.55848319159784,-2.00965638510735,54.6126575358332));
#8570=CARTESIAN_POINT('Ctrl Pts',(-3.49666503069175,-2.11200347138385,54.6184636859023));
#8571=CARTESIAN_POINT('Ctrl Pts',(-3.4348421398624,-2.21435838859317,54.6242702802202));
#8572=CARTESIAN_POINT('Ctrl Pts',(-3.36852788294009,-2.31398564958607,54.6300768745381));
#8573=CARTESIAN_POINT('Ctrl Pts',(-3.29800233105639,-2.41047829783772,54.635883468856));
#8574=CARTESIAN_POINT('Ctrl Pts',(-3.2274156120223,-2.50705463462734,54.6416950992611));
#8575=CARTESIAN_POINT('Ctrl Pts',(-3.15261054266328,-2.60049059795527,54.6475067296662));
#8576=CARTESIAN_POINT('Ctrl Pts',(-3.07390881038207,-2.69041067970217,54.6533183600713));
#8577=CARTESIAN_POINT('Ctrl Pts',(-2.99517263341694,-2.78037011596775,54.6591325340007));
#8578=CARTESIAN_POINT('Ctrl Pts',(-2.91253667615821,-2.86681030866367,54.6649467079301));
#8579=CARTESIAN_POINT('Ctrl Pts',(-2.82635983936874,-2.94939232019132,54.6707608818596));
#8580=CARTESIAN_POINT('Ctrl Pts',(-2.74005896454961,-3.03209319556193,54.6765834243797));
#8581=CARTESIAN_POINT('Ctrl Pts',(-2.65020733296229,-3.11092452379591,54.6824059668999));
#8582=CARTESIAN_POINT('Ctrl Pts',(-2.5571976537131,-3.18558709814128,54.6882285094201));
#8583=CARTESIAN_POINT('Ctrl Pts',(-2.4781218381537,-3.24906440508164,54.6931787716092));
#8584=CARTESIAN_POINT('Ctrl Pts',(-2.39676397863391,-3.30952907413331,54.6981290337984));
#8585=CARTESIAN_POINT('Ctrl Pts',(-2.31338095599002,-3.36682247118298,54.7030792959875));
#8586=CARTESIAN_POINT('Ctrl Pts',(-2.31338095599002,-3.36682247118299,53.4530632234442));
#8587=CARTESIAN_POINT('Ctrl Pts',(-2.21483110028557,-3.43453716696917,53.458871188923));
#8588=CARTESIAN_POINT('Ctrl Pts',(-2.11333532917852,-3.49790096330531,53.4646791544019));
#8589=CARTESIAN_POINT('Ctrl Pts',(-2.00931967003337,-3.55666409204145,53.4704871198808));
#8590=CARTESIAN_POINT('Ctrl Pts',(-1.90519361781242,-3.6154895867961,53.4763012494236));
#8591=CARTESIAN_POINT('Ctrl Pts',(-1.79854269304458,-3.66970446364335,53.4821153789664));
#8592=CARTESIAN_POINT('Ctrl Pts',(-1.68981715296657,-3.71910513289688,53.4879295085092));
#8593=CARTESIAN_POINT('Ctrl Pts',(-1.58102771926253,-3.76853483293643,53.493747054782));
#8594=CARTESIAN_POINT('Ctrl Pts',(-1.47016161960171,-3.81314453778066,53.4995646010548));
#8595=CARTESIAN_POINT('Ctrl Pts',(-1.35768711150758,-3.85277960792545,53.5053821473277));
#8596=CARTESIAN_POINT('Ctrl Pts',(-1.24504420052336,-3.89247402183155,53.511208403944));
#8597=CARTESIAN_POINT('Ctrl Pts',(-1.13078846152099,-3.92717880812908,53.5170346605604));
#8598=CARTESIAN_POINT('Ctrl Pts',(-1.01540158357285,-3.95678968661183,53.5228609171768));
#8599=CARTESIAN_POINT('Ctrl Pts',(-0.951426222865082,-3.97320720882488,
53.5260912400284));
#8600=CARTESIAN_POINT('Ctrl Pts',(-0.887103309351932,-3.98805974644403,
53.52932156288));
#8601=CARTESIAN_POINT('Ctrl Pts',(-0.822515744067601,-4.00133638310514,
53.5325518857316));
#8602=CARTESIAN_POINT('Ctrl Pts',(-0.706017010642136,-4.02528389294484,
53.5383785261864));
#8603=CARTESIAN_POINT('Ctrl Pts',(-0.588286158508163,-4.04417751280474,
53.5442051666412));
#8604=CARTESIAN_POINT('Ctrl Pts',(-0.469799099151263,-4.05789524340349,
53.5500318070961));
#8605=CARTESIAN_POINT('Ctrl Pts',(-0.35146026844917,-4.07159581296571,53.5558511583576));
#8606=CARTESIAN_POINT('Ctrl Pts',(-0.232367513824851,-4.08013332601978,
53.5616705096192));
#8607=CARTESIAN_POINT('Ctrl Pts',(-0.113007938716276,-4.08343656811112,
53.5674898608808));
#8608=CARTESIAN_POINT('Ctrl Pts',(0.00623332579019821,-4.08673653599039,
53.5733034439335));
#8609=CARTESIAN_POINT('Ctrl Pts',(0.125740479250513,-4.08481254346311,53.5791170269863));
#8610=CARTESIAN_POINT('Ctrl Pts',(0.245020869434864,-4.07764512599385,53.584930610039));
#8611=CARTESIAN_POINT('Ctrl Pts',(0.368018493961781,-4.07025434431255,53.5909253666321));
#8612=CARTESIAN_POINT('Ctrl Pts',(0.490774551486939,-4.05728792303876,53.5969201232251));
#8613=CARTESIAN_POINT('Ctrl Pts',(0.612747926644611,-4.03878261093522,53.6029148798182));
#8614=CARTESIAN_POINT('Ctrl Pts',(0.730904161196627,-4.02085642012073,53.6087220312984));
#8615=CARTESIAN_POINT('Ctrl Pts',(0.848325537981576,-3.99773291183685,53.6145291827786));
#8616=CARTESIAN_POINT('Ctrl Pts',(0.964525580467868,-3.96949813006923,53.6203363342587));
#8617=CARTESIAN_POINT('Ctrl Pts',(1.08070899498276,-3.941267388637,53.6261426547483));
#8618=CARTESIAN_POINT('Ctrl Pts',(1.19567102660526,-3.90792692462295,53.6319489752378));
#8619=CARTESIAN_POINT('Ctrl Pts',(1.30893682451529,-3.86961359691479,53.6377552957274));
#8620=CARTESIAN_POINT('Ctrl Pts',(1.42221305970884,-3.83129673868752,53.6435621512612));
#8621=CARTESIAN_POINT('Ctrl Pts',(1.53379236409329,-3.78800623634791,53.6493690067949));
#8622=CARTESIAN_POINT('Ctrl Pts',(1.64321705206185,-3.73992817040824,53.6551758623287));
#8623=CARTESIAN_POINT('Ctrl Pts',(1.75267756490243,-3.69183436404847,53.6609846189861));
#8624=CARTESIAN_POINT('Ctrl Pts',(1.85998168524429,-3.63895004074933,53.6667933756435));
#8625=CARTESIAN_POINT('Ctrl Pts',(1.96469421522189,-3.58150829130321,53.6726021323009));
#8626=CARTESIAN_POINT('Ctrl Pts',(2.06952181802128,-3.52400341680225,53.6784172724352));
#8627=CARTESIAN_POINT('Ctrl Pts',(2.17175178805305,-3.46193131564877,53.6842324125695));
#8628=CARTESIAN_POINT('Ctrl Pts',(2.27097580354513,-3.39556974596496,53.6900475527038));
#8629=CARTESIAN_POINT('Ctrl Pts',(2.37026517097005,-3.32916446854745,53.695866522865));
#8630=CARTESIAN_POINT('Ctrl Pts',(2.46654431298234,-3.25846433685901,53.7016854930262));
#8631=CARTESIAN_POINT('Ctrl Pts',(2.55943734126607,-3.18378791632434,53.7075044631874));
#8632=CARTESIAN_POINT('Ctrl Pts',(2.6524610884637,-3.10900641125569,53.7133316217937));
#8633=CARTESIAN_POINT('Ctrl Pts',(2.74208890681506,-3.03023771809086,53.7191587803999));
#8634=CARTESIAN_POINT('Ctrl Pts',(2.82798107374755,-2.94783785960586,53.7249859390062));
#8635=CARTESIAN_POINT('Ctrl Pts',(2.8467442219051,-2.92983760640314,53.7262588820949));
#8636=CARTESIAN_POINT('Ctrl Pts',(2.86532925483141,-2.91166419900583,53.7275318251835));
#8637=CARTESIAN_POINT('Ctrl Pts',(2.88373288971329,-2.89332155502734,53.7288047682722));
#8638=CARTESIAN_POINT('Ctrl Pts',(2.96797181797925,-2.80936180032512,53.7346314086191));
#8639=CARTESIAN_POINT('Ctrl Pts',(3.04867504377748,-2.72158645576335,53.740458048966));
#8640=CARTESIAN_POINT('Ctrl Pts',(3.12547828030272,-2.63032517369164,53.7462846893129));
#8641=CARTESIAN_POINT('Ctrl Pts',(3.20218543505863,-2.53917806057751,53.752104040463));
#8642=CARTESIAN_POINT('Ctrl Pts',(3.2750020446252,-2.444553993408,53.757923391613));
#8643=CARTESIAN_POINT('Ctrl Pts',(3.34360000726998,-2.34681997421707,53.763742742763));
#8644=CARTESIAN_POINT('Ctrl Pts',(3.41212997477236,-2.24918283018534,53.7695563257007));
#8645=CARTESIAN_POINT('Ctrl Pts',(3.47644938138893,-2.14844219876397,53.7753699086384));
#8646=CARTESIAN_POINT('Ctrl Pts',(3.53627022838904,-2.04499825716534,53.7811834915762));
#8647=CARTESIAN_POINT('Ctrl Pts',(3.59795532401731,-1.938330602833,53.787178248211));
#8648=CARTESIAN_POINT('Ctrl Pts',(3.65485659782205,-1.82878872493102,53.7931730048459));
#8649=CARTESIAN_POINT('Ctrl Pts',(3.706706203894,-1.7168442323093,53.7991677614808));
#8650=CARTESIAN_POINT('Ctrl Pts',(3.75693318200392,-1.60840303079596,53.804974912838));
#8651=CARTESIAN_POINT('Ctrl Pts',(3.80241977601923,-1.49770774825449,53.8107820641953));
#8652=CARTESIAN_POINT('Ctrl Pts',(3.84296939715654,-1.3852116129019,53.8165892155525));
#8653=CARTESIAN_POINT('Ctrl Pts',(3.88351321571274,-1.27273157555301,53.8223955359164));
#8654=CARTESIAN_POINT('Ctrl Pts',(3.91912132817581,-1.158451581456,53.8282018562802));
#8655=CARTESIAN_POINT('Ctrl Pts',(3.94964594291672,-1.04284319319898,53.8340081766441));
#8656=CARTESIAN_POINT('Ctrl Pts',(3.98017337044418,-0.927224151843767,53.8398150320496));
#8657=CARTESIAN_POINT('Ctrl Pts',(4.0056162647757,-0.810276867263508,53.8456218874551));
#8658=CARTESIAN_POINT('Ctrl Pts',(4.02587735828219,-0.69248573708837,53.8514287428606));
#8659=CARTESIAN_POINT('Ctrl Pts',(4.04614508511947,-0.574656042976366,53.8572374993872));
#8660=CARTESIAN_POINT('Ctrl Pts',(4.06122756804862,-0.455982355514988,53.8630462559138));
#8661=CARTESIAN_POINT('Ctrl Pts',(4.07107915507459,-0.336956248075587,53.8688550124405));
#8662=CARTESIAN_POINT('Ctrl Pts',(4.08094156840191,-0.217799338106082,53.874670152441));
#8663=CARTESIAN_POINT('Ctrl Pts',(4.08556157816917,-0.0982896417554054,
53.8804852924415));
#8664=CARTESIAN_POINT('Ctrl Pts',(4.08494561455591,0.021079044579889,53.886300432442));
#8665=CARTESIAN_POINT('Ctrl Pts',(4.08432924525062,0.140526350698755,53.8921194024675));
#8666=CARTESIAN_POINT('Ctrl Pts',(4.0784700544374,0.259832055481758,53.897938372493));
#8667=CARTESIAN_POINT('Ctrl Pts',(4.06742640050331,0.378506904149321,53.9037573425185));
#8668=CARTESIAN_POINT('Ctrl Pts',(4.05636720596094,0.497348751832471,53.9095845009872));
#8669=CARTESIAN_POINT('Ctrl Pts',(4.04010904303405,0.615557569138881,53.915411659456));
#8670=CARTESIAN_POINT('Ctrl Pts',(4.01876146302421,0.732653603902604,53.9212388179247));
#8671=CARTESIAN_POINT('Ctrl Pts',(4.01409807857125,0.758233263412903,53.9225117622208));
#8672=CARTESIAN_POINT('Ctrl Pts',(4.00919201371126,0.783759877033307,53.9237847065168));
#8673=CARTESIAN_POINT('Ctrl Pts',(4.0040447251659,0.809228545511804,53.9250576508129));
#8674=CARTESIAN_POINT('Ctrl Pts',(3.98048407096562,0.925806134989238,53.9308842914046));
#8675=CARTESIAN_POINT('Ctrl Pts',(3.9517904716661,1.04153945104153,53.9367109319963));
#8676=CARTESIAN_POINT('Ctrl Pts',(3.91803793295716,1.15594279958342,53.942537572588));
#8677=CARTESIAN_POINT('Ctrl Pts',(3.88432761905494,1.27020302824562,53.9483569239866));
#8678=CARTESIAN_POINT('Ctrl Pts',(3.84557106839036,1.38313621100127,53.9541762753851));
#8679=CARTESIAN_POINT('Ctrl Pts',(3.80189340042581,1.49426623190069,53.9599956267837));
#8680=CARTESIAN_POINT('Ctrl Pts',(3.75825902627393,1.60528609943041,53.9658092099735));
#8681=CARTESIAN_POINT('Ctrl Pts',(3.70971338740881,1.71450598344587,53.9716227931632));
#8682=CARTESIAN_POINT('Ctrl Pts',(3.65643139642823,1.82146491682215,53.977436376353));
#8683=CARTESIAN_POINT('Ctrl Pts',(3.60148893606277,1.93175709715565,53.9834311328947));
#8684=CARTESIAN_POINT('Ctrl Pts',(3.54151020734356,2.03964467537803,53.9894258894364));
#8685=CARTESIAN_POINT('Ctrl Pts',(3.47674081996221,2.14464408954225,53.9954206459781));
#8686=CARTESIAN_POINT('Ctrl Pts',(3.41399837996478,2.24635756421471,54.0012277975943));
#8687=CARTESIAN_POINT('Ctrl Pts',(3.34676088525576,2.34536057575913,54.0070349492106));
#8688=CARTESIAN_POINT('Ctrl Pts',(3.27529792236496,2.44123913612571,54.0128421008269));
#8689=CARTESIAN_POINT('Ctrl Pts',(3.20384518567459,2.53710397647096,54.0186484214519));
#8690=CARTESIAN_POINT('Ctrl Pts',(3.12816842699467,2.62984492794562,54.0244547420769));
#8691=CARTESIAN_POINT('Ctrl Pts',(3.04857944346241,2.71907858968777,54.0302610627019));
#8692=CARTESIAN_POINT('Ctrl Pts',(2.96898312592808,2.8083204741742,54.0360679183704));
#8693=CARTESIAN_POINT('Ctrl Pts',(2.8854741382294,2.89405412199044,54.0418747740389));
#8694=CARTESIAN_POINT('Ctrl Pts',(2.79840285378173,2.97593119341599,54.0476816297074));
#8695=CARTESIAN_POINT('Ctrl Pts',(2.71130306282304,3.05783507080462,54.0534903864987));
#8696=CARTESIAN_POINT('Ctrl Pts',(2.62063895255242,3.13587958147787,54.0592991432899));
#8697=CARTESIAN_POINT('Ctrl Pts',(2.52679535449982,3.20975547923484,54.0651079000811));
#8698=CARTESIAN_POINT('Ctrl Pts',(2.43284862796809,3.28371256216736,54.0709230403472));
#8699=CARTESIAN_POINT('Ctrl Pts',(2.33571576002902,3.35349163592164,54.0767381806133));
#8700=CARTESIAN_POINT('Ctrl Pts',(2.23581216669383,3.41882566903664,54.0825533208794));
#8701=CARTESIAN_POINT('Ctrl Pts',(2.13584277385464,3.48420273310608,54.0883722911714));
#8702=CARTESIAN_POINT('Ctrl Pts',(2.03309937117241,3.54512871841213,54.0941912614633));
#8703=CARTESIAN_POINT('Ctrl Pts',(1.92802223191034,3.60138241141641,54.1000102317553));
#8704=CARTESIAN_POINT('Ctrl Pts',(1.822797228322,3.65771526449751,54.1058373904899));
#8705=CARTESIAN_POINT('Ctrl Pts',(1.71523230008273,3.70936252723781,54.1116645492244));
#8706=CARTESIAN_POINT('Ctrl Pts',(1.60578803419549,3.75615092737693,54.117491707959));
#8707=CARTESIAN_POINT('Ctrl Pts',(1.58187995360847,3.76637184513809,54.1187646497571));
#8708=CARTESIAN_POINT('Ctrl Pts',(1.55788224752409,3.77636108546979,54.1200375915553));
#8709=CARTESIAN_POINT('Ctrl Pts',(1.5337998058897,3.78611716081961,54.1213105333535));
#8710=CARTESIAN_POINT('Ctrl Pts',(1.42356717029867,3.83077367510339,54.127137173837));
#8711=CARTESIAN_POINT('Ctrl Pts',(1.31120722579543,3.87068314002797,54.1329638143204));
#8712=CARTESIAN_POINT('Ctrl Pts',(1.1971659072405,3.90563935746006,54.1387904548039));
#8713=CARTESIAN_POINT('Ctrl Pts',(1.08326725568749,3.94055184426187,54.144609806093));
#8714=CARTESIAN_POINT('Ctrl Pts',(0.967691800422726,3.97052329033378,54.1504291573822));
#8715=CARTESIAN_POINT('Ctrl Pts',(0.850905683399544,3.9953954144688,54.1562485086714));
#8716=CARTESIAN_POINT('Ctrl Pts',(0.734235326157389,4.0202428850601,54.1620620917507));
#8717=CARTESIAN_POINT('Ctrl Pts',(0.61635709116518,4.04000100490577,54.16787567483));
#8718=CARTESIAN_POINT('Ctrl Pts',(0.497751952524549,4.05456138118021,54.1736892579093));
#8719=CARTESIAN_POINT('Ctrl Pts',(0.375450623738313,4.06957551451712,54.179684014492));
#8720=CARTESIAN_POINT('Ctrl Pts',(0.252376765074173,4.07906250494079,54.1856787710747));
#8721=CARTESIAN_POINT('Ctrl Pts',(0.129069195615655,4.08296046303943,54.1916735276574));
#8722=CARTESIAN_POINT('Ctrl Pts',(0.00962051950209979,4.08673643507807,
54.1974806791613));
#8723=CARTESIAN_POINT('Ctrl Pts',(-0.110047020198127,4.08526796015158,54.2032878306652));
#8724=CARTESIAN_POINT('Ctrl Pts',(-0.229439408649957,4.07855152692207,54.2090949821692));
#8725=CARTESIAN_POINT('Ctrl Pts',(-0.348814712290411,4.07183605480069,54.2149013026814));
#8726=CARTESIAN_POINT('Ctrl Pts',(-0.467914535926838,4.05987414081413,54.2207076231936));
#8727=CARTESIAN_POINT('Ctrl Pts',(-0.586247092284356,4.04271435384546,54.2265139437057));
#8728=CARTESIAN_POINT('Ctrl Pts',(-0.704590552797133,4.02555298562995,54.2323207992611));
#8729=CARTESIAN_POINT('Ctrl Pts',(-0.822166201852386,4.00319285064147,54.2381276548164));
#8730=CARTESIAN_POINT('Ctrl Pts',(-0.938490216218402,3.97573403462333,54.2439345103717));
#8731=CARTESIAN_POINT('Ctrl Pts',(-1.05485231422392,3.94826622878778,54.2497432670494));
#8732=CARTESIAN_POINT('Ctrl Pts',(-1.16996156588243,3.91569651569341,54.2555520237272));
#8733=CARTESIAN_POINT('Ctrl Pts',(-1.28334774707571,3.87817528743553,54.2613607804049));
#8734=CARTESIAN_POINT('Ctrl Pts',(-1.39685853288007,3.84061282559871,54.2671759205578));
#8735=CARTESIAN_POINT('Ctrl Pts',(-1.5086420812892,3.79808811560402,54.2729910607107));
#8736=CARTESIAN_POINT('Ctrl Pts',(-1.61824650749295,3.75080034672427,54.2788062008636));
#8737=CARTESIAN_POINT('Ctrl Pts',(-1.72792312246141,3.70348143270066,54.2846251710423));
#8738=CARTESIAN_POINT('Ctrl Pts',(-1.83541739071912,3.65139338944626,54.290444141221));
#8739=CARTESIAN_POINT('Ctrl Pts',(-1.94030193146339,3.59478141404445,54.2962631113997));
#8740=CARTESIAN_POINT('Ctrl Pts',(-2.04533406552763,3.53808977438192,54.3020902700218));
#8741=CARTESIAN_POINT('Ctrl Pts',(-2.14774879391313,3.47686170553716,54.3079174286439));
#8742=CARTESIAN_POINT('Ctrl Pts',(-2.24714751724139,3.41138579403676,54.3137445872661));
#8743=CARTESIAN_POINT('Ctrl Pts',(-2.26886116963209,3.39708258032658,54.3150175301421));
#8744=CARTESIAN_POINT('Ctrl Pts',(-2.29043102323381,3.38257680976385,54.3162904730181));
#8745=CARTESIAN_POINT('Ctrl Pts',(-2.31185313982904,3.36787174041154,54.3175634158941));
#8746=CARTESIAN_POINT('Ctrl Pts',(-2.40962137593576,3.30075938547629,54.3233729902702));
#8747=CARTESIAN_POINT('Ctrl Pts',(-2.50462505378427,3.22927620521925,54.3291825646463));
#8748=CARTESIAN_POINT('Ctrl Pts',(-2.59644759805791,3.15367799093999,54.3349921390224));
#8749=CARTESIAN_POINT('Ctrl Pts',(-2.68815504986841,3.07817453318005,54.340794431546));
#8750=CARTESIAN_POINT('Ctrl Pts',(-2.77668898388059,2.99856655800571,54.3465967240695));
#8751=CARTESIAN_POINT('Ctrl Pts',(-2.86166152162032,2.91515322679232,54.3523990165931));
#8752=CARTESIAN_POINT('Ctrl Pts',(-2.94654999687871,2.83182241555285,54.3581955689668));
#8753=CARTESIAN_POINT('Ctrl Pts',(-3.0278837930395,2.74469402282852,54.3639921213404));
#8754=CARTESIAN_POINT('Ctrl Pts',(-3.10530837555256,2.65410717430987,54.3697886737141));
#8755=CARTESIAN_POINT('Ctrl Pts',(-3.18355610618591,2.56255724156576,54.3756468527835));
#8756=CARTESIAN_POINT('Ctrl Pts',(-3.25781068237893,2.46747515130599,54.3815050318528));
#8757=CARTESIAN_POINT('Ctrl Pts',(-3.32774444873561,2.36924922368022,54.3873632109222));
#8758=CARTESIAN_POINT('Ctrl Pts',(-3.39686760748384,2.27216184025747,54.3931534873922));
#8759=CARTESIAN_POINT('Ctrl Pts',(-3.46176935901469,2.17200346539132,54.3989437638621));
#8760=CARTESIAN_POINT('Ctrl Pts',(-3.5221744930545,2.0691814421351,54.4047340403321));
#8761=CARTESIAN_POINT('Ctrl Pts',(-3.5825715191737,1.96637322023558,54.4105235395982));
#8762=CARTESIAN_POINT('Ctrl Pts',(-3.63847292019524,1.86090241487841,54.4163130388643));
#8763=CARTESIAN_POINT('Ctrl Pts',(-3.68964809220262,1.75320334123158,54.4221025381304));
#8764=CARTESIAN_POINT('Ctrl Pts',(-3.74082863267413,1.64549296955503,54.4278926447363));
#8765=CARTESIAN_POINT('Ctrl Pts',(-3.7872817823887,1.53555423576914,54.4336827513422));
#8766=CARTESIAN_POINT('Ctrl Pts',(-3.82882426433602,1.42384330346836,54.4394728579481));
#8767=CARTESIAN_POINT('Ctrl Pts',(-3.87122223430697,1.3098318980083,54.4453822007341));
#8768=CARTESIAN_POINT('Ctrl Pts',(-3.90850489483918,1.19397491631519,54.45129154352));
#8769=CARTESIAN_POINT('Ctrl Pts',(-3.94053066445184,1.07677438793591,54.457200886306));
#8770=CARTESIAN_POINT('Ctrl Pts',(-3.97195588228142,0.961771620520624,54.4629994162562));
#8771=CARTESIAN_POINT('Ctrl Pts',(-3.99831961112235,0.845475672892513,54.4687979462064));
#8772=CARTESIAN_POINT('Ctrl Pts',(-4.01953987707944,0.728370905904543,54.4745964761567));
#8773=CARTESIAN_POINT('Ctrl Pts',(-4.04136843803518,0.607909242060507,54.4805612253605));
#8774=CARTESIAN_POINT('Ctrl Pts',(-4.05775414418478,0.486592157322449,54.4865259745643));
#8775=CARTESIAN_POINT('Ctrl Pts',(-4.0686651095036,0.36495099220038,54.4924907237681));
#8776=CARTESIAN_POINT('Ctrl Pts',(-4.07957607482243,0.24330982707832,54.4984554729719));
#8777=CARTESIAN_POINT('Ctrl Pts',(-4.0850123434796,0.121345049922239,54.5044202221757));
#8778=CARTESIAN_POINT('Ctrl Pts',(-4.08499997893751,-0.000414825933535863,
54.5103849713796));
#8779=CARTESIAN_POINT('Origin',(0.,0.,46.4896150285955));
#8780=CARTESIAN_POINT('',(-2.31338095599002,-3.36682247118298,52.2032272635689));
#8781=CARTESIAN_POINT('',(-2.31338095599003,-3.36682247118298,52.3072351639912));
#8782=CARTESIAN_POINT('',(-2.31338095599002,-3.36682247118298,46.4896150285955));
#8783=CARTESIAN_POINT('',(-4.08499863636843,0.00333779389427079,53.3646150286363));
#8784=CARTESIAN_POINT('Ctrl Pts',(-2.31338095599003,-3.36682247118298,52.3072351639912));
#8785=CARTESIAN_POINT('Ctrl Pts',(-2.21493144244683,-3.43446822076041,52.3130540845183));
#8786=CARTESIAN_POINT('Ctrl Pts',(-2.11360661907073,-3.49772756075896,52.3188730050453));
#8787=CARTESIAN_POINT('Ctrl Pts',(-2.00984156052795,-3.55636920209004,52.3246919255724));
#8788=CARTESIAN_POINT('Ctrl Pts',(-1.90593025909387,-3.61509349092598,52.3305190470852));
#8789=CARTESIAN_POINT('Ctrl Pts',(-1.79957222056283,-3.66918690786224,52.336346168598));
#8790=CARTESIAN_POINT('Ctrl Pts',(-1.69122393906574,-3.71846562279806,52.3421732901108));
#8791=CARTESIAN_POINT('Ctrl Pts',(-1.66665354039674,-3.72964067472449,52.3434947203788));
#8792=CARTESIAN_POINT('Ctrl Pts',(-1.64198085808676,-3.74056832863762,52.3448161506469));
#8793=CARTESIAN_POINT('Ctrl Pts',(-1.61721132365331,-3.75124679735252,52.3461375809149));
#8794=CARTESIAN_POINT('Ctrl Pts',(-1.50799383531472,-3.79833187823997,52.3519642263563));
#8795=CARTESIAN_POINT('Ctrl Pts',(-1.39654450508684,-3.84071813988266,52.3577908717977));
#8796=CARTESIAN_POINT('Ctrl Pts',(-1.28330459644759,-3.87818956637456,52.363617517239));
#8797=CARTESIAN_POINT('Ctrl Pts',(-1.17020635109364,-3.91561411605911,52.3694368735387));
#8798=CARTESIAN_POINT('Ctrl Pts',(-1.05532236665007,-3.94813593315012,52.3752562298384));
#8799=CARTESIAN_POINT('Ctrl Pts',(-0.939115169065273,-3.97558645978571,
52.3810755861381));
#8800=CARTESIAN_POINT('Ctrl Pts',(-0.823023156410561,-4.00300977737525,
52.3868891742741));
#8801=CARTESIAN_POINT('Ctrl Pts',(-0.705610934579691,-4.02537171157905,
52.39270276241));
#8802=CARTESIAN_POINT('Ctrl Pts',(-0.587356961998321,-4.04255325248686,
52.3985163505459));
#8803=CARTESIAN_POINT('Ctrl Pts',(-0.465417887214954,-4.06027021502028,
52.4045111052505));
#8804=CARTESIAN_POINT('Ctrl Pts',(-0.342584159196125,-4.0724784877694,52.4105058599551));
#8805=CARTESIAN_POINT('Ctrl Pts',(-0.219393094396066,-4.07910427301526,
52.4165006146596));
#8806=CARTESIAN_POINT('Ctrl Pts',(-0.100057133964627,-4.08552271291761,
52.4223077713019));
#8807=CARTESIAN_POINT('Ctrl Pts',(0.0196136949359783,-4.08670282490637,
52.4281149279442));
#8808=CARTESIAN_POINT('Ctrl Pts',(0.139125575425362,-4.08263016623629,52.4339220845864));
#8809=CARTESIAN_POINT('Ctrl Pts',(0.258620354455936,-4.07855809034011,52.4397284102581));
#8810=CARTESIAN_POINT('Ctrl Pts',(0.377955822841558,-4.06923475253925,52.4455347359299));
#8811=CARTESIAN_POINT('Ctrl Pts',(0.496639238214287,-4.05469782685047,52.4513410616016));
#8812=CARTESIAN_POINT('Ctrl Pts',(0.615333590380842,-4.04015956156965,52.457147922332));
#8813=CARTESIAN_POINT('Ctrl Pts',(0.733375365265743,-4.02040680275784,52.4629547830624));
#8814=CARTESIAN_POINT('Ctrl Pts',(0.850278642547521,-3.99552890491704,52.4687616437927));
#8815=CARTESIAN_POINT('Ctrl Pts',(0.967220193279139,-3.97064286219786,52.4745704056554));
#8816=CARTESIAN_POINT('Ctrl Pts',(1.08302210643856,-3.94062842817693,52.480379167518));
#8817=CARTESIAN_POINT('Ctrl Pts',(1.19721094421841,-3.90562555233392,52.4861879293807));
#8818=CARTESIAN_POINT('Ctrl Pts',(1.31152526834388,-3.87058421053346,52.492003074707));
#8819=CARTESIAN_POINT('Ctrl Pts',(1.42422258870311,-3.8305436043431,52.4978182200333));
#8820=CARTESIAN_POINT('Ctrl Pts',(1.53484672242706,-3.78569287431705,52.5036333653596));
#8821=CARTESIAN_POINT('Ctrl Pts',(1.64554371644493,-3.74081260428683,52.509452340711));
#8822=CARTESIAN_POINT('Ctrl Pts',(1.75416443444624,-3.69111607020024,52.5152713160623));
#8823=CARTESIAN_POINT('Ctrl Pts',(1.86027617340527,-3.63683895143305,52.5210902914136));
#8824=CARTESIAN_POINT('Ctrl Pts',(1.96653723173567,-3.58248545445046,52.5269174551685));
#8825=CARTESIAN_POINT('Ctrl Pts',(2.07028191132472,-3.52353870894868,52.5327446189234));
#8826=CARTESIAN_POINT('Ctrl Pts',(2.17110532330159,-3.4602784100606,52.5385717826783));
#8827=CARTESIAN_POINT('Ctrl Pts',(2.19312932682573,-3.44645974415422,52.5398446762707));
#8828=CARTESIAN_POINT('Ctrl Pts',(2.21501406010772,-3.43243540469784,52.5411175698632));
#8829=CARTESIAN_POINT('Ctrl Pts',(2.23675551426093,-3.41820856142853,52.5423904634556));
#8830=CARTESIAN_POINT('Ctrl Pts',(2.33627651339756,-3.35308551828965,52.5482171041771));
#8831=CARTESIAN_POINT('Ctrl Pts',(2.43310945763141,-3.28350890485543,52.5540437448986));
#8832=CARTESIAN_POINT('Ctrl Pts',(2.52683075548952,-3.20972761042308,52.5598703856202));
#8833=CARTESIAN_POINT('Ctrl Pts',(2.6204348071879,-3.13603861703254,52.5656897371634));
#8834=CARTESIAN_POINT('Ctrl Pts',(2.71093463758183,-3.05815565528383,52.5715090887067));
#8835=CARTESIAN_POINT('Ctrl Pts',(2.79793451014694,-2.97637152871223,52.5773284402499));
#8836=CARTESIAN_POINT('Ctrl Pts',(2.88484814764639,-2.89466846731139,52.5831420235989));
#8837=CARTESIAN_POINT('Ctrl Pts',(2.96826843360688,-2.80907221176675,52.5889556069479));
#8838=CARTESIAN_POINT('Ctrl Pts',(3.04783216983345,-2.71991618704112,52.594769190297));
#8839=CARTESIAN_POINT('Ctrl Pts',(3.12987541154458,-2.62798172501764,52.6007639467844));
#8840=CARTESIAN_POINT('Ctrl Pts',(3.20781744996931,-2.53226226087349,52.6067587032719));
#8841=CARTESIAN_POINT('Ctrl Pts',(3.28130032850117,-2.43316525418601,52.6127534597594));
#8842=CARTESIAN_POINT('Ctrl Pts',(3.35248357540003,-2.33716946802593,52.6185606115704));
#8843=CARTESIAN_POINT('Ctrl Pts',(3.41948233654224,-2.23800473731128,52.6243677633814));
#8844=CARTESIAN_POINT('Ctrl Pts',(3.482012159524,-2.13607498017439,52.6301749151925));
#8845=CARTESIAN_POINT('Ctrl Pts',(3.54453303475801,-2.03415980874575,52.6359812360251));
#8846=CARTESIAN_POINT('Ctrl Pts',(3.6025860304528,-1.92948074531676,52.6417875568578));
#8847=CARTESIAN_POINT('Ctrl Pts',(3.65593075681061,-1.82246956117411,52.6475938776905));
#8848=CARTESIAN_POINT('Ctrl Pts',(3.70928039891937,-1.71544851588181,52.6534007335794));
#8849=CARTESIAN_POINT('Ctrl Pts',(3.75792072710644,-1.60609528758058,52.6592075894682));
#8850=CARTESIAN_POINT('Ctrl Pts',(3.80165822082893,-1.49486446609844,52.6650144453571));
#8851=CARTESIAN_POINT('Ctrl Pts',(3.84541003398569,-1.38359722820785,52.6708232023813));
#8852=CARTESIAN_POINT('Ctrl Pts',(3.88425567115322,-1.27045155390415,52.6766319594054));
#8853=CARTESIAN_POINT('Ctrl Pts',(3.91805069814696,-1.1558995314257,52.6824407164295));
#8854=CARTESIAN_POINT('Ctrl Pts',(3.95188286394642,-1.04122162281288,52.6882558569461));
#8855=CARTESIAN_POINT('Ctrl Pts',(3.98065322554323,-0.925134672530824,52.6940709974626));
#8856=CARTESIAN_POINT('Ctrl Pts',(4.00426789676726,-0.808123512168205,52.6998861379792));
#8857=CARTESIAN_POINT('Ctrl Pts',(4.02789812136444,-0.691035284535784,52.7057051085322));
#8858=CARTESIAN_POINT('Ctrl Pts',(4.04636582989237,-0.57302203647665,52.7115240790851));
#8859=CARTESIAN_POINT('Ctrl Pts',(4.05962890585733,-0.454574687733093,52.7173430496381));
#8860=CARTESIAN_POINT('Ctrl Pts',(4.07291064562427,-0.335960659867111,52.723170208647));
#8861=CARTESIAN_POINT('Ctrl Pts',(4.08097310808659,-0.216911717493788,52.728997367656));
#8862=CARTESIAN_POINT('Ctrl Pts',(4.08382623292447,-0.0979198615089626,
52.734824526665));
#8863=CARTESIAN_POINT('Ctrl Pts',(4.08444949652334,-0.0719261540439095,
52.736097466442));
#8864=CARTESIAN_POINT('Ctrl Pts',(4.08482436641676,-0.0459351536481145,
52.7373704062191));
#8865=CARTESIAN_POINT('Ctrl Pts',(4.08495127505391,-0.0199519531724785,
52.7386433459962));
#8866=CARTESIAN_POINT('Ctrl Pts',(4.08553217514419,0.0989811930683613,52.7444699851281));
#8867=CARTESIAN_POINT('Ctrl Pts',(4.08091559422358,0.218129010432613,52.75029662426));
#8868=CARTESIAN_POINT('Ctrl Pts',(4.0710754597632,0.337000891562378,52.7561232633919));
#8869=CARTESIAN_POINT('Ctrl Pts',(4.06124763546442,0.455724062115895,52.7619426133074));
#8870=CARTESIAN_POINT('Ctrl Pts',(4.04620928887724,0.574171580131339,52.7677619632229));
#8871=CARTESIAN_POINT('Ctrl Pts',(4.02598634147149,0.691851847063394,52.7735813131384));
#8872=CARTESIAN_POINT('Ctrl Pts',(4.00578343936559,0.809415467485428,52.7793948948238));
#8873=CARTESIAN_POINT('Ctrl Pts',(3.98040622898983,0.926212950150694,52.7852084765092));
#8874=CARTESIAN_POINT('Ctrl Pts',(3.94993246284014,1.04175742810004,52.7910220581946));
#8875=CARTESIAN_POINT('Ctrl Pts',(3.91850900724911,1.16090275309187,52.7970168152922));
#8876=CARTESIAN_POINT('Ctrl Pts',(3.88166616893103,1.27871525635869,52.8030115723898));
#8877=CARTESIAN_POINT('Ctrl Pts',(3.83954634323955,1.39467160224758,52.8090063294874));
#8878=CARTESIAN_POINT('Ctrl Pts',(3.7987446652614,1.50699907290559,52.814813479556));
#8879=CARTESIAN_POINT('Ctrl Pts',(3.75299151228405,1.61758441980801,52.8206206296246));
#8880=CARTESIAN_POINT('Ctrl Pts',(3.70246687307412,1.72596757031781,52.8264277796931));
#8881=CARTESIAN_POINT('Ctrl Pts',(3.65194946395254,1.834335211172,52.8322340987571));
#8882=CARTESIAN_POINT('Ctrl Pts',(3.59666209881831,1.94050091284881,52.8380404178211));
#8883=CARTESIAN_POINT('Ctrl Pts',(3.53683230480951,2.04402598996584,52.8438467368851));
#8884=CARTESIAN_POINT('Ctrl Pts',(3.47699699769631,2.14756060655342,52.8496535909809));
#8885=CARTESIAN_POINT('Ctrl Pts',(3.41261863355883,2.24845376169357,52.8554604450767));
#8886=CARTESIAN_POINT('Ctrl Pts',(3.34396962684773,2.3462932755135,52.8612672991724));
#8887=CARTESIAN_POINT('Ctrl Pts',(3.2752981450587,2.44416482112533,52.8670760543809));
#8888=CARTESIAN_POINT('Ctrl Pts',(3.20235347410291,2.53898040347634,52.8728848095894));
#8889=CARTESIAN_POINT('Ctrl Pts',(3.12544970132398,2.63035913222773,52.8786935647979));
#8890=CARTESIAN_POINT('Ctrl Pts',(3.04846141598508,2.72183828063364,52.8845087034744));
#8891=CARTESIAN_POINT('Ctrl Pts',(2.96750560724484,2.80987272450696,52.8903238421509));
#8892=CARTESIAN_POINT('Ctrl Pts',(2.88293487550622,2.89411670524703,52.8961389808274));
#8893=CARTESIAN_POINT('Ctrl Pts',(2.79830844301607,2.97841617153089,52.9019579495239));
#8894=CARTESIAN_POINT('Ctrl Pts',(2.71006264636445,3.05891992849812,52.9077769182204));
#8895=CARTESIAN_POINT('Ctrl Pts',(2.61858372191455,3.13532203949198,52.9135958869169));
#8896=CARTESIAN_POINT('Ctrl Pts',(2.52697606842891,3.21183166344728,52.9194230440593));
#8897=CARTESIAN_POINT('Ctrl Pts',(2.4321265298229,3.28422787539933,52.9252502012018));
#8898=CARTESIAN_POINT('Ctrl Pts',(2.33445096018978,3.3522475616322,52.9310773583442));
#8899=CARTESIAN_POINT('Ctrl Pts',(2.3131134930913,3.36710662846431,52.9323503150751));
#8900=CARTESIAN_POINT('Ctrl Pts',(2.29164125791616,3.38175701461162,52.933623271806));
#8901=CARTESIAN_POINT('Ctrl Pts',(2.27003874127722,3.39619627128653,52.9348962285368));
#8902=CARTESIAN_POINT('Ctrl Pts',(2.17115862198715,3.46228835890476,52.9407228697334));
#8903=CARTESIAN_POINT('Ctrl Pts',(2.06923234116559,3.52416371376206,52.94654951093));
#8904=CARTESIAN_POINT('Ctrl Pts',(1.96465472573961,3.58152995361326,52.9523761521266));
#8905=CARTESIAN_POINT('Ctrl Pts',(1.86020793795112,3.63882442772759,52.958195504137));
#8906=CARTESIAN_POINT('Ctrl Pts',(1.75311676738121,3.69162081248238,52.9640148561475));
#8907=CARTESIAN_POINT('Ctrl Pts',(1.64380554930374,3.73966954637415,52.969834208158));
#8908=CARTESIAN_POINT('Ctrl Pts',(1.53460268164954,3.78767065385807,52.9756477919658));
#8909=CARTESIAN_POINT('Ctrl Pts',(1.42318451557263,3.83093330946312,52.9814613757737));
#8910=CARTESIAN_POINT('Ctrl Pts',(1.31000003150605,3.86925379336302,52.9872749595816));
#8911=CARTESIAN_POINT('Ctrl Pts',(1.19328830553101,3.90876848349958,52.9932697158939));
#8912=CARTESIAN_POINT('Ctrl Pts',(1.07469875546949,3.94302771155996,52.9992644722062));
#8913=CARTESIAN_POINT('Ctrl Pts',(0.954746438207526,3.97186155835397,53.0052592285186));
#8914=CARTESIAN_POINT('Ctrl Pts',(0.838547992052256,3.99979305872529,53.0110663807643));
#8915=CARTESIAN_POINT('Ctrl Pts',(0.721071227025833,4.02263358284084,53.0168735330101));
#8916=CARTESIAN_POINT('Ctrl Pts',(0.602799171696235,4.04027946540859,53.0226806852558));
#8917=CARTESIAN_POINT('Ctrl Pts',(0.484544040784918,4.05792282289722,53.0284870065135));
#8918=CARTESIAN_POINT('Ctrl Pts',(0.365494249146629,4.07037295703365,53.0342933277711));
#8919=CARTESIAN_POINT('Ctrl Pts',(0.246141210279892,4.07757765157231,53.0400996490288));
#8920=CARTESIAN_POINT('Ctrl Pts',(0.126777173166066,4.08478301001539,53.0459065053323));
#8921=CARTESIAN_POINT('Ctrl Pts',(0.00711024035019893,4.08674194324849,
53.0517133616359));
#8922=CARTESIAN_POINT('Ctrl Pts',(-0.112365521214941,4.08345429625974,53.0575202179394));
#8923=CARTESIAN_POINT('Ctrl Pts',(-0.231880398314553,4.08016557291819,53.0633289753674));
#8924=CARTESIAN_POINT('Ctrl Pts',(-0.351203572249954,4.0716268643931,53.0691377327954));
#8925=CARTESIAN_POINT('Ctrl Pts',(-0.469844086081757,4.05789003483017,53.0749464902233));
#8926=CARTESIAN_POINT('Ctrl Pts',(-0.588614978687084,4.04413810931955,53.0807616311256));
#8927=CARTESIAN_POINT('Ctrl Pts',(-0.706701308455423,4.02517670759286,53.0865767720278));
#8928=CARTESIAN_POINT('Ctrl Pts',(-0.823620176257923,4.0011091968679,53.0923919129301));
#8929=CARTESIAN_POINT('Ctrl Pts',(-0.940616050333473,3.97702583455852,53.0982108838586));
#8930=CARTESIAN_POINT('Ctrl Pts',(-1.05644253656456,3.94782976495233,53.104029854787));
#8931=CARTESIAN_POINT('Ctrl Pts',(-1.17063139603742,3.9136743776931,53.1098488257155));
#8932=CARTESIAN_POINT('Ctrl Pts',(-1.28498094172898,3.87947092707592,53.1156759850823));
#8933=CARTESIAN_POINT('Ctrl Pts',(-1.39768787761184,3.840294363912,53.1215031444491));
#8934=CARTESIAN_POINT('Ctrl Pts',(-1.5083033446677,3.79634640417129,53.1273303038159));
#8935=CARTESIAN_POINT('Ctrl Pts',(-1.53246715658383,3.78674602674182,53.1286032395698));
#8936=CARTESIAN_POINT('Ctrl Pts',(-1.55653125664943,3.77691813330193,53.1298761753236));
#8937=CARTESIAN_POINT('Ctrl Pts',(-1.58049112762186,3.76686511512008,53.1311491110775));
#8938=CARTESIAN_POINT('Ctrl Pts',(-1.69016324034444,3.72084918521332,53.1369757515317));
#8939=CARTESIAN_POINT('Ctrl Pts',(-1.79799860007571,3.66996640222913,53.1428023919859));
#8940=CARTESIAN_POINT('Ctrl Pts',(-1.90353553495269,3.61438479788364,53.1486290324401));
#8941=CARTESIAN_POINT('Ctrl Pts',(-2.00894044192748,3.55887272675542,53.154448383701));
#8942=CARTESIAN_POINT('Ctrl Pts',(-2.11205228553337,3.49867371481663,53.160267734962));
#8943=CARTESIAN_POINT('Ctrl Pts',(-2.21242883229364,3.43400402766738,53.1660870862229));
#8944=CARTESIAN_POINT('Ctrl Pts',(-2.31270588465065,3.36939844186591,53.171900669275));
#8945=CARTESIAN_POINT('Ctrl Pts',(-2.4102526931584,3.30033121648047,53.1777142523271));
#8946=CARTESIAN_POINT('Ctrl Pts',(-2.5046516651484,3.22706446112707,53.1835278353793));
#8947=CARTESIAN_POINT('Ctrl Pts',(-2.60199247109591,3.15151443272195,53.1895225919725));
#8948=CARTESIAN_POINT('Ctrl Pts',(-2.69598563869675,3.07149904554205,53.1955173485658));
#8949=CARTESIAN_POINT('Ctrl Pts',(-2.78620531770213,2.98735416842536,53.2015121051591));
#8950=CARTESIAN_POINT('Ctrl Pts',(-2.87360158380063,2.90584259409493,53.2073192566387));
#8951=CARTESIAN_POINT('Ctrl Pts',(-2.95745670070888,2.82045643756548,53.2131264081182));
#8952=CARTESIAN_POINT('Ctrl Pts',(-3.0374177477781,2.73154140101932,53.2189335595978));
#8953=CARTESIAN_POINT('Ctrl Pts',(-3.11736735259683,2.64263908801991,53.2247398800868));
#8954=CARTESIAN_POINT('Ctrl Pts',(-3.1934237231818,2.55020920245243,53.2305462005757));
#8955=CARTESIAN_POINT('Ctrl Pts',(-3.26527222642084,2.45463282129216,53.2363525210646));
#8956=CARTESIAN_POINT('Ctrl Pts',(-3.3371273503981,2.35904763290318,53.2421593765978));
#8957=CARTESIAN_POINT('Ctrl Pts',(-3.40477359103225,2.26031569842973,53.2479662321309));
#8958=CARTESIAN_POINT('Ctrl Pts',(-3.46793827504224,2.15884902679577,53.2537730876641));
#8959=CARTESIAN_POINT('Ctrl Pts',(-3.53112363872488,2.05734913568818,53.2595818443209));
#8960=CARTESIAN_POINT('Ctrl Pts',(-3.58982431233119,1.95311307279088,53.2653906009777));
#8961=CARTESIAN_POINT('Ctrl Pts',(-3.64381272664073,1.84657894853457,53.2711993576344));
#8962=CARTESIAN_POINT('Ctrl Pts',(-3.69786047099602,1.73992774963277,53.2770144977681));
#8963=CARTESIAN_POINT('Ctrl Pts',(-3.74718543523956,1.63097381251409,53.2828296379019));
#8964=CARTESIAN_POINT('Ctrl Pts',(-3.79160745312437,1.52017693753448,53.2886447780356));
#8965=CARTESIAN_POINT('Ctrl Pts',(-3.83605872869159,1.40930708838725,53.2944637481962));
#8966=CARTESIAN_POINT('Ctrl Pts',(-3.87560049196883,1.29659226788354,53.3002827183568));
#8967=CARTESIAN_POINT('Ctrl Pts',(-3.91010238680603,1.18250764255196,53.3061016885174));
#8968=CARTESIAN_POINT('Ctrl Pts',(-3.94465283265201,1.0682624775262,53.3119288471231));
#8969=CARTESIAN_POINT('Ctrl Pts',(-3.97414915509558,0.952644054234602,53.3177560057288));
#8970=CARTESIAN_POINT('Ctrl Pts',(-3.99851199692488,0.836138033130776,53.3235831643345));
#8971=CARTESIAN_POINT('Ctrl Pts',(-4.00383406096464,0.810687286880546,53.324856107429));
#8972=CARTESIAN_POINT('Ctrl Pts',(-4.00891134974107,0.785194202913159,53.3261290505236));
#8973=CARTESIAN_POINT('Ctrl Pts',(-4.013743365907,0.759663868192736,53.3274019936181));
#8974=CARTESIAN_POINT('Ctrl Pts',(-4.0458370446992,0.590094410261053,53.3358567308113));
#8975=CARTESIAN_POINT('Ctrl Pts',(-4.06719182948094,0.418433988893306,53.3443114680044));
#8976=CARTESIAN_POINT('Ctrl Pts',(-4.07759833749446,0.245798287346335,53.3527662051976));
#8977=CARTESIAN_POINT('Ctrl Pts',(-4.08245970979669,0.165151982477693,53.3567158129969));
#8978=CARTESIAN_POINT('Ctrl Pts',(-4.08493248888153,0.0842931598013199,
53.3606654207962));
#8979=CARTESIAN_POINT('Ctrl Pts',(-4.08499863636774,0.00333779473110509,
53.3646150285955));
#8980=CARTESIAN_POINT('Ctrl Pts',(-4.08499863636843,0.00333779389426807,
53.3646150286363));
#8981=CARTESIAN_POINT('Ctrl Pts',(-4.0850946608337,-0.114182886570259,53.3703485658236));
#8982=CARTESIAN_POINT('Ctrl Pts',(-4.08011509051747,-0.231867440180717,
53.3760821030108));
#8983=CARTESIAN_POINT('Ctrl Pts',(-4.07004418083968,-0.349235402004226,
53.381815640198));
#8984=CARTESIAN_POINT('Ctrl Pts',(-4.0596633716385,-0.470214981506232,53.3877256083631));
#8985=CARTESIAN_POINT('Ctrl Pts',(-4.04387275277963,-0.590857721096756,
53.3936355765281));
#8986=CARTESIAN_POINT('Ctrl Pts',(-4.0227131092999,-0.710636503612598,53.3995455446931));
#8987=CARTESIAN_POINT('Ctrl Pts',(-4.00221473529391,-0.826672025871896,
53.4052708178021));
#8988=CARTESIAN_POINT('Ctrl Pts',(-3.97667799340902,-0.941896338091274,
53.4109960909111));
#8989=CARTESIAN_POINT('Ctrl Pts',(-3.94619255154103,-1.05583585190221,53.4167213640201));
#8990=CARTESIAN_POINT('Ctrl Pts',(-3.91571465964673,-1.16974714764318,53.4224452192175));
#8991=CARTESIAN_POINT('Ctrl Pts',(-3.8802906122784,-1.28237387106175,53.4281690744149));
#8992=CARTESIAN_POINT('Ctrl Pts',(-3.84006075202239,-1.39325461448268,53.4338929296123));
#8993=CARTESIAN_POINT('Ctrl Pts',(-3.79983072022201,-1.50413583071077,53.4396168092168));
#8994=CARTESIAN_POINT('Ctrl Pts',(-3.75479497912581,-1.61327065677188,53.4453406888213));
#8995=CARTESIAN_POINT('Ctrl Pts',(-3.7051428357764,-1.72021555814811,53.4510645684258));
#8996=CARTESIAN_POINT('Ctrl Pts',(-3.65547797106196,-1.82718785985465,53.4567899145443));
#8997=CARTESIAN_POINT('Ctrl Pts',(-3.60119453146051,-1.93196874060564,53.4625152606628));
#8998=CARTESIAN_POINT('Ctrl Pts',(-3.54252842342547,-2.03413799168657,53.4682406067813));
#8999=CARTESIAN_POINT('Ctrl Pts',(-3.4838014026026,-2.13641332469661,53.473971897504));
#9000=CARTESIAN_POINT('Ctrl Pts',(-3.42068284295228,-2.23607125209266,53.4797031882267));
#9001=CARTESIAN_POINT('Ctrl Pts',(-3.35345271933515,-2.33271941287068,53.4854344789494));
#9002=CARTESIAN_POINT('Ctrl Pts',(-3.28618056105595,-2.42942800151284,53.4911693530787));
#9003=CARTESIAN_POINT('Ctrl Pts',(-3.2147919776946,-2.52312274512152,53.496904227208));
#9004=CARTESIAN_POINT('Ctrl Pts',(-3.13960694212807,-2.61344470937137,53.5026391013373));
#9005=CARTESIAN_POINT('Ctrl Pts',(-3.06431706707054,-2.70389262034303,53.5083819722878));
#9006=CARTESIAN_POINT('Ctrl Pts',(-2.98522046104977,-2.79095806015633,53.5141248432383));
#9007=CARTESIAN_POINT('Ctrl Pts',(-2.90267351731113,-2.87431930235676,53.5198677141888));
#9008=CARTESIAN_POINT('Ctrl Pts',(-2.8845282000555,-2.89264361720165,53.5211301015121));
#9009=CARTESIAN_POINT('Ctrl Pts',(-2.86621628596619,-2.91078910223333,53.5223924888354));
#9010=CARTESIAN_POINT('Ctrl Pts',(-2.84774176294681,-2.92875261016847,53.5236548761588));
#9011=CARTESIAN_POINT('Ctrl Pts',(-2.76248879875287,-3.01164743225319,53.5294803181018));
#9012=CARTESIAN_POINT('Ctrl Pts',(-2.67347771023089,-3.09094862859931,53.5353057600448));
#9013=CARTESIAN_POINT('Ctrl Pts',(-2.58104361116293,-3.16629734505068,53.5411312019878));
#9014=CARTESIAN_POINT('Ctrl Pts',(-2.49470736968296,-3.23667532292191,53.5465723407817));
#9015=CARTESIAN_POINT('Ctrl Pts',(-2.40538541417085,-3.3036051904254,53.5520134795756));
#9016=CARTESIAN_POINT('Ctrl Pts',(-2.31338095599001,-3.36682247118299,53.5574546183695));
#9017=CARTESIAN_POINT('',(-4.08499939840936,-0.00221697883968487,53.2603849714447));
#9018=CARTESIAN_POINT('Ctrl Pts',(-4.08499939840936,-0.00221697883967045,
53.2603849714447));
#9019=CARTESIAN_POINT('Ctrl Pts',(-4.08492707751238,-0.135475274033514,
53.2668482540158));
#9020=CARTESIAN_POINT('Ctrl Pts',(-4.07833004186189,-0.268506050828305,
53.2733115365868));
#9021=CARTESIAN_POINT('Ctrl Pts',(-4.06529953148975,-0.400705277316363,
53.2797748191579));
#9022=CARTESIAN_POINT('Ctrl Pts',(-4.05222537576177,-0.533347301677931,
53.2862597503259));
#9023=CARTESIAN_POINT('Ctrl Pts',(-4.03267468654002,-0.665151973365606,
53.2927446814939));
#9024=CARTESIAN_POINT('Ctrl Pts',(-4.00678976762601,-0.795525460338974,
53.299229612662));
#9025=CARTESIAN_POINT('Ctrl Pts',(-3.98078013150707,-0.926527105234957,
53.3057457891467));
#9026=CARTESIAN_POINT('Ctrl Pts',(-3.94837518576072,-1.05608352155153,53.3122619656315));
#9027=CARTESIAN_POINT('Ctrl Pts',(-3.90976823011133,-1.18361200856199,53.3187781421162));
#9028=CARTESIAN_POINT('Ctrl Pts',(-3.87516577533156,-1.29791262177236,53.3246184291411));
#9029=CARTESIAN_POINT('Ctrl Pts',(-3.83558190815159,-1.41058434768274,53.330458716166));
#9030=CARTESIAN_POINT('Ctrl Pts',(-3.79118783028315,-1.52122313797581,53.3362990031909));
#9031=CARTESIAN_POINT('Ctrl Pts',(-3.74690246501772,-1.6315909950394,53.3421249884703));
#9032=CARTESIAN_POINT('Ctrl Pts',(-3.69772314220471,-1.7401990447553,53.3479509737497));
#9033=CARTESIAN_POINT('Ctrl Pts',(-3.64381057578868,-1.84658319275643,53.353776959029));
#9034=CARTESIAN_POINT('Ctrl Pts',(-3.58996186347553,-1.95284133925584,53.3595960440051));
#9035=CARTESIAN_POINT('Ctrl Pts',(-3.53139123772933,-2.05688046120153,53.3654151289811));
#9036=CARTESIAN_POINT('Ctrl Pts',(-3.46830796704526,-2.15825504649714,53.3712342139571));
#9037=CARTESIAN_POINT('Ctrl Pts',(-3.40528456459923,-2.25953342375317,53.3770477764172));
#9038=CARTESIAN_POINT('Ctrl Pts',(-3.3377572495909,-2.35815194973833,53.3828613388773));
#9039=CARTESIAN_POINT('Ctrl Pts',(-3.26598154053163,-2.45368897313955,53.3886749013375));
#9040=CARTESIAN_POINT('Ctrl Pts',(-3.1942586231698,-2.54915572817701,53.3944841878687));
#9041=CARTESIAN_POINT('Ctrl Pts',(-3.11829377405021,-2.64154516592262,53.4002934743999));
#9042=CARTESIAN_POINT('Ctrl Pts',(-3.03838585205935,-2.73046450517225,53.4061027609311));
#9043=CARTESIAN_POINT('Ctrl Pts',(-2.9585130687976,-2.81934474300995,53.4119094928852));
#9044=CARTESIAN_POINT('Ctrl Pts',(-2.87470093510515,-2.90475761602359,53.4177162248393));
#9045=CARTESIAN_POINT('Ctrl Pts',(-2.78728827016216,-2.98634376772274,53.4235229567934));
#9046=CARTESIAN_POINT('Ctrl Pts',(-2.69987790237354,-3.06792777538491,53.42932953615));
#9047=CARTESIAN_POINT('Ctrl Pts',(-2.60886748387272,-3.14568497751308,53.4351361155066));
#9048=CARTESIAN_POINT('Ctrl Pts',(-2.51463206891315,-3.21929348739651,53.4409426948631));
#9049=CARTESIAN_POINT('Ctrl Pts',(-2.44906374430374,-3.27050975966657,53.4449828710568));
#9050=CARTESIAN_POINT('Ctrl Pts',(-2.38193487256495,-3.31971831691873,53.4490230472505));
#9051=CARTESIAN_POINT('Ctrl Pts',(-2.31338095599002,-3.36682247118299,53.4530632234442));
#9052=CARTESIAN_POINT('Ctrl Pts',(-2.31338095599002,-3.36682247118298,52.2032272635689));
#9053=CARTESIAN_POINT('Ctrl Pts',(-2.21500698803516,-3.43441631255116,52.209038374945));
#9054=CARTESIAN_POINT('Ctrl Pts',(-2.11358325818932,-3.49775331847722,52.2148494863211));
#9055=CARTESIAN_POINT('Ctrl Pts',(-2.0095158195868,-3.55655327119254,52.2206605976972));
#9056=CARTESIAN_POINT('Ctrl Pts',(-1.90550258339924,-3.61532259857991,52.2264686824179));
#9057=CARTESIAN_POINT('Ctrl Pts',(-1.79884873132084,-3.66955937251817,52.2322767671387));
#9058=CARTESIAN_POINT('Ctrl Pts',(-1.68998803059726,-3.71902748799172,52.2380848518594));
#9059=CARTESIAN_POINT('Ctrl Pts',(-1.58115537394738,-3.76848285977111,52.2438914403345));
#9060=CARTESIAN_POINT('Ctrl Pts',(-1.47011737018069,-3.8131718473842,52.2496980288095));
#9061=CARTESIAN_POINT('Ctrl Pts',(-1.35733050818773,-3.85290525338255,52.2555046172846));
#9062=CARTESIAN_POINT('Ctrl Pts',(-1.24454616975475,-3.89263777036216,52.2613110758396));
#9063=CARTESIAN_POINT('Ctrl Pts',(-1.13001343562466,-3.92741479094115,52.2671175343946));
#9064=CARTESIAN_POINT('Ctrl Pts',(-1.01420620174307,-3.95709625613857,52.2729239929496));
#9065=CARTESIAN_POINT('Ctrl Pts',(-0.898374316818721,-3.9867840394134,52.2787316874831));
#9066=CARTESIAN_POINT('Ctrl Pts',(-0.781267787618402,-4.01137400909616,
52.2845393820167));
#9067=CARTESIAN_POINT('Ctrl Pts',(-0.663372383682657,-4.03077685819585,
52.2903470765502));
#9068=CARTESIAN_POINT('Ctrl Pts',(-0.54535394965723,-4.05019995519482,52.2961608317202));
#9069=CARTESIAN_POINT('Ctrl Pts',(-0.426545399849018,-4.06442505521714,
52.3019745868902));
#9070=CARTESIAN_POINT('Ctrl Pts',(-0.307439577105467,-4.07341452671211,
52.3077883420602));
#9071=CARTESIAN_POINT('Ctrl Pts',(-0.188267544862691,-4.08240899534653,
52.313605329027));
#9072=CARTESIAN_POINT('Ctrl Pts',(-0.0687983178358109,-4.08616202451501,
52.3194223159937));
#9073=CARTESIAN_POINT('Ctrl Pts',(0.0504750103484449,-4.0846881488469,52.3252393029605));
#9074=CARTESIAN_POINT('Ctrl Pts',(0.169931934319669,-4.08321200446233,52.331065243935));
#9075=CARTESIAN_POINT('Ctrl Pts',(0.289191950067047,-4.07649290644593,52.3368911849095));
#9076=CARTESIAN_POINT('Ctrl Pts',(0.407766381997247,-4.06459734509002,52.3427171258841));
#9077=CARTESIAN_POINT('Ctrl Pts',(0.491331501897505,-4.05621396939254,52.3468229474186));
#9078=CARTESIAN_POINT('Ctrl Pts',(0.574556245414403,-4.04526069041347,52.3509287689531));
#9079=CARTESIAN_POINT('Ctrl Pts',(0.657273191228009,-4.0317759054904,52.3550345904877));
#9080=CARTESIAN_POINT('Ctrl Pts',(0.774658327852714,-4.01263939960301,52.3608612372171));
#9081=CARTESIAN_POINT('Ctrl Pts',(0.891393842455179,-3.98834168701438,52.3666878839465));
#9082=CARTESIAN_POINT('Ctrl Pts',(1.00699158944047,-3.95893836006525,52.3725145306759));
#9083=CARTESIAN_POINT('Ctrl Pts',(1.12244472614728,-3.92957181604148,52.3783338883963));
#9084=CARTESIAN_POINT('Ctrl Pts',(1.23676253446512,-3.89511246137051,52.3841532461168));
#9085=CARTESIAN_POINT('Ctrl Pts',(1.34946450787744,-3.85566732771113,52.3899726038373));
#9086=CARTESIAN_POINT('Ctrl Pts',(1.46205477330165,-3.81626129129547,52.3957861935245));
#9087=CARTESIAN_POINT('Ctrl Pts',(1.57303200732343,-3.77187944130429,52.4015997832116));
#9088=CARTESIAN_POINT('Ctrl Pts',(1.68192895912139,-3.7226791396075,52.4074133728987));
#9089=CARTESIAN_POINT('Ctrl Pts',(1.79421938401356,-3.67194564623474,52.4134081270708));
#9090=CARTESIAN_POINT('Ctrl Pts',(1.9042973225786,-3.61608858344617,52.4194028812429));
#9091=CARTESIAN_POINT('Ctrl Pts',(2.01167027494216,-3.55533510444713,52.4253976354149));
#9092=CARTESIAN_POINT('Ctrl Pts',(2.11568317291385,-3.49648280250842,52.4312047939249));
#9093=CARTESIAN_POINT('Ctrl Pts',(2.21715747509268,-3.43303618012524,52.437011952435));
#9094=CARTESIAN_POINT('Ctrl Pts',(2.31566929715199,-3.36524898131292,52.442819110945));
#9095=CARTESIAN_POINT('Ctrl Pts',(2.41416702468894,-3.29747148111512,52.4486254385991));
#9096=CARTESIAN_POINT('Ctrl Pts',(2.50970277920253,-3.22535487070371,52.4544317662533));
#9097=CARTESIAN_POINT('Ctrl Pts',(2.60188164598711,-3.14919623083024,52.4602380939075));
#9098=CARTESIAN_POINT('Ctrl Pts',(2.69406900893618,-3.07303057138326,52.4660449567332));
#9099=CARTESIAN_POINT('Ctrl Pts',(2.78289855458322,-2.99282240150259,52.471851819559));
#9100=CARTESIAN_POINT('Ctrl Pts',(2.86800894597763,-2.90890867608322,52.4776586823848));
#9101=CARTESIAN_POINT('Ctrl Pts',(2.95314720364018,-2.82496747620001,52.4834674464543));
#9102=CARTESIAN_POINT('Ctrl Pts',(3.03456359502749,-2.73731859401619,52.4892762105238));
#9103=CARTESIAN_POINT('Ctrl Pts',(3.11193454611108,-2.64633489579842,52.4950849745933));
#9104=CARTESIAN_POINT('Ctrl Pts',(3.18939052502715,-2.55525120983922,52.5009001222811));
#9105=CARTESIAN_POINT('Ctrl Pts',(3.26279192542986,-2.46082570358057,52.5067152699689));
#9106=CARTESIAN_POINT('Ctrl Pts',(3.33185620162636,-2.3634634018076,52.5125304176567));
#9107=CARTESIAN_POINT('Ctrl Pts',(3.40096596666728,-2.26603697283543,52.5183493954628));
#9108=CARTESIAN_POINT('Ctrl Pts',(3.46573269772204,-2.16567023788159,52.5241683732689));
#9109=CARTESIAN_POINT('Ctrl Pts',(3.52591869455345,-2.06279479333221,52.529987351075));
#9110=CARTESIAN_POINT('Ctrl Pts',(3.58618938569597,-1.95977458147208,52.5358145174024));
#9111=CARTESIAN_POINT('Ctrl Pts',(3.6418662878908,-1.85423897356204,52.5416416837298));
#9112=CARTESIAN_POINT('Ctrl Pts',(3.69275883995195,-1.74664167760784,52.5474688500572));
#9113=CARTESIAN_POINT('Ctrl Pts',(3.70387570519099,-1.72313834380428,52.5487417243809));
#9114=CARTESIAN_POINT('Ctrl Pts',(3.71476447124475,-1.69953670046962,52.5500145987046));
#9115=CARTESIAN_POINT('Ctrl Pts',(3.72542346702583,-1.67584157703921,52.5512874730283));
#9116=CARTESIAN_POINT('Ctrl Pts',(3.77421541008635,-1.56737628284319,52.5571141018029));
#9117=CARTESIAN_POINT('Ctrl Pts',(3.81834414749158,-1.45660573581094,52.5629407305775));
#9118=CARTESIAN_POINT('Ctrl Pts',(3.85758676850764,-1.34396775386718,52.568767359352));
#9119=CARTESIAN_POINT('Ctrl Pts',(3.89678029524987,-1.231470687076,52.5745866987534));
#9120=CARTESIAN_POINT('Ctrl Pts',(3.93109973111366,-1.11711121406019,52.5804060381548));
#9121=CARTESIAN_POINT('Ctrl Pts',(3.96036928397369,-1.00134915716634,52.5862253775562));
#9122=CARTESIAN_POINT('Ctrl Pts',(3.98960982362738,-0.885701848470356,52.5920389485848));
#9123=CARTESIAN_POINT('Ctrl Pts',(4.01381033934235,-0.768655114975705,52.5978525196133));
#9124=CARTESIAN_POINT('Ctrl Pts',(4.03284433088837,-0.650685486868673,52.6036660906418));
#9125=CARTESIAN_POINT('Ctrl Pts',(4.05247154974745,-0.529039130980441,52.6096608516805));
#9126=CARTESIAN_POINT('Ctrl Pts',(4.06660477596062,-0.406411827768004,52.6156556127191));
#9127=CARTESIAN_POINT('Ctrl Pts',(4.075161791792,-0.283339673746216,52.6216503737577));
#9128=CARTESIAN_POINT('Ctrl Pts',(4.08345099316412,-0.164119388533449,52.6274575128826));
#9129=CARTESIAN_POINT('Ctrl Pts',(4.08650779254272,-0.0444821194083759,
52.6332646520076));
#9130=CARTESIAN_POINT('Ctrl Pts',(4.08431000327408,0.0750786065086086,52.6390717911325));
#9131=CARTESIAN_POINT('Ctrl Pts',(4.08211252854322,0.194622221428443,52.6448780991656));
#9132=CARTESIAN_POINT('Ctrl Pts',(4.07466196826704,0.314088907287876,52.6506844071987));
#9133=CARTESIAN_POINT('Ctrl Pts',(4.06198826299498,0.432985393854173,52.6564907152318));
#9134=CARTESIAN_POINT('Ctrl Pts',(4.04931339004772,0.55189283479214,52.6622975582215));
#9135=CARTESIAN_POINT('Ctrl Pts',(4.03141445853581,0.670229566454351,52.6681044012111));
#9136=CARTESIAN_POINT('Ctrl Pts',(4.00837319014032,0.787508329203119,52.6739112442008));
#9137=CARTESIAN_POINT('Ctrl Pts',(3.98532437847418,0.904825486776082,52.6797199882398));
#9138=CARTESIAN_POINT('Ctrl Pts',(3.95712996032764,1.02108358664462,52.6855287322788));
#9139=CARTESIAN_POINT('Ctrl Pts',(3.92392244191665,1.13580705660022,52.6913374763179));
#9140=CARTESIAN_POINT('Ctrl Pts',(3.89067843061372,1.25065660014977,52.6971526037869));
#9141=CARTESIAN_POINT('Ctrl Pts',(3.8524104362825,1.36396775564721,52.7029677312558));
#9142=CARTESIAN_POINT('Ctrl Pts',(3.80930042078689,1.47528143219958,52.7087828587248));
#9143=CARTESIAN_POINT('Ctrl Pts',(3.76616201198175,1.58666842265907,52.7146018161789));
#9144=CARTESIAN_POINT('Ctrl Pts',(3.7181753941769,1.69605494150659,52.7204207736329));
#9145=CARTESIAN_POINT('Ctrl Pts',(3.66556943056963,1.80300464493951,52.7262397310869));
#9146=CARTESIAN_POINT('Ctrl Pts',(3.61288943947137,1.91010484876563,52.7320668770198));
#9147=CARTESIAN_POINT('Ctrl Pts',(3.55557732414915,2.01476103695856,52.7378940229527));
#9148=CARTESIAN_POINT('Ctrl Pts',(3.49390639434769,2.11656398616633,52.7437211688856));
#9149=CARTESIAN_POINT('Ctrl Pts',(3.48043308645596,2.13880497529003,52.7449942311134));
#9150=CARTESIAN_POINT('Ctrl Pts',(3.46675189086912,2.16090990094908,52.7462672933412));
#9151=CARTESIAN_POINT('Ctrl Pts',(3.45286591532056,2.18287470341692,52.747540355569));
#9152=CARTESIAN_POINT('Ctrl Pts',(3.38931155483806,2.28340483679403,52.7533670009825));
#9153=CARTESIAN_POINT('Ctrl Pts',(3.32126201023034,2.38131708177875,52.7591936463961));
#9154=CARTESIAN_POINT('Ctrl Pts',(3.24895949813556,2.4761839954807,52.7650202918096));
#9155=CARTESIAN_POINT('Ctrl Pts',(3.17674743658946,2.57093223053445,52.7708396480812));
#9156=CARTESIAN_POINT('Ctrl Pts',(3.10029323527421,2.66264239043829,52.7766590043528));
#9157=CARTESIAN_POINT('Ctrl Pts',(3.01988345646099,2.75091419520734,52.7824783606244));
#9158=CARTESIAN_POINT('Ctrl Pts',(2.93955338007064,2.83909850468893,52.7882919487319));
#9159=CARTESIAN_POINT('Ctrl Pts',(2.85527579944563,2.92385093948815,52.7941055368394));
#9160=CARTESIAN_POINT('Ctrl Pts',(2.76737840353038,3.00480311695686,52.799919124947));
#9161=CARTESIAN_POINT('Ctrl Pts',(2.67674189491262,3.08827797596,52.8059138796621));
#9162=CARTESIAN_POINT('Ctrl Pts',(2.5822565373443,3.16771149489399,52.8119086343772));
#9163=CARTESIAN_POINT('Ctrl Pts',(2.48432412614819,3.24273937223423,52.8179033890923));
#9164=CARTESIAN_POINT('Ctrl Pts',(2.389456383202,3.31541934911195,52.8237105457057));
#9165=CARTESIAN_POINT('Ctrl Pts',(2.29135445900398,3.38396504402743,52.829517702319));
#9166=CARTESIAN_POINT('Ctrl Pts',(2.19041776181656,3.44808570495551,52.8353248589324));
#9167=CARTESIAN_POINT('Ctrl Pts',(2.08949550808893,3.51219719058646,52.8411311845751));
#9168=CARTESIAN_POINT('Ctrl Pts',(1.98573963224814,3.57188468292064,52.8469375102178));
#9169=CARTESIAN_POINT('Ctrl Pts',(1.87957808327149,3.62690105033008,52.8527438358605));
#9170=CARTESIAN_POINT('Ctrl Pts',(1.77340675140529,3.68192248755107,52.8585506965617));
#9171=CARTESIAN_POINT('Ctrl Pts',(1.66482966773145,3.73227175636399,52.8643575572629));
#9172=CARTESIAN_POINT('Ctrl Pts',(1.55429833197111,3.77774823078932,52.8701644179642));
#9173=CARTESIAN_POINT('Ctrl Pts',(1.44373080889862,3.8232395939461,52.8759731797976));
#9174=CARTESIAN_POINT('Ctrl Pts',(1.33120813820938,3.86385483482828,52.881781941631));
#9175=CARTESIAN_POINT('Ctrl Pts',(1.21720008567028,3.8994421333627,52.8875907034644));
#9176=CARTESIAN_POINT('Ctrl Pts',(1.10306674545585,3.93506854009874,52.8934058487616));
#9177=CARTESIAN_POINT('Ctrl Pts',(0.987445154693642,3.96565585411625,52.8992209940587));
#9178=CARTESIAN_POINT('Ctrl Pts',(0.870818613648606,3.99110259729352,52.9050361393558));
#9179=CARTESIAN_POINT('Ctrl Pts',(0.754115258948155,4.01656610044108,52.910855114678));
#9180=CARTESIAN_POINT('Ctrl Pts',(0.636406036678969,4.03688222061418,52.9166740900001));
#9181=CARTESIAN_POINT('Ctrl Pts',(0.518181146399915,4.05200114752151,52.9224930653222));
#9182=CARTESIAN_POINT('Ctrl Pts',(0.399789891239966,4.06714134963129,52.9283202290481));
#9183=CARTESIAN_POINT('Ctrl Pts',(0.280881924693484,4.07706972837865,52.934147392774));
#9184=CARTESIAN_POINT('Ctrl Pts',(0.161949343723945,4.08178850628831,52.9399745564999));
#9185=CARTESIAN_POINT('Ctrl Pts',(0.135969542851364,4.08281928279594,52.9412474503698));
#9186=CARTESIAN_POINT('Ctrl Pts',(0.109988553447076,4.08360167160106,52.9425203442398));
#9187=CARTESIAN_POINT('Ctrl Pts',(0.0840114739612687,4.08413602518854,52.9437932381097));
#9188=CARTESIAN_POINT('Ctrl Pts',(-0.034897975426568,4.08658201573572,52.9496198788329));
#9189=CARTESIAN_POINT('Ctrl Pts',(-0.15410357739852,4.08383452756355,52.9554465195561));
#9190=CARTESIAN_POINT('Ctrl Pts',(-0.273115193520258,4.07585979776886,52.9612731602793));
#9191=CARTESIAN_POINT('Ctrl Pts',(-0.391977925072666,4.06789504443067,52.9670925118242));
#9192=CARTESIAN_POINT('Ctrl Pts',(-0.510646750076163,4.05471608350436,52.972911863369));
#9193=CARTESIAN_POINT('Ctrl Pts',(-0.628629723682521,4.0363411241498,52.9787312149139));
#9194=CARTESIAN_POINT('Ctrl Pts',(-0.746495751490381,4.01798437822238,52.9845447982645));
#9195=CARTESIAN_POINT('Ctrl Pts',(-0.863676879673685,3.99444194254858,52.9903583816151));
#9196=CARTESIAN_POINT('Ctrl Pts',(-0.979685081592328,3.96578392514083,52.9961719649657));
#9197=CARTESIAN_POINT('Ctrl Pts',(-1.09930853567253,3.93623281605797,53.0021667214525));
#9198=CARTESIAN_POINT('Ctrl Pts',(-1.21768431984795,3.90124209033029,53.0081614779394));
#9199=CARTESIAN_POINT('Ctrl Pts',(-1.3342869301514,3.86094591881668,53.0141562344262));
#9200=CARTESIAN_POINT('Ctrl Pts',(-1.44724048568803,3.82191080772327,53.0199633862387));
#9201=CARTESIAN_POINT('Ctrl Pts',(-1.55852978083371,3.77789750739931,53.0257705380513));
#9202=CARTESIAN_POINT('Ctrl Pts',(-1.66769197672091,3.72907876972058,53.0315776898638));
#9203=CARTESIAN_POINT('Ctrl Pts',(-1.77683855196805,3.68026701779293,53.0373840106979));
#9204=CARTESIAN_POINT('Ctrl Pts',(-1.88385826112438,3.62665136253305,53.0431903315319));
#9205=CARTESIAN_POINT('Ctrl Pts',(-1.98830890445525,3.56845242373553,53.048996652366));
#9206=CARTESIAN_POINT('Ctrl Pts',(-2.09276917297909,3.51024812186892,53.0548035082563));
#9207=CARTESIAN_POINT('Ctrl Pts',(-2.19465954872222,3.44745989522938,53.0606103641465));
#9208=CARTESIAN_POINT('Ctrl Pts',(-2.29356363027887,3.380353661063,53.0664172200368));
#9209=CARTESIAN_POINT('Ctrl Pts',(-2.39250009253079,3.3132254566555,53.0722259770622));
#9210=CARTESIAN_POINT('Ctrl Pts',(-2.48844797885417,3.24177666199389,53.0780347340876));
#9211=CARTESIAN_POINT('Ctrl Pts',(-2.58102152001363,3.16631535277625,53.0838434911131));
#9212=CARTESIAN_POINT('Ctrl Pts',(-2.67369679420993,3.09077111588775,53.0896586316309));
#9213=CARTESIAN_POINT('Ctrl Pts',(-2.76299000531434,3.01120582074493,53.0954737721487));
#9214=CARTESIAN_POINT('Ctrl Pts',(-2.84854990754255,2.92796660230941,53.1012889126665));
#9215=CARTESIAN_POINT('Ctrl Pts',(-2.93416616224167,2.8446725598791,53.1071078832206));
#9216=CARTESIAN_POINT('Ctrl Pts',(-3.01604393215193,2.75770007124546,53.1129268537748));
#9217=CARTESIAN_POINT('Ctrl Pts',(-3.09387126105113,2.667430527688,53.118745824329));
#9218=CARTESIAN_POINT('Ctrl Pts',(-3.17180810857496,2.57703395682027,53.1245729833391));
#9219=CARTESIAN_POINT('Ctrl Pts',(-3.24568288782318,2.4833313902525,53.1304001423491));
#9220=CARTESIAN_POINT('Ctrl Pts',(-3.31522599577638,2.38673450491012,53.1362273013592));
#9221=CARTESIAN_POINT('Ctrl Pts',(-3.33041765044895,2.36563296706175,53.1375002411229));
#9222=CARTESIAN_POINT('Ctrl Pts',(-3.34540276909452,2.34439340882316,53.1387731808866));
#9223=CARTESIAN_POINT('Ctrl Pts',(-3.36017883296746,2.32302027767246,53.1400461206503));
#9224=CARTESIAN_POINT('Ctrl Pts',(-3.42855138775025,2.22412143742332,53.1459363323112));
#9225=CARTESIAN_POINT('Ctrl Pts',(-3.49265941604598,2.12204927775056,53.1518265439721));
#9226=CARTESIAN_POINT('Ctrl Pts',(-3.55219939808078,2.01720213074311,53.1577167556331));
#9227=CARTESIAN_POINT('Ctrl Pts',(-3.61166123393254,1.91249259553971,53.1635992363955));
#9228=CARTESIAN_POINT('Ctrl Pts',(-3.66656675741592,1.80501565989358,53.1694817171579));
#9229=CARTESIAN_POINT('Ctrl Pts',(-3.71665474298537,1.69519984705178,53.1753641979204));
#9230=CARTESIAN_POINT('Ctrl Pts',(-3.7666878415431,1.58550437168689,53.1812402325903));
#9231=CARTESIAN_POINT('Ctrl Pts',(-3.81191374341681,1.47347547702521,53.1871162672601));
#9232=CARTESIAN_POINT('Ctrl Pts',(-3.85211657335827,1.3595671757065,53.19299230193));
#9233=CARTESIAN_POINT('Ctrl Pts',(-3.89227897573479,1.24577341943986,53.198862427718));
#9234=CARTESIAN_POINT('Ctrl Pts',(-3.9274282343796,1.13010439218986,53.204732553506));
#9235=CARTESIAN_POINT('Ctrl Pts',(-3.95739640388031,1.01303440344108,53.210602679294));
#9236=CARTESIAN_POINT('Ctrl Pts',(-3.98734661432799,0.896034571334156,53.2164692872863));
#9237=CARTESIAN_POINT('Ctrl Pts',(-4.01212181647168,0.777635831074868,53.2223358952785));
#9238=CARTESIAN_POINT('Ctrl Pts',(-4.03160383849986,0.658327797828088,53.2282025032707));
#9239=CARTESIAN_POINT('Ctrl Pts',(-4.05108012858619,0.539054867031542,53.2340673852072));
#9240=CARTESIAN_POINT('Ctrl Pts',(-4.06526627018128,0.418873565411573,53.2399322671437));
#9241=CARTESIAN_POINT('Ctrl Pts',(-4.074095230338,0.298283513016052,53.2457971490802));
#9242=CARTESIAN_POINT('Ctrl Pts',(-4.08141537212827,0.19830160502653,53.2506597565216));
#9243=CARTESIAN_POINT('Ctrl Pts',(-4.0850538085329,0.0980390096750171,53.2555223639631));
#9244=CARTESIAN_POINT('Ctrl Pts',(-4.08499939840981,-0.0022169780104106,
53.2603849714045));
#9245=CARTESIAN_POINT('Origin',(0.,0.,46.4896150285955));
#9246=CARTESIAN_POINT('',(-2.31338095599002,-3.36682247118298,50.953013989131));
#9247=CARTESIAN_POINT('',(-2.31338095599002,-3.36682247118299,51.0573853382455));
#9248=CARTESIAN_POINT('',(-2.31338095599002,-3.36682247118298,46.4896150285955));
#9249=CARTESIAN_POINT('',(-4.08744329586254,-0.00250500349578786,50.7603840336099));
#9250=CARTESIAN_POINT('Ctrl Pts',(-4.08499922105558,-0.00252269208140621,
50.7603849714045));
#9251=CARTESIAN_POINT('Ctrl Pts',(-4.08489554760012,-0.17040128016159,50.7685938243239));
#9252=CARTESIAN_POINT('Ctrl Pts',(-4.07444292066524,-0.337949364085238,
50.7768026772432));
#9253=CARTESIAN_POINT('Ctrl Pts',(-4.05376347893569,-0.504208941657341,
50.7850115301626));
#9254=CARTESIAN_POINT('Ctrl Pts',(-4.0390990543464,-0.622108692987181,50.7908326788268));
#9255=CARTESIAN_POINT('Ctrl Pts',(-4.0192630313701,-0.739559716220486,50.796653827491));
#9256=CARTESIAN_POINT('Ctrl Pts',(-3.99429146142702,-0.856072848051627,
50.8024749761552));
#9257=CARTESIAN_POINT('Ctrl Pts',(-3.96935207559578,-0.972435814247411,
50.8082886223475));
#9258=CARTESIAN_POINT('Ctrl Pts',(-3.93929039337994,-1.08786289707374,50.8141022685399));
#9259=CARTESIAN_POINT('Ctrl Pts',(-3.90419418194402,-1.2018705378178,50.8199159147323));
#9260=CARTESIAN_POINT('Ctrl Pts',(-3.86913946520073,-1.31574338589288,50.8257226873776));
#9261=CARTESIAN_POINT('Ctrl Pts',(-3.82906218921653,-1.42819974450792,50.8315294600229));
#9262=CARTESIAN_POINT('Ctrl Pts',(-3.78410087487403,-1.53876754864975,50.8373362326682));
#9263=CARTESIAN_POINT('Ctrl Pts',(-3.73916942985995,-1.64926189884342,50.8431391476772));
#9264=CARTESIAN_POINT('Ctrl Pts',(-3.68936055212682,-1.75786981223455,50.8489420626861));
#9265=CARTESIAN_POINT('Ctrl Pts',(-3.63486208925382,-1.8641358834874,50.8547449776951));
#9266=CARTESIAN_POINT('Ctrl Pts',(-3.58038693189061,-1.97035651153262,50.8605454111682));
#9267=CARTESIAN_POINT('Ctrl Pts',(-3.52122636487616,-2.07423692646578,50.8663458446412));
#9268=CARTESIAN_POINT('Ctrl Pts',(-3.45761544334531,-2.17534375351115,50.8721462781143));
#9269=CARTESIAN_POINT('Ctrl Pts',(-3.39401666823448,-2.27643127434372,50.8779456040024));
#9270=CARTESIAN_POINT('Ctrl Pts',(-3.3259694479581,-2.37474591591575,50.8837449298905));
#9271=CARTESIAN_POINT('Ctrl Pts',(-3.2537533285065,-2.4698814297923,50.8895442557786));
#9272=CARTESIAN_POINT('Ctrl Pts',(-3.18150701820337,-2.56505671625976,50.8953460061474));
#9273=CARTESIAN_POINT('Ctrl Pts',(-3.10508857127888,-2.65704989170036,50.9011477565161));
#9274=CARTESIAN_POINT('Ctrl Pts',(-3.02481911174047,-2.74548617575278,50.9069495068849));
#9275=CARTESIAN_POINT('Ctrl Pts',(-2.94453257356551,-2.83394127606684,50.9127524916707));
#9276=CARTESIAN_POINT('Ctrl Pts',(-2.86039367350361,-2.91883768214517,50.9185554764565));
#9277=CARTESIAN_POINT('Ctrl Pts',(-2.77276092894155,-2.9998369673926,50.9243584612423));
#9278=CARTESIAN_POINT('Ctrl Pts',(-2.6850428209863,-3.080915154355,50.9301670987379));
#9279=CARTESIAN_POINT('Ctrl Pts',(-2.59382437887124,-3.15808836898283,50.9359757362334));
#9280=CARTESIAN_POINT('Ctrl Pts',(-2.49949784853709,-3.23105795447226,50.941784373729));
#9281=CARTESIAN_POINT('Ctrl Pts',(-2.43871189780588,-3.27808105192665,50.945527578863));
#9282=CARTESIAN_POINT('Ctrl Pts',(-2.37663587796835,-3.32335931471133,50.949270783997));
#9283=CARTESIAN_POINT('Ctrl Pts',(-2.31338095599002,-3.36682247118298,50.953013989131));
#9284=CARTESIAN_POINT('',(3.17505078219416,-2.57026798806822,50.));
#9285=CARTESIAN_POINT('Ctrl Pts',(3.17505078219411,-2.57026798806828,50.));
#9286=CARTESIAN_POINT('Ctrl Pts',(4.02021879563803,-1.52623235652025,50.0654176275135));
#9287=CARTESIAN_POINT('Ctrl Pts',(4.58685143039127,1.44312147364938,50.1962528825406));
#9288=CARTESIAN_POINT('Ctrl Pts',(1.3219330033413,4.62797967283566,50.3925057650812));
#9289=CARTESIAN_POINT('Ctrl Pts',(-2.94254776511638,3.69335577407833,50.5805492729265));
#9290=CARTESIAN_POINT('Ctrl Pts',(-4.08029497582926,1.16864264796801,50.7031751532581));
#9291=CARTESIAN_POINT('Ctrl Pts',(-4.08907877044555,-0.00249316702003614,
50.7603834060762));
#9292=CARTESIAN_POINT('',(1.46246200503919,-3.81424040718683,50.0000002080809));
#9293=CARTESIAN_POINT('Origin',(0.,0.,50.));
#9294=CARTESIAN_POINT('',(-4.08499988058316,0.000987742680470998,50.8646150285511));
#9295=CARTESIAN_POINT('Ctrl Pts',(1.46246200503919,-3.81424040718683,50.0000002080809));
#9296=CARTESIAN_POINT('Ctrl Pts',(1.57281875983439,-3.77192724816746,50.005789033466));
#9297=CARTESIAN_POINT('Ctrl Pts',(1.68152243212576,-3.72474980731752,50.0115778588512));
#9298=CARTESIAN_POINT('Ctrl Pts',(1.78811065278834,-3.67285791903048,50.0173666842363));
#9299=CARTESIAN_POINT('Ctrl Pts',(1.89456686500696,-3.62103029832745,50.0231483402192));
#9300=CARTESIAN_POINT('Ctrl Pts',(1.9989124667768,-3.56450002029049,50.028929996202));
#9301=CARTESIAN_POINT('Ctrl Pts',(2.1007027958165,-3.50346582167555,50.0347116521849));
#9302=CARTESIAN_POINT('Ctrl Pts',(2.20239442697394,-3.44249080300635,50.0404877021617));
#9303=CARTESIAN_POINT('Ctrl Pts',(2.30153536049967,-3.37702076131729,50.0462637521385));
#9304=CARTESIAN_POINT('Ctrl Pts',(2.39770399593268,-3.30730109725263,50.0520398021153));
#9305=CARTESIAN_POINT('Ctrl Pts',(2.49380794685844,-3.2376283277092,50.0578119670318));
#9306=CARTESIAN_POINT('Ctrl Pts',(2.58694324233037,-3.16371186332526,50.0635841319483));
#9307=CARTESIAN_POINT('Ctrl Pts',(2.67671637718872,-3.08584096091968,50.0693562968649));
#9308=CARTESIAN_POINT('Ctrl Pts',(2.7664581058625,-3.00799730082816,50.0751264424503));
#9309=CARTESIAN_POINT('Ctrl Pts',(2.85283969999958,-2.92620222359289,50.0808965880358));
#9310=CARTESIAN_POINT('Ctrl Pts',(2.93550041055213,-2.84078551454492,50.0866667336213));
#9311=CARTESIAN_POINT('Ctrl Pts',(3.01815231908193,-2.75537790098878,50.09243626478));
#9312=CARTESIAN_POINT('Ctrl Pts',(3.09708384437165,-2.66634971987523,50.0982057959388));
#9313=CARTESIAN_POINT('Ctrl Pts',(3.17197133573925,-2.57406737387516,50.1039753270975));
#9314=CARTESIAN_POINT('Ctrl Pts',(3.24686907737394,-2.48177239667758,50.109745647964));
#9315=CARTESIAN_POINT('Ctrl Pts',(3.31772142436844,-2.38622269065863,50.1155159688305));
#9316=CARTESIAN_POINT('Ctrl Pts',(3.38424568780932,-2.287816890519,50.121286289697));
#9317=CARTESIAN_POINT('Ctrl Pts',(3.45083484815304,-2.1893150918471,50.127062239727));
#9318=CARTESIAN_POINT('Ctrl Pts',(3.51308726037022,-2.08795197779127,50.132838189757));
#9319=CARTESIAN_POINT('Ctrl Pts',(3.57076411768132,-1.98415438307596,50.138614139787));
#9320=CARTESIAN_POINT('Ctrl Pts',(3.62847000267175,-1.88030454898018,50.1443929967441));
#9321=CARTESIAN_POINT('Ctrl Pts',(3.68159556108044,-1.77401816375787,50.1501718537013));
#9322=CARTESIAN_POINT('Ctrl Pts',(3.72994921676155,-1.66574423018059,50.1559507106585));
#9323=CARTESIAN_POINT('Ctrl Pts',(3.77837747178567,-1.55730325309447,50.1617384831552));
#9324=CARTESIAN_POINT('Ctrl Pts',(3.82201896532527,-1.44686898697977,50.167526255652));
#9325=CARTESIAN_POINT('Ctrl Pts',(3.86073114014527,-1.33490826033575,50.1733140281488));
#9326=CARTESIAN_POINT('Ctrl Pts',(3.89203796568312,-1.24436478267184,50.1779946430885));
#9327=CARTESIAN_POINT('Ctrl Pts',(3.92012191362614,-1.1528233751915,50.1826752580281));
#9328=CARTESIAN_POINT('Ctrl Pts',(3.94493205986919,-1.06053573396478,50.1873558729678));
#9329=CARTESIAN_POINT('Ctrl Pts',(3.97586421810565,-0.945475714014513,50.1931914500958));
#9330=CARTESIAN_POINT('Ctrl Pts',(4.00180582916819,-0.828884727081285,50.1990270272237));
#9331=CARTESIAN_POINT('Ctrl Pts',(4.0226077902163,-0.711232427615012,50.2048626043517));
#9332=CARTESIAN_POINT('Ctrl Pts',(4.04338434750931,-0.593723807400644,50.2106910549606));
#9333=CARTESIAN_POINT('Ctrl Pts',(4.05903367022548,-0.475156849716197,50.2165195055695));
#9334=CARTESIAN_POINT('Ctrl Pts',(4.06945674036903,-0.356015221957,50.2223479561784));
#9335=CARTESIAN_POINT('Ctrl Pts',(4.07986976374012,-0.236988434528732,50.2281707887577));
#9336=CARTESIAN_POINT('Ctrl Pts',(4.08506652215019,-0.117388481742685,50.2339936213369));
#9337=CARTESIAN_POINT('Ctrl Pts',(4.08499935671531,0.00229251727920632,
50.2398164539162));
#9338=CARTESIAN_POINT('Ctrl Pts',(4.08493024750646,0.125437095626447,50.2458077998159));
#9339=CARTESIAN_POINT('Ctrl Pts',(4.07928781543186,0.248667050864927,50.2517991457155));
#9340=CARTESIAN_POINT('Ctrl Pts',(4.06807764895099,0.371442111378571,50.2577904916152));
#9341=CARTESIAN_POINT('Ctrl Pts',(4.05719422942123,0.490638600890343,50.2636072054959));
#9342=CARTESIAN_POINT('Ctrl Pts',(4.04106319214363,0.609405915005833,50.2694239193766));
#9343=CARTESIAN_POINT('Ctrl Pts',(4.0197424561347,0.727252078957643,50.2752406332573));
#9344=CARTESIAN_POINT('Ctrl Pts',(3.99842440272144,0.845083415390828,50.2810566152734));
#9345=CARTESIAN_POINT('Ctrl Pts',(3.97191802161883,0.961993432446621,50.2868725972895));
#9346=CARTESIAN_POINT('Ctrl Pts',(3.94033263351198,1.07749883400428,50.2926885793056));
#9347=CARTESIAN_POINT('Ctrl Pts',(3.90874385921344,1.19301661861163,50.2985051848388));
#9348=CARTESIAN_POINT('Ctrl Pts',(3.87207510227841,1.30712909633735,50.304321790372));
#9349=CARTESIAN_POINT('Ctrl Pts',(3.83048581820237,1.41936725217631,50.3101383959053));
#9350=CARTESIAN_POINT('Ctrl Pts',(3.78670914526065,1.5375085750892,50.3162609258722));
#9351=CARTESIAN_POINT('Ctrl Pts',(3.73748046088016,1.65357258449981,50.3223834558391));
#9352=CARTESIAN_POINT('Ctrl Pts',(3.68304315640458,1.76703653274666,50.328505985806));
#9353=CARTESIAN_POINT('Ctrl Pts',(3.63124944958615,1.87499041706503,50.3343311919794));
#9354=CARTESIAN_POINT('Ctrl Pts',(3.57474134718814,1.98059048751101,50.3401563981528));
#9355=CARTESIAN_POINT('Ctrl Pts',(3.51377502506969,2.08341308270743,50.3459816043262));
#9356=CARTESIAN_POINT('Ctrl Pts',(3.45276743203757,2.18630528325814,50.3518107538502));
#9357=CARTESIAN_POINT('Ctrl Pts',(3.38729583027118,2.2864159246399,50.3576399033742));
#9358=CARTESIAN_POINT('Ctrl Pts',(3.31765886986535,2.38335155258383,50.3634690528981));
#9359=CARTESIAN_POINT('Ctrl Pts',(3.24792504971802,2.48042201064974,50.3693063103279));
#9360=CARTESIAN_POINT('Ctrl Pts',(3.17401455895687,2.57430832408995,50.3751435677577));
#9361=CARTESIAN_POINT('Ctrl Pts',(3.09626535598136,2.6646511676671,50.3809808251875));
#9362=CARTESIAN_POINT('Ctrl Pts',(3.08459780545874,2.67820860171726,50.3818568019611));
#9363=CARTESIAN_POINT('Ctrl Pts',(3.07284387231894,2.69168630714175,50.3827327787348));
#9364=CARTESIAN_POINT('Ctrl Pts',(3.06100476611686,2.70508314508258,50.3836087555084));
#9365=CARTESIAN_POINT('Ctrl Pts',(2.98233802783124,2.79410046836335,50.3894293161504));
#9366=CARTESIAN_POINT('Ctrl Pts',(2.89965717996909,2.87982798958123,50.3952498767924));
#9367=CARTESIAN_POINT('Ctrl Pts',(2.81326808570803,2.96188245511814,50.4010704374344));
#9368=CARTESIAN_POINT('Ctrl Pts',(2.72698833177785,3.04383306654605,50.4068836311508));
#9369=CARTESIAN_POINT('Ctrl Pts',(2.63700996013592,3.12211958956528,50.4126968248672));
#9370=CARTESIAN_POINT('Ctrl Pts',(2.54367836128961,3.19639255948124,50.4185100185837));
#9371=CARTESIAN_POINT('Ctrl Pts',(2.45044049148093,3.27059094014683,50.4243173743518));
#9372=CARTESIAN_POINT('Ctrl Pts',(2.3538564115977,3.34078353291223,50.4301247301199));
#9373=CARTESIAN_POINT('Ctrl Pts',(2.25430710778994,3.40665884170513,50.4359320858879));
#9374=CARTESIAN_POINT('Ctrl Pts',(2.15150582662759,3.47468609937388,50.4419291505613));
#9375=CARTESIAN_POINT('Ctrl Pts',(2.04554259183216,3.53810886625143,50.4479262152347));
#9376=CARTESIAN_POINT('Ctrl Pts',(1.93687288945575,3.59663014641363,50.4539232799081));
#9377=CARTESIAN_POINT('Ctrl Pts',(1.83175977362679,3.65323611813923,50.4597240701915));
#9378=CARTESIAN_POINT('Ctrl Pts',(1.72411496627118,3.70525621613186,50.4655248604749));
#9379=CARTESIAN_POINT('Ctrl Pts',(1.61437806486332,3.75246698369062,50.4713256507583));
#9380=CARTESIAN_POINT('Ctrl Pts',(1.50465761465709,3.79967067364971,50.4771255714166));
#9381=CARTESIAN_POINT('Ctrl Pts',(1.39284606955893,3.84206630548709,50.4829254920749));
#9382=CARTESIAN_POINT('Ctrl Pts',(1.2794043061154,3.87947800889416,50.4887254127331));
#9383=CARTESIAN_POINT('Ctrl Pts',(1.16595269870593,3.91689295872056,50.4945258366824));
#9384=CARTESIAN_POINT('Ctrl Pts',(1.05087097998002,3.9493229922709,50.5003262606317));
#9385=CARTESIAN_POINT('Ctrl Pts',(0.934635909121122,3.97664188950694,50.506126684581));
#9386=CARTESIAN_POINT('Ctrl Pts',(0.818363240305797,4.00396962344519,50.5119289847633));
#9387=CARTESIAN_POINT('Ctrl Pts',(0.700936875202572,4.026182839741,50.5177312849457));
#9388=CARTESIAN_POINT('Ctrl Pts',(0.582843859901059,4.04320640519077,50.5235335851281));
#9389=CARTESIAN_POINT('Ctrl Pts',(0.464621020012701,4.06024868535745,50.5293422640215));
#9390=CARTESIAN_POINT('Ctrl Pts',(0.345730471955937,4.07208986877292,50.535150942915));
#9391=CARTESIAN_POINT('Ctrl Pts',(0.226664622678819,4.07870667599741,50.5409596218084));
#9392=CARTESIAN_POINT('Ctrl Pts',(0.107520475418681,4.08532783444993,50.5467721205028));
#9393=CARTESIAN_POINT('Ctrl Pts',(-0.0117987948272657,4.08671777019441,
50.5525846191972));
#9394=CARTESIAN_POINT('Ctrl Pts',(-0.130802197900687,4.08290531178772,50.5583971178916));
#9395=CARTESIAN_POINT('Ctrl Pts',(-0.2499739328687,4.07908746060796,50.5642178384426));
#9396=CARTESIAN_POINT('Ctrl Pts',(-0.368828502858761,4.07005255946358,50.5700385589936));
#9397=CARTESIAN_POINT('Ctrl Pts',(-0.486881335483542,4.05588110836077,50.5758592795445));
#9398=CARTESIAN_POINT('Ctrl Pts',(-0.51393925465946,4.05263298656631,50.5771933990461));
#9399=CARTESIAN_POINT('Ctrl Pts',(-0.5409551053352,4.04911523465669,50.5785275185476));
#9400=CARTESIAN_POINT('Ctrl Pts',(-0.567923149774569,4.04532919500381,50.5798616380491));
#9401=CARTESIAN_POINT('Ctrl Pts',(-0.685726289369142,4.02879083017196,50.5856894045461));
#9402=CARTESIAN_POINT('Ctrl Pts',(-0.802993418979347,4.00707616775879,50.5915171710431));
#9403=CARTESIAN_POINT('Ctrl Pts',(-0.919235126998391,3.98023011662545,50.5973449375401));
#9404=CARTESIAN_POINT('Ctrl Pts',(-1.0353315133892,3.95341762755799,50.6031654183517));
#9405=CARTESIAN_POINT('Ctrl Pts',(-1.15040463430047,3.9214866007382,50.6089858991633));
#9406=CARTESIAN_POINT('Ctrl Pts',(-1.26397159091224,3.88453353922537,50.6148063799749));
#9407=CARTESIAN_POINT('Ctrl Pts',(-1.37742604064251,3.84761708584079,50.6206210946361));
#9408=CARTESIAN_POINT('Ctrl Pts',(-1.48937690910271,3.80568862107416,50.6264358092974));
#9409=CARTESIAN_POINT('Ctrl Pts',(-1.59935344743643,3.75889525661107,50.6322505239587));
#9410=CARTESIAN_POINT('Ctrl Pts',(-1.71272719878724,3.71065642905853,50.6382448571516));
#9411=CARTESIAN_POINT('Ctrl Pts',(-1.82400223363396,3.65724736251386,50.6442391903446));
#9412=CARTESIAN_POINT('Ctrl Pts',(-1.93268140335395,3.59888421502135,50.6502335235376));
#9413=CARTESIAN_POINT('Ctrl Pts',(-2.0379873814761,3.54233254694345,50.6560418042016));
#9414=CARTESIAN_POINT('Ctrl Pts',(-2.14085586804854,3.48112998805264,50.6618500848658));
#9415=CARTESIAN_POINT('Ctrl Pts',(-2.24085734570053,3.4155209494629,50.6676583655299));
#9416=CARTESIAN_POINT('Ctrl Pts',(-2.34084446549131,3.34992133078868,50.6734658122614));
#9417=CARTESIAN_POINT('Ctrl Pts',(-2.43796505430244,3.27991671423282,50.6792732589929));
#9418=CARTESIAN_POINT('Ctrl Pts',(-2.53181760052623,3.20579547658075,50.6850807057245));
#9419=CARTESIAN_POINT('Ctrl Pts',(-2.62567872512337,3.13166746404962,50.6908886832722));
#9420=CARTESIAN_POINT('Ctrl Pts',(-2.71627089332352,3.05342233495526,50.6966966608199));
#9421=CARTESIAN_POINT('Ctrl Pts',(-2.80322528081623,2.97138907331113,50.7025046383675));
#9422=CARTESIAN_POINT('Ctrl Pts',(-2.89020804844925,2.88932903768189,50.7083145115208));
#9423=CARTESIAN_POINT('Ctrl Pts',(-2.97355037769829,2.80347869014922,50.714124384674));
#9424=CARTESIAN_POINT('Ctrl Pts',(-3.05292040165361,2.71420375454149,50.7199342578272));
#9425=CARTESIAN_POINT('Ctrl Pts',(-3.13237744299417,2.62483094229122,50.7257505006392));
#9426=CARTESIAN_POINT('Ctrl Pts',(-3.20785321528757,2.53202635258575,50.7315667434512));
#9427=CARTESIAN_POINT('Ctrl Pts',(-3.27905615631144,2.43618877013996,50.7373829862632));
#9428=CARTESIAN_POINT('Ctrl Pts',(-3.35030590092513,2.34028819109833,50.7432030522465));
#9429=CARTESIAN_POINT('Ctrl Pts',(-3.41727699259905,2.24135098549292,50.7490231182298));
#9430=CARTESIAN_POINT('Ctrl Pts',(-3.47972211153957,2.13980350183436,50.7548431842132));
#9431=CARTESIAN_POINT('Ctrl Pts',(-3.54225489158131,2.0381134647722,50.7606714204651));
#9432=CARTESIAN_POINT('Ctrl Pts',(-3.60024882084813,1.933806191218,50.766499656717));
#9433=CARTESIAN_POINT('Ctrl Pts',(-3.65350321437514,1.82733118578723,50.7723278929689));
#9434=CARTESIAN_POINT('Ctrl Pts',(-3.66503640948176,1.80427211159105,50.7735901021758));
#9435=CARTESIAN_POINT('Ctrl Pts',(-3.67634749467981,1.78111143438283,50.7748523113828));
#9436=CARTESIAN_POINT('Ctrl Pts',(-3.68743473585548,1.7578538246414,50.7761145205898));
#9437=CARTESIAN_POINT('Ctrl Pts',(-3.74247739978587,1.64239130546845,50.782380764472));
#9438=CARTESIAN_POINT('Ctrl Pts',(-3.79215297082213,1.52421596465456,50.7886470083543));
#9439=CARTESIAN_POINT('Ctrl Pts',(-3.83620714792583,1.40383037372853,50.7949132522366));
#9440=CARTESIAN_POINT('Ctrl Pts',(-3.88012390350456,1.28382031067697,50.8011599493506));
#9441=CARTESIAN_POINT('Ctrl Pts',(-3.91845412677658,1.16161403697445,50.8074066464647));
#9442=CARTESIAN_POINT('Ctrl Pts',(-3.95099138915027,1.03773409063231,50.8136533435787));
#9443=CARTESIAN_POINT('Ctrl Pts',(-3.98346592666386,0.914092958244832,50.8198879984011));
#9444=CARTESIAN_POINT('Ctrl Pts',(-4.01016967757586,0.788784880497225,50.8261226532235));
#9445=CARTESIAN_POINT('Ctrl Pts',(-4.03094500985105,0.662349852839839,50.8323573080459));
#9446=CARTESIAN_POINT('Ctrl Pts',(-4.05165968241143,0.53628398956535,50.8385737589533));
#9447=CARTESIAN_POINT('Ctrl Pts',(-4.06648039935784,0.40909804205386,50.8447902098606));
#9448=CARTESIAN_POINT('Ctrl Pts',(-4.07530010119103,0.281343358251793,50.851006660768));
#9449=CARTESIAN_POINT('Ctrl Pts',(-4.08173580692684,0.188121210057571,50.8555427833624));
#9450=CARTESIAN_POINT('Ctrl Pts',(-4.08497724620056,0.0945965863802722,
50.8600789059567));
#9451=CARTESIAN_POINT('Ctrl Pts',(-4.08499988058316,0.000987742680465642,
50.8646150285511));
#9452=CARTESIAN_POINT('Ctrl Pts',(-4.08499988058338,0.000987741764322645,
50.8646150285955));
#9453=CARTESIAN_POINT('Ctrl Pts',(-4.08502967467695,-0.122231578376562,
50.8705860236432));
#9454=CARTESIAN_POINT('Ctrl Pts',(-4.07947997096532,-0.24539499124926,50.8765570186908));
#9455=CARTESIAN_POINT('Ctrl Pts',(-4.06839208895291,-0.367982079108958,
50.8825280137385));
#9456=CARTESIAN_POINT('Ctrl Pts',(-4.05729609641797,-0.490658836513985,
50.8885033764273));
#9457=CARTESIAN_POINT('Ctrl Pts',(-4.04065388598581,-0.612758056698495,
50.8944787391161));
#9458=CARTESIAN_POINT('Ctrl Pts',(-4.01855840692874,-0.7337665365103,50.9004541018049));
#9459=CARTESIAN_POINT('Ctrl Pts',(-3.99639854085159,-0.855127639381329,
50.9064468769154));
#9460=CARTESIAN_POINT('Ctrl Pts',(-3.96875366769712,-0.975391269297092,
50.9124396520259));
#9461=CARTESIAN_POINT('Ctrl Pts',(-3.93576823229061,-1.09405366490498,50.9184324271363));
#9462=CARTESIAN_POINT('Ctrl Pts',(-3.90279218938141,-1.21268227177498,50.9244234958232));
#9463=CARTESIAN_POINT('Ctrl Pts',(-3.86447878240159,-1.32971021344599,50.9304145645101));
#9464=CARTESIAN_POINT('Ctrl Pts',(-3.82102101337489,-1.44465338934553,50.936405633197));
#9465=CARTESIAN_POINT('Ctrl Pts',(-3.77747245573135,-1.55983669565648,50.9424092179622));
#9466=CARTESIAN_POINT('Ctrl Pts',(-3.72875819676169,-1.67292618416678,50.9484128027274));
#9467=CARTESIAN_POINT('Ctrl Pts',(-3.67511885388689,-1.78345911357819,50.9544163874925));
#9468=CARTESIAN_POINT('Ctrl Pts',(-3.6216574237353,-1.89362542376159,50.9604000593718));
#9469=CARTESIAN_POINT('Ctrl Pts',(-3.56330377686136,-2.00125182718268,50.9663837312511));
#9470=CARTESIAN_POINT('Ctrl Pts',(-3.50033892327115,-2.105908930185,50.9723674031304));
#9471=CARTESIAN_POINT('Ctrl Pts',(-3.43902918689205,-2.20781497823259,50.9781937860183));
#9472=CARTESIAN_POINT('Ctrl Pts',(-3.37316769210698,-2.30720406476472,50.9840201689062));
#9473=CARTESIAN_POINT('Ctrl Pts',(-3.30298702653468,-2.40364342250334,50.9898465517941));
#9474=CARTESIAN_POINT('Ctrl Pts',(-3.23291250694739,-2.49993691883502,50.9956641224665));
#9475=CARTESIAN_POINT('Ctrl Pts',(-3.15853205917908,-2.59328924068462,51.0014816931389));
#9476=CARTESIAN_POINT('Ctrl Pts',(-3.08012300868858,-2.68329410451915,51.0072992638113));
#9477=CARTESIAN_POINT('Ctrl Pts',(-3.00178278679312,-2.77321996078648,51.0131117277362));
#9478=CARTESIAN_POINT('Ctrl Pts',(-2.91942125901157,-2.85980389522568,51.0189241916612));
#9479=CARTESIAN_POINT('Ctrl Pts',(-2.83335766623238,-2.94267044284646,51.0247366555862));
#9480=CARTESIAN_POINT('Ctrl Pts',(-2.74735299251528,-3.02548026009955,51.0305451403033));
#9481=CARTESIAN_POINT('Ctrl Pts',(-2.65765158807283,-3.10457747088664,51.0363536250205));
#9482=CARTESIAN_POINT('Ctrl Pts',(-2.5646109376554,-3.17962194898361,51.0421621097376));
#9483=CARTESIAN_POINT('Ctrl Pts',(-2.48332874727353,-3.24518231994423,51.0472365192402));
#9484=CARTESIAN_POINT('Ctrl Pts',(-2.39949871580841,-3.30765000597534,51.0523109287428));
#9485=CARTESIAN_POINT('Ctrl Pts',(-2.31338095599002,-3.36682247118299,51.0573853382455));
#9486=CARTESIAN_POINT('Origin',(0.,0.,0.));
#9487=CARTESIAN_POINT('',(-3.38700661857411,0.136349654327207,58.7578931987404));
#9488=CARTESIAN_POINT('',(-3.38228028396882,0.136179104830184,59.1010527180904));
#9489=CARTESIAN_POINT('',(-3.38700661857411,0.136349654327212,0.));
#9490=CARTESIAN_POINT('',(-3.38941152592639,0.000621225212723754,59.1089821571774));
#9491=CARTESIAN_POINT('Ctrl Pts',(-3.3822802839685,0.136179104839289,59.1010527180899));
#9492=CARTESIAN_POINT('Ctrl Pts',(-3.38391039591696,0.0910238355186148,
59.1036956766094));
#9493=CARTESIAN_POINT('Ctrl Pts',(-3.38468059381083,0.045828374490169,59.1063386351288));
#9494=CARTESIAN_POINT('Ctrl Pts',(-3.38459238031828,0.000629980057637551,
59.1089815936483));
#9495=CARTESIAN_POINT('',(0.784811935329644,3.29764693208114,60.));
#9496=CARTESIAN_POINT('Ctrl Pts',(-3.38974994318795,0.00062061041689021,
59.1089821967504));
#9497=CARTESIAN_POINT('Ctrl Pts',(-3.38976958113811,-0.106641109035038,
59.1152447433034));
#9498=CARTESIAN_POINT('Ctrl Pts',(-3.38469376469629,-0.213844138759583,
59.1215072898564));
#9499=CARTESIAN_POINT('Ctrl Pts',(-3.37456524596793,-0.320490972112212,
59.1277698364093));
#9500=CARTESIAN_POINT('Ctrl Pts',(-3.36442804830286,-0.427229189125262,
59.1340377492204));
#9501=CARTESIAN_POINT('Ctrl Pts',(-3.34922955936844,-0.533409872464934,
59.1403056620314));
#9502=CARTESIAN_POINT('Ctrl Pts',(-3.32906407250675,-0.638543235532868,
59.1465735748424));
#9503=CARTESIAN_POINT('Ctrl Pts',(-3.30886074569859,-0.743873878282574,
59.1528532492085));
#9504=CARTESIAN_POINT('Ctrl Pts',(-3.28367187382311,-0.848152890830866,
59.1591329235747));
#9505=CARTESIAN_POINT('Ctrl Pts',(-3.25364250612429,-0.950902468627188,
59.1654125979408));
#9506=CARTESIAN_POINT('Ctrl Pts',(-3.2235828914976,-1.05375554041308,59.171698597477));
#9507=CARTESIAN_POINT('Ctrl Pts',(-3.18867318755257,-1.15507573799927,59.1779845970132));
#9508=CARTESIAN_POINT('Ctrl Pts',(-3.14910709129851,-1.25440407765338,59.1842705965494));
#9509=CARTESIAN_POINT('Ctrl Pts',(-3.10945856420961,-1.35393935503287,59.1905696921511));
#9510=CARTESIAN_POINT('Ctrl Pts',(-3.06513441912835,-1.45147412624603,59.1968687877528));
#9511=CARTESIAN_POINT('Ctrl Pts',(-3.01637526412841,-1.54657212196983,59.2031678833546));
#9512=CARTESIAN_POINT('Ctrl Pts',(-2.98587555195019,-1.60605759702173,59.2071080788488));
#9513=CARTESIAN_POINT('Ctrl Pts',(-2.95364144219183,-1.66459015785701,59.2110482743431));
#9514=CARTESIAN_POINT('Ctrl Pts',(-2.91974031768174,-1.72206897068721,59.2149884698374));
#9515=CARTESIAN_POINT('Ctrl Pts',(-2.86712558833523,-1.81127640034992,59.2211036746426));
#9516=CARTESIAN_POINT('Ctrl Pts',(-2.81033235993871,-1.89821685460951,59.2272188794477));
#9517=CARTESIAN_POINT('Ctrl Pts',(-2.74958134053344,-1.98247509802528,59.2333340842529));
#9518=CARTESIAN_POINT('Ctrl Pts',(-2.68890965946338,-2.06662330363714,59.2394413028518));
#9519=CARTESIAN_POINT('Ctrl Pts',(-2.62429071108117,-2.14809592057705,59.2455485214508));
#9520=CARTESIAN_POINT('Ctrl Pts',(-2.55599019115997,-2.22650380758579,59.2516557400497));
#9521=CARTESIAN_POINT('Ctrl Pts',(-2.4877595740189,-2.30483144733883,59.2577567081609));
#9522=CARTESIAN_POINT('Ctrl Pts',(-2.41585515688706,-2.38010027576606,59.2638576762722));
#9523=CARTESIAN_POINT('Ctrl Pts',(-2.34058436746746,-2.45195225917368,59.2699586443834));
#9524=CARTESIAN_POINT('Ctrl Pts',(-2.26536746257994,-2.52375280548952,59.2760552449596));
#9525=CARTESIAN_POINT('Ctrl Pts',(-2.1867892855036,-2.59214107869901,59.2821518455358));
#9526=CARTESIAN_POINT('Ctrl Pts',(-2.10519520272108,-2.65679472691063,59.288248446112));
#9527=CARTESIAN_POINT('Ctrl Pts',(-2.0236315585697,-2.72142425611164,59.2943427723544));
#9528=CARTESIAN_POINT('Ctrl Pts',(-1.93905457831871,-2.78232166560899,59.3004370985968));
#9529=CARTESIAN_POINT('Ctrl Pts',(-1.8518433121115,-2.83920436212117,59.3065314248393));
#9530=CARTESIAN_POINT('Ctrl Pts',(-1.76464226969447,-2.89608039026607,59.3126250366429));
#9531=CARTESIAN_POINT('Ctrl Pts',(-1.67480791200506,-2.94894240899023,59.3187186484465));
#9532=CARTESIAN_POINT('Ctrl Pts',(-1.58274817452861,-2.99755121366197,59.3248122602502));
#9533=CARTESIAN_POINT('Ctrl Pts',(-1.49067567919406,-3.04616675465786,59.3309067165211));
#9534=CARTESIAN_POINT('Ctrl Pts',(-1.39637756776693,-3.09052771183969,59.337001172792));
#9535=CARTESIAN_POINT('Ctrl Pts',(-1.30028546643281,-3.13044130567618,59.3430956290629));
#9536=CARTESIAN_POINT('Ctrl Pts',(-1.20409757987879,-3.17039468563776,59.3491961603267));
#9537=CARTESIAN_POINT('Ctrl Pts',(-1.10611252594308,-3.20589168543545,59.3552966915905));
#9538=CARTESIAN_POINT('Ctrl Pts',(-1.00678092200151,-3.23678810514278,59.3613972228543));
#9539=CARTESIAN_POINT('Ctrl Pts',(-0.907397221978165,-3.26770072898196,
59.3675009536413));
#9540=CARTESIAN_POINT('Ctrl Pts',(-0.806665976843181,-3.29400785806359,
59.3736046844284));
#9541=CARTESIAN_POINT('Ctrl Pts',(-0.705050068363768,-3.31561600062496,
59.3797084152154));
#9542=CARTESIAN_POINT('Ctrl Pts',(-0.603275798898071,-3.33725781790143,
59.385821658222));
#9543=CARTESIAN_POINT('Ctrl Pts',(-0.500614532174362,-3.354185950616,59.3919349012286));
#9544=CARTESIAN_POINT('Ctrl Pts',(-0.397536566596506,-3.36635852824958,
59.3980481442351));
#9545=CARTESIAN_POINT('Ctrl Pts',(-0.323384486521762,-3.37511521981155,
59.4024458802828));
#9546=CARTESIAN_POINT('Ctrl Pts',(-0.24901688977199,-3.38141197800158,59.4068436163304));
#9547=CARTESIAN_POINT('Ctrl Pts',(-0.174608662886954,-3.38524989880287,
59.411241352378));
#9548=CARTESIAN_POINT('Ctrl Pts',(-0.0712383170763532,-3.39058166407979,
59.4173508313303));
#9549=CARTESIAN_POINT('Ctrl Pts',(0.032545193583603,-3.39118312805083,59.4234603102825));
#9550=CARTESIAN_POINT('Ctrl Pts',(0.136274250313483,-3.38700965324894,59.4295697892348));
#9551=CARTESIAN_POINT('Ctrl Pts',(0.239870040415355,-3.38284154034787,59.4356714189914));
#9552=CARTESIAN_POINT('Ctrl Pts',(0.343411093082286,-3.37391070268049,59.441773048748));
#9553=CARTESIAN_POINT('Ctrl Pts',(0.446426780436103,-3.36022442586942,59.4478746785046));
#9554=CARTESIAN_POINT('Ctrl Pts',(0.549339343826491,-3.34655184972031,59.4539702002183));
#9555=CARTESIAN_POINT('Ctrl Pts',(0.651727167272397,-3.32813335731369,59.460065721932));
#9556=CARTESIAN_POINT('Ctrl Pts',(0.753122600543466,-3.30502820124892,59.4661612436456));
#9557=CARTESIAN_POINT('Ctrl Pts',(0.854449270320235,-3.28193871444277,59.4722526315501));
#9558=CARTESIAN_POINT('Ctrl Pts',(0.954784473738238,-3.25416897903038,59.4783440194545));
#9559=CARTESIAN_POINT('Ctrl Pts',(1.05366943498394,-3.22182957095509,59.484435407359));
#9560=CARTESIAN_POINT('Ctrl Pts',(1.1525198355889,-3.18950146561633,59.4905246663021));
#9561=CARTESIAN_POINT('Ctrl Pts',(1.24992059666244,-3.15260699449364,59.4966139252451));
#9562=CARTESIAN_POINT('Ctrl Pts',(1.34542759362092,-3.11130674360845,59.5027031841882));
#9563=CARTESIAN_POINT('Ctrl Pts',(1.44092574753966,-3.07001031673377,59.5087918793237));
#9564=CARTESIAN_POINT('Ctrl Pts',(1.53453009476259,-3.02430909064457,59.5148805744593));
#9565=CARTESIAN_POINT('Ctrl Pts',(1.62581684242783,-2.97441164894471,59.5209692695949));
#9566=CARTESIAN_POINT('Ctrl Pts',(1.71711859007868,-2.92450600823539,59.5270589652079));
#9567=CARTESIAN_POINT('Ctrl Pts',(1.80610160734986,-2.87040298633066,59.533148660821));
#9568=CARTESIAN_POINT('Ctrl Pts',(1.89236783500343,-2.81235649225777,59.5392383564341));
#9569=CARTESIAN_POINT('Ctrl Pts',(1.97872391772104,-2.7542495368481,59.5453343950856));
#9570=CARTESIAN_POINT('Ctrl Pts',(2.06235720538278,-2.69219114507215,59.551430433737));
#9571=CARTESIAN_POINT('Ctrl Pts',(2.14289974529792,-2.62647782098043,59.5575264723884));
#9572=CARTESIAN_POINT('Ctrl Pts',(2.22348644605957,-2.56072846678559,59.5636258534503));
#9573=CARTESIAN_POINT('Ctrl Pts',(2.30097870578457,-2.49132047282192,59.5697252345122));
#9574=CARTESIAN_POINT('Ctrl Pts',(2.37504418729172,-2.4185884666292,59.5758246155741));
#9575=CARTESIAN_POINT('Ctrl Pts',(2.4492285035767,-2.34573976516061,59.5819337828222));
#9576=CARTESIAN_POINT('Ctrl Pts',(2.51997476855938,-2.26955671052065,59.5880429500703));
#9577=CARTESIAN_POINT('Ctrl Pts',(2.58698967555324,-2.19040851922214,59.5941521173184));
#9578=CARTESIAN_POINT('Ctrl Pts',(2.63577541747057,-2.13278994736818,59.5985994898518));
#9579=CARTESIAN_POINT('Ctrl Pts',(2.68258452817756,-2.07360068171943,59.6030468623852));
#9580=CARTESIAN_POINT('Ctrl Pts',(2.72731848949463,-2.01299252839168,59.6074942349187));
#9581=CARTESIAN_POINT('Ctrl Pts',(2.78816077688645,-1.93055988494842,59.613543069179));
#9582=CARTESIAN_POINT('Ctrl Pts',(2.84537453202934,-1.84521426173784,59.6195919034394));
#9583=CARTESIAN_POINT('Ctrl Pts',(2.89866549401247,-1.75731141700083,59.6256407376998));
#9584=CARTESIAN_POINT('Ctrl Pts',(2.95188611923875,-1.6695245919562,59.6316815883291));
#9585=CARTESIAN_POINT('Ctrl Pts',(3.00119401608682,-1.57918762171329,59.6377224389583));
#9586=CARTESIAN_POINT('Ctrl Pts',(3.04633616420661,-1.48668794208702,59.6437632895875));
#9587=CARTESIAN_POINT('Ctrl Pts',(3.09143222324147,-1.3942827024856,59.6497979726486));
#9588=CARTESIAN_POINT('Ctrl Pts',(3.13237079724932,-1.29971953192066,59.6558326557096));
#9589=CARTESIAN_POINT('Ctrl Pts',(3.16894357674446,-1.20341251028482,59.6618673387706));
#9590=CARTESIAN_POINT('Ctrl Pts',(3.2054922146009,-1.1071690607743,59.6678980383461));
#9591=CARTESIAN_POINT('Ctrl Pts',(3.23768063031878,-1.00918445394829,59.6739287379216));
#9592=CARTESIAN_POINT('Ctrl Pts',(3.26534803997469,-0.90989408193123,59.679959437497));
#9593=CARTESIAN_POINT('Ctrl Pts',(3.29300616308019,-0.810637036671354,59.6859881128716));
#9594=CARTESIAN_POINT('Ctrl Pts',(3.31614617738074,-0.710075516331877,59.6920167882462));
#9595=CARTESIAN_POINT('Ctrl Pts',(3.33465701319445,-0.608660551418521,59.6980454636208));
#9596=CARTESIAN_POINT('Ctrl Pts',(3.35316664186638,-0.507252200049869,59.7040737458491));
#9597=CARTESIAN_POINT('Ctrl Pts',(3.36704761369299,-0.404990943633947,59.7101020280775));
#9598=CARTESIAN_POINT('Ctrl Pts',(3.37624008473162,-0.302337481552332,59.7161303103058));
#9599=CARTESIAN_POINT('Ctrl Pts',(3.38543444239343,-0.199662951316172,59.7221598297528));
#9600=CARTESIAN_POINT('Ctrl Pts',(3.38993834900092,-0.0965964897647501,
59.7281893491998));
#9601=CARTESIAN_POINT('Ctrl Pts',(3.38974396269868,0.00639764393193157,
59.7342188686468));
#9602=CARTESIAN_POINT('Ctrl Pts',(3.38954934829926,0.10951263321651,59.7402554632649));
#9603=CARTESIAN_POINT('Ctrl Pts',(3.38464543380326,0.212554688382857,59.746292057883));
#9604=CARTESIAN_POINT('Ctrl Pts',(3.37507651961816,0.315061183299604,59.7523286525011));
#9605=CARTESIAN_POINT('Ctrl Pts',(3.36550181885814,0.417629666598875,59.7583688976073));
#9606=CARTESIAN_POINT('Ctrl Pts',(3.3512565639643,0.519661513581867,59.7644091427135));
#9607=CARTESIAN_POINT('Ctrl Pts',(3.33243646798291,0.620703028313545,59.7704493878197));
#9608=CARTESIAN_POINT('Ctrl Pts',(3.31358238495012,0.721927013057994,59.7765005409531));
#9609=CARTESIAN_POINT('Ctrl Pts',(3.29013705966018,0.822156669244242,59.7825516940866));
#9610=CARTESIAN_POINT('Ctrl Pts',(3.26224653946451,0.920951995628335,59.7886028472201));
#9611=CARTESIAN_POINT('Ctrl Pts',(3.2389792621021,1.00337061833462,59.7936509372999));
#9612=CARTESIAN_POINT('Ctrl Pts',(3.21261929588641,1.08479119739988,59.7986990273796));
#9613=CARTESIAN_POINT('Ctrl Pts',(3.18327663589853,1.16496992314933,59.8037471174594));
#9614=CARTESIAN_POINT('Ctrl Pts',(3.14686255675042,1.26447127942173,59.8100117693957));
#9615=CARTESIAN_POINT('Ctrl Pts',(3.10572884959804,1.36240134727722,59.8162764213321));
#9616=CARTESIAN_POINT('Ctrl Pts',(3.06002946255804,1.45829515214745,59.8225410732684));
#9617=CARTESIAN_POINT('Ctrl Pts',(3.01439608204426,1.55405045150688,59.8287966767702));
#9618=CARTESIAN_POINT('Ctrl Pts',(2.96421031748651,1.6477749831512,59.8350522802721));
#9619=CARTESIAN_POINT('Ctrl Pts',(2.90967481768643,1.73902200038454,59.8413078837739));
#9620=CARTESIAN_POINT('Ctrl Pts',(2.85520568671812,1.83015797145604,59.8475558743062));
#9621=CARTESIAN_POINT('Ctrl Pts',(2.79639756218108,1.91882208860135,59.8538038648385));
#9622=CARTESIAN_POINT('Ctrl Pts',(2.73349955967788,2.00459103553339,59.8600518553708));
#9623=CARTESIAN_POINT('Ctrl Pts',(2.67067421049986,2.09026091096962,59.8662926288649));
#9624=CARTESIAN_POINT('Ctrl Pts',(2.60376863072127,2.17304195745685,59.872533402359));
#9625=CARTESIAN_POINT('Ctrl Pts',(2.53307546014354,2.25253940603014,59.8787741758531));
#9626=CARTESIAN_POINT('Ctrl Pts',(2.46243000911888,2.3319831919556,59.8850107366783));
#9627=CARTESIAN_POINT('Ctrl Pts',(2.38800232095185,2.40814749359993,59.8912472975035));
#9628=CARTESIAN_POINT('Ctrl Pts',(2.3101254528726,2.48067036393193,59.8974838583287));
#9629=CARTESIAN_POINT('Ctrl Pts',(2.23228512686462,2.55315920444273,59.9037174927798));
#9630=CARTESIAN_POINT('Ctrl Pts',(2.15099913524756,2.62200974333339,59.9099511272309));
#9631=CARTESIAN_POINT('Ctrl Pts',(2.06663715137858,2.68689708530897,59.9161847616819));
#9632=CARTESIAN_POINT('Ctrl Pts',(1.9822974027976,2.75176732492789,59.922416753134));
#9633=CARTESIAN_POINT('Ctrl Pts',(1.89488359359858,2.81267620483484,59.9286487445861));
#9634=CARTESIAN_POINT('Ctrl Pts',(1.80479776397003,2.86933966160662,59.9348807360381));
#9635=CARTESIAN_POINT('Ctrl Pts',(1.71469299596977,2.92601503050276,59.941114037616));
#9636=CARTESIAN_POINT('Ctrl Pts',(1.62191542118583,2.97844297598582,59.9473473391939));
#9637=CARTESIAN_POINT('Ctrl Pts',(1.52689515218141,3.02638336248812,59.9535806407717));
#9638=CARTESIAN_POINT('Ctrl Pts',(1.43186603238507,3.07432821446279,59.9598145229589));
#9639=CARTESIAN_POINT('Ctrl Pts',(1.33459416225473,3.11778450052887,59.9660484051461));
#9640=CARTESIAN_POINT('Ctrl Pts',(1.23553234644241,3.15655902580555,59.9722822873333));
#9641=CARTESIAN_POINT('Ctrl Pts',(1.13640492145646,3.19535923165896,59.9785202982543));
#9642=CARTESIAN_POINT('Ctrl Pts',(1.03548555781407,3.22947134348404,59.9847583091752));
#9643=CARTESIAN_POINT('Ctrl Pts',(0.933245001729504,3.25875111495906,59.9909963200961));
#9644=CARTESIAN_POINT('Ctrl Pts',(0.884055110280037,3.27283817429909,59.9939975467307));
#9645=CARTESIAN_POINT('Ctrl Pts',(0.834559611961812,3.28580740796592,59.9969987733654));
#9646=CARTESIAN_POINT('Ctrl Pts',(0.784811935329691,3.29764693208113,60.));
#9647=CARTESIAN_POINT('',(-3.37882581077538,0.271921317549902,59.9999963691758));
#9648=CARTESIAN_POINT('Origin',(0.,0.,60.));
#9649=CARTESIAN_POINT('',(-3.38974910170284,-0.00246779350202193,58.7660178032823));
#9650=CARTESIAN_POINT('Ctrl Pts',(-3.37882581077538,0.271921317549902,59.9999963691758));
#9651=CARTESIAN_POINT('Ctrl Pts',(-3.3705827143447,0.374347957842939,59.9939311509688));
#9652=CARTESIAN_POINT('Ctrl Pts',(-3.35766337532631,0.476579186057627,59.9878659327618));
#9653=CARTESIAN_POINT('Ctrl Pts',(-3.34008176227551,0.578151263783581,59.9818007145547));
#9654=CARTESIAN_POINT('Ctrl Pts',(-3.32252284426811,0.679592228243256,59.9757433255719));
#9655=CARTESIAN_POINT('Ctrl Pts',(-3.30031368710692,0.780375309900067,59.9696859365891));
#9656=CARTESIAN_POINT('Ctrl Pts',(-3.27352015539963,0.88004025742712,59.9636285476062));
#9657=CARTESIAN_POINT('Ctrl Pts',(-3.24569321907837,0.983549200503179,59.9573375300823));
#9658=CARTESIAN_POINT('Ctrl Pts',(-3.2129211553574,1.08585154404973,59.9510465125584));
#9659=CARTESIAN_POINT('Ctrl Pts',(-3.17533659756997,1.18644112986391,59.9447554950345));
#9660=CARTESIAN_POINT('Ctrl Pts',(-3.13920831724097,1.28313320151276,59.938708233658));
#9661=CARTESIAN_POINT('Ctrl Pts',(-3.09863371580969,1.37824232821105,59.9326609722816));
#9662=CARTESIAN_POINT('Ctrl Pts',(-3.05378153165466,1.4713338912106,59.9266137109051));
#9663=CARTESIAN_POINT('Ctrl Pts',(-3.00894339869995,1.5643962906761,59.9205683440023));
#9664=CARTESIAN_POINT('Ctrl Pts',(-2.95983053393135,1.6554419922977,59.9145229770995));
#9665=CARTESIAN_POINT('Ctrl Pts',(-2.90665925565672,1.74405763494362,59.9084776101967));
#9666=CARTESIAN_POINT('Ctrl Pts',(-2.85349042996258,1.8326691901009,59.9024325221428));
#9667=CARTESIAN_POINT('Ctrl Pts',(-2.79626378655923,1.91885053782882,59.8963874340888));
#9668=CARTESIAN_POINT('Ctrl Pts',(-2.73524041089657,2.00221501270428,59.8903423460348));
#9669=CARTESIAN_POINT('Ctrl Pts',(-2.67420354727771,2.08559791357424,59.8842959218391));
#9670=CARTESIAN_POINT('Ctrl Pts',(-2.60936854071464,2.16616235540417,59.8782494976433));
#9671=CARTESIAN_POINT('Ctrl Pts',(-2.54103779588299,2.24355342757735,59.8722030734475));
#9672=CARTESIAN_POINT('Ctrl Pts',(-2.47263591117817,2.32102507242794,59.8661503542545));
#9673=CARTESIAN_POINT('Ctrl Pts',(-2.4007313125139,2.39531642933056,59.8600976350615));
#9674=CARTESIAN_POINT('Ctrl Pts',(-2.32566426496307,2.46610843013315,59.8540449158685));
#9675=CARTESIAN_POINT('Ctrl Pts',(-2.25055077251949,2.53694423080521,59.8479884517847));
#9676=CARTESIAN_POINT('Ctrl Pts',(-2.17227126463747,2.60427608378036,59.8419319877009));
#9677=CARTESIAN_POINT('Ctrl Pts',(-2.09119865285149,2.66782556716366,59.8358755236172));
#9678=CARTESIAN_POINT('Ctrl Pts',(-2.01000848889477,2.73146719485508,59.8298102778933));
#9679=CARTESIAN_POINT('Ctrl Pts',(-1.92601749196678,2.79131525928248,59.8237450321693));
#9680=CARTESIAN_POINT('Ctrl Pts',(-1.83962685362631,2.84713506913826,59.8176797864454));
#9681=CARTESIAN_POINT('Ctrl Pts',(-1.81571829597486,2.86258316823403,59.8160012333077));
#9682=CARTESIAN_POINT('Ctrl Pts',(-1.79162608731277,2.87772301716914,59.8143226801699));
#9683=CARTESIAN_POINT('Ctrl Pts',(-1.76735903007707,2.89255027982316,59.8126441270322));
#9684=CARTESIAN_POINT('Ctrl Pts',(-1.67896520419358,2.94655923775484,59.8065299232227));
#9685=CARTESIAN_POINT('Ctrl Pts',(-1.58795127391211,2.99659951709765,59.8004157194132));
#9686=CARTESIAN_POINT('Ctrl Pts',(-1.49470788425146,3.04240914461821,59.7943015156036));
#9687=CARTESIAN_POINT('Ctrl Pts',(-1.40158320174281,3.08816045239689,59.788195095721));
#9688=CARTESIAN_POINT('Ctrl Pts',(-1.30623508230095,3.12969163111811,59.7820886758383));
#9689=CARTESIAN_POINT('Ctrl Pts',(-1.20908150021065,3.16678496086305,59.7759822559556));
#9690=CARTESIAN_POINT('Ctrl Pts',(-1.11202415897218,3.20384154575951,59.7698818851247));
#9691=CARTESIAN_POINT('Ctrl Pts',(-1.01316530769847,3.23646887353432,59.7637815142938));
#9692=CARTESIAN_POINT('Ctrl Pts',(-0.912945011732789,3.26449635748797,59.7576811434629));
#9693=CARTESIAN_POINT('Ctrl Pts',(-0.81279147236823,3.29250517237316,59.7515848360806));
#9694=CARTESIAN_POINT('Ctrl Pts',(-0.711278700560812,3.31592012224861,59.7454885286984));
#9695=CARTESIAN_POINT('Ctrl Pts',(-0.608863371791357,3.33461998689369,59.7393922213161));
#9696=CARTESIAN_POINT('Ctrl Pts',(-0.506483110413252,3.35331344863522,59.7332980013322));
#9697=CARTESIAN_POINT('Ctrl Pts',(-0.403201324673627,3.36729495786349,59.7272037813484));
#9698=CARTESIAN_POINT('Ctrl Pts',(-0.299485598072089,3.37649425277867,59.7211095613645));
#9699=CARTESIAN_POINT('Ctrl Pts',(-0.195778851751454,3.38569275116805,59.715015869052));
#9700=CARTESIAN_POINT('Ctrl Pts',(-0.0916386632773638,3.39010982122857,
59.7089221767394));
#9701=CARTESIAN_POINT('Ctrl Pts',(0.0124624203631624,3.3897270908701,59.7028284844268));
#9702=CARTESIAN_POINT('Ctrl Pts',(0.116581120678082,3.38934429574347,59.6967337608992));
#9703=CARTESIAN_POINT('Ctrl Pts',(0.220660277360656,3.38416008768294,59.6906390373717));
#9704=CARTESIAN_POINT('Ctrl Pts',(0.324228393133874,3.37420820513285,59.6845443138442));
#9705=CARTESIAN_POINT('Ctrl Pts',(0.427904615032644,3.36424593464186,59.6784432285426));
#9706=CARTESIAN_POINT('Ctrl Pts',(0.531068306318182,3.34950609234175,59.6723421432411));
#9707=CARTESIAN_POINT('Ctrl Pts',(0.633254156655067,3.33007420871954,59.6662410579395));
#9708=CARTESIAN_POINT('Ctrl Pts',(0.735496284187732,3.31063162330334,59.6601366125644));
#9709=CARTESIAN_POINT('Ctrl Pts',(0.836759083943799,3.28649194763691,59.6540321671893));
#9710=CARTESIAN_POINT('Ctrl Pts',(0.936590396338981,3.25779119834062,59.6479277218143));
#9711=CARTESIAN_POINT('Ctrl Pts',(1.03658141668464,3.22904453421322,59.6418135106809));
#9712=CARTESIAN_POINT('Ctrl Pts',(1.13513597172525,3.19572235713619,59.6356992995476));
#9713=CARTESIAN_POINT('Ctrl Pts',(1.23181973666577,3.15800968948176,59.6295850884143));
#9714=CARTESIAN_POINT('Ctrl Pts',(1.30136430405099,3.13088299288918,59.62518714044));
#9715=CARTESIAN_POINT('Ctrl Pts',(1.36994134546611,3.10148571668628,59.6207891924658));
#9716=CARTESIAN_POINT('Ctrl Pts',(1.43739728720325,3.06990131783429,59.6163912444915));
#9717=CARTESIAN_POINT('Ctrl Pts',(1.53093592444134,3.02610441054166,59.6102927741482));
#9718=CARTESIAN_POINT('Ctrl Pts',(1.62263027937754,2.97795391002212,59.604194303805));
#9719=CARTESIAN_POINT('Ctrl Pts',(1.7120474884185,2.92562787447411,59.5980958334617));
#9720=CARTESIAN_POINT('Ctrl Pts',(1.80134670584262,2.87337088641264,59.5920054104327));
#9721=CARTESIAN_POINT('Ctrl Pts',(1.88837438447763,2.81694953136673,59.5859149874036));
#9722=CARTESIAN_POINT('Ctrl Pts',(1.97271919323224,2.75658920536832,59.5798245643746));
#9723=CARTESIAN_POINT('Ctrl Pts',(2.05697690872072,2.69629120659566,59.5737404302309));
#9724=CARTESIAN_POINT('Ctrl Pts',(2.13855691653878,2.63206257248482,59.5676562960872));
#9725=CARTESIAN_POINT('Ctrl Pts',(2.21707475798935,2.56417327417366,59.5615721619436));
#9726=CARTESIAN_POINT('Ctrl Pts',(2.2955363800184,2.49633258515955,59.5554923840901));
#9727=CARTESIAN_POINT('Ctrl Pts',(2.37093987270381,2.42483672341953,59.5494126062366));
#9728=CARTESIAN_POINT('Ctrl Pts',(2.44293259664658,2.3499968916451,59.5433328283831));
#9729=CARTESIAN_POINT('Ctrl Pts',(2.51489854712299,2.2751848921516,59.537255311546));
#9730=CARTESIAN_POINT('Ctrl Pts',(2.58345595319024,2.19703170245457,59.5311777947089));
#9731=CARTESIAN_POINT('Ctrl Pts',(2.64828849560439,2.11588589166558,59.5251002778718));
#9732=CARTESIAN_POINT('Ctrl Pts',(2.7131137731791,2.03474917370659,59.5190234420535));
#9733=CARTESIAN_POINT('Ctrl Pts',(2.7742147497887,1.95062083606934,59.5129466062352));
#9734=CARTESIAN_POINT('Ctrl Pts',(2.8313155254947,1.86388236152196,59.506869770417));
#9735=CARTESIAN_POINT('Ctrl Pts',(2.88842473940007,1.77713106899562,59.5007920365802));
#9736=CARTESIAN_POINT('Ctrl Pts',(2.94153234254682,1.6877692310256,59.4947143027435));
#9737=CARTESIAN_POINT('Ctrl Pts',(2.99040639390585,1.59620633433995,59.4886365689068));
#9738=CARTESIAN_POINT('Ctrl Pts',(3.03933077822348,1.50454914157369,59.4825525759138));
#9739=CARTESIAN_POINT('Ctrl Pts',(3.08401270199905,1.41068674191281,59.4764685829207));
#9740=CARTESIAN_POINT('Ctrl Pts',(3.12426678168413,1.31505214321147,59.4703845899277));
#9741=CARTESIAN_POINT('Ctrl Pts',(3.16454255151007,1.21936601363592,59.4642973186914));
#9742=CARTESIAN_POINT('Ctrl Pts',(3.20038557718903,1.1219061849542,59.4582100474552));
#9743=CARTESIAN_POINT('Ctrl Pts',(3.23165981215085,1.02312263244887,59.4521227762189));
#9744=CARTESIAN_POINT('Ctrl Pts',(3.26298442443984,0.924179956903502,59.4460256994524));
#9745=CARTESIAN_POINT('Ctrl Pts',(3.28972543462535,0.823909712182205,59.439928622686));
#9746=CARTESIAN_POINT('Ctrl Pts',(3.31179749576697,0.722774106849198,59.4338315459196));
#9747=CARTESIAN_POINT('Ctrl Pts',(3.32832108597023,0.647061952612234,59.4292671512633));
#9748=CARTESIAN_POINT('Ctrl Pts',(3.34222910857796,0.570865067973735,59.4247027566071));
#9749=CARTESIAN_POINT('Ctrl Pts',(3.35350482013033,0.494378886950759,59.4201383619509));
#9750=CARTESIAN_POINT('Ctrl Pts',(3.36858890646888,0.392059476517221,59.4140323417004));
#9751=CARTESIAN_POINT('Ctrl Pts',(3.37901099388049,0.288878871688489,59.4079263214499));
#9752=CARTESIAN_POINT('Ctrl Pts',(3.38468164869492,0.18529759709133,59.4018203011994));
#9753=CARTESIAN_POINT('Ctrl Pts',(3.39034491257526,0.0818513267220041,59.3957222393231));
#9754=CARTESIAN_POINT('Ctrl Pts',(3.39126903291786,-0.0219941523002653,
59.3896241774468));
#9755=CARTESIAN_POINT('Ctrl Pts',(3.38741596139382,-0.125770294562564,59.3835261155706));
#9756=CARTESIAN_POINT('Ctrl Pts',(3.3835668141757,-0.229440742101569,59.3774342644953));
#9757=CARTESIAN_POINT('Ctrl Pts',(3.37495016640692,-0.333041568791544,59.37134241342));
#9758=CARTESIAN_POINT('Ctrl Pts',(3.36157997946325,-0.436102171711884,59.3652505623446));
#9759=CARTESIAN_POINT('Ctrl Pts',(3.34821916601326,-0.539090521498238,59.3591629821092));
#9760=CARTESIAN_POINT('Ctrl Pts',(3.33011149556153,-0.641538978427963,59.3530754018738));
#9761=CARTESIAN_POINT('Ctrl Pts',(3.30732286692106,-0.742980831812695,59.3469878216383));
#9762=CARTESIAN_POINT('Ctrl Pts',(3.28454251641038,-0.844385835730001,59.3409024527593));
#9763=CARTESIAN_POINT('Ctrl Pts',(3.25708468084369,-0.944784546674081,59.3348170838802));
#9764=CARTESIAN_POINT('Ctrl Pts',(3.22506644606084,-1.04372002040419,59.3287317150011));
#9765=CARTESIAN_POINT('Ctrl Pts',(3.19305158275161,-1.14264507637259,59.3226469869026));
#9766=CARTESIAN_POINT('Ctrl Pts',(3.15647740670422,-1.24010679528403,59.316562258804));
#9767=CARTESIAN_POINT('Ctrl Pts',(3.11551073277267,-1.33566385609489,59.3104775307055));
#9768=CARTESIAN_POINT('Ctrl Pts',(3.07453780506184,-1.4312355041961,59.304391873741));
#9769=CARTESIAN_POINT('Ctrl Pts',(3.02917121550791,-1.52490152402909,59.2983062167766));
#9770=CARTESIAN_POINT('Ctrl Pts',(2.9796253644156,-1.6162418600665,59.2922205598121));
#9771=CARTESIAN_POINT('Ctrl Pts',(2.93002855914626,-1.70767613276156,59.2861286442077));
#9772=CARTESIAN_POINT('Ctrl Pts',(2.87624411312226,-1.79677956922563,59.2800367286033));
#9773=CARTESIAN_POINT('Ctrl Pts',(2.8185317074462,-1.88315800628104,59.2739448129989));
#9774=CARTESIAN_POINT('Ctrl Pts',(2.76078813751174,-1.96958308703293,59.2678496078066));
#9775=CARTESIAN_POINT('Ctrl Pts',(2.69911263613288,-2.05327989343153,59.2617544026143));
#9776=CARTESIAN_POINT('Ctrl Pts',(2.63380624001871,-2.13388606831257,59.255659197422));
#9777=CARTESIAN_POINT('Ctrl Pts',(2.56839544543498,-2.21462109981097,59.249554248466));
#9778=CARTESIAN_POINT('Ctrl Pts',(2.4993424454928,-2.29225531125116,59.2434492995099));
#9779=CARTESIAN_POINT('Ctrl Pts',(2.42698643575381,-2.36646189556625,59.2373443505539));
#9780=CARTESIAN_POINT('Ctrl Pts',(2.37381480846378,-2.42099343839043,59.2328580601727));
#9781=CARTESIAN_POINT('Ctrl Pts',(2.31886027471514,-2.47367475259768,59.2283717697915));
#9782=CARTESIAN_POINT('Ctrl Pts',(2.26226850542853,-2.52439027724442,59.2238854794102));
#9783=CARTESIAN_POINT('Ctrl Pts',(2.18524772879517,-2.59341354944284,59.2177796874599));
#9784=CARTESIAN_POINT('Ctrl Pts',(2.10493719415618,-2.65902336062621,59.2116738955096));
#9785=CARTESIAN_POINT('Ctrl Pts',(2.02167171369199,-2.72089113059632,59.2055681035593));
#9786=CARTESIAN_POINT('Ctrl Pts',(1.93851454729975,-2.78267842123632,59.1994702541944));
#9787=CARTESIAN_POINT('Ctrl Pts',(1.85241041719165,-2.8407330957871,59.1933724048295));
#9788=CARTESIAN_POINT('Ctrl Pts',(1.7637291654895,-2.8947650152131,59.1872745554646));
#9789=CARTESIAN_POINT('Ctrl Pts',(1.67513800473733,-2.94874204381543,59.1811829008819));
#9790=CARTESIAN_POINT('Ctrl Pts',(1.58397529153529,-2.99870422304866,59.1750912462992));
#9791=CARTESIAN_POINT('Ctrl Pts',(1.49064126746975,-3.04440366479483,59.1689995917165));
#9792=CARTESIAN_POINT('Ctrl Pts',(1.39737229531499,-3.09007125496236,59.1629121828928));
#9793=CARTESIAN_POINT('Ctrl Pts',(1.30193540428378,-3.13148182870483,59.1568247740691));
#9794=CARTESIAN_POINT('Ctrl Pts',(1.20475623387012,-3.1684329690639,59.1507373652453));
#9795=CARTESIAN_POINT('Ctrl Pts',(1.10761211796475,-3.20537078039319,59.1446521522741));
#9796=CARTESIAN_POINT('Ctrl Pts',(1.00872737056014,-3.23785220392031,59.1385669393029));
#9797=CARTESIAN_POINT('Ctrl Pts',(0.90854771262464,-3.26572290869641,59.1324817263317));
#9798=CARTESIAN_POINT('Ctrl Pts',(0.808378344346053,-3.2935907508156,59.1263971383851));
#9799=CARTESIAN_POINT('Ctrl Pts',(0.706914741463906,-3.31684870154608,59.1203125504385));
#9800=CARTESIAN_POINT('Ctrl Pts',(0.604617016221556,-3.33539252955261,59.1142279624919));
#9801=CARTESIAN_POINT('Ctrl Pts',(0.502303404986299,-3.35393923726266,59.108142429659));
#9802=CARTESIAN_POINT('Ctrl Pts',(0.399155834257855,-3.36777029158176,59.1020568968261));
#9803=CARTESIAN_POINT('Ctrl Pts',(0.295642918161283,-3.37683288414471,59.0959713639931));
#9804=CARTESIAN_POINT('Ctrl Pts',(0.192023105992799,-3.38590483549672,59.0898795467314));
#9805=CARTESIAN_POINT('Ctrl Pts',(0.0880376212267635,-3.39019845399246,
59.0837877294696));
#9806=CARTESIAN_POINT('Ctrl Pts',(-0.0158415490729636,-3.38971298310387,
59.0776959122079));
#9807=CARTESIAN_POINT('Ctrl Pts',(-0.119777056577213,-3.38922724892793,
59.0716007911466));
#9808=CARTESIAN_POINT('Ctrl Pts',(-0.223605708239737,-3.38395728413858,
59.0655056700853));
#9809=CARTESIAN_POINT('Ctrl Pts',(-0.326859245018531,-3.37395437083045,
59.059410549024));
#9810=CARTESIAN_POINT('Ctrl Pts',(-0.43027825514994,-3.36393542692761,59.0533056599669));
#9811=CARTESIAN_POINT('Ctrl Pts',(-0.533119886389554,-3.3491684437396,59.0472007709097));
#9812=CARTESIAN_POINT('Ctrl Pts',(-0.634924492216723,-3.32975613997232,
59.0410958818526));
#9813=CARTESIAN_POINT('Ctrl Pts',(-0.709762020412863,-3.31548597195062,
59.0366081201916));
#9814=CARTESIAN_POINT('Ctrl Pts',(-0.784039355673478,-3.29870661602957,
59.0321203585306));
#9815=CARTESIAN_POINT('Ctrl Pts',(-0.857579600464567,-3.27947591718052,
59.0276325968696));
#9816=CARTESIAN_POINT('Ctrl Pts',(-0.957605192774021,-3.2533193270255,59.0215285783208));
#9817=CARTESIAN_POINT('Ctrl Pts',(-1.05660029666248,-3.22253858110059,59.015424559772));
#9818=CARTESIAN_POINT('Ctrl Pts',(-1.15410634620905,-3.18723133834681,59.0093205412232));
#9819=CARTESIAN_POINT('Ctrl Pts',(-1.25148501946813,-3.15197021894152,59.0032244966127));
#9820=CARTESIAN_POINT('Ctrl Pts',(-1.34737810717236,-3.11219450292162,58.9971284520022));
#9821=CARTESIAN_POINT('Ctrl Pts',(-1.44133974546717,-3.06805228127498,58.9910324073917));
#9822=CARTESIAN_POINT('Ctrl Pts',(-1.53520545770926,-3.0239551247119,58.9849425862731));
#9823=CARTESIAN_POINT('Ctrl Pts',(-1.62714325687212,-2.97550050789795,58.9788527651545));
#9824=CARTESIAN_POINT('Ctrl Pts',(-1.71672571818852,-2.92288519634455,58.9727629440359));
#9825=CARTESIAN_POINT('Ctrl Pts',(-1.80624520006417,-2.87030687509983,58.9666774042635));
#9826=CARTESIAN_POINT('Ctrl Pts',(-1.89341226959328,-2.81357389188496,58.9605918644911));
#9827=CARTESIAN_POINT('Ctrl Pts',(-1.9778233931322,-2.75292929224109,58.9545063247187));
#9828=CARTESIAN_POINT('Ctrl Pts',(-2.06220376487716,-2.69230678601518,58.9484230019677));
#9829=CARTESIAN_POINT('Ctrl Pts',(-2.14382983944766,-2.62777574473887,58.9423396792167));
#9830=CARTESIAN_POINT('Ctrl Pts',(-2.22232709072012,-2.55962250426727,58.9362563564656));
#9831=CARTESIAN_POINT('Ctrl Pts',(-2.30081603298364,-2.49147647788119,58.9301736776401));
#9832=CARTESIAN_POINT('Ctrl Pts',(-2.37617648789699,-2.41970929495399,58.9240909988146));
#9833=CARTESIAN_POINT('Ctrl Pts',(-2.44806776033335,-2.34464694641144,58.9180083199891));
#9834=CARTESIAN_POINT('Ctrl Pts',(-2.51997000363706,-2.26957314308387,58.9119247129249));
#9835=CARTESIAN_POINT('Ctrl Pts',(-2.58840171704246,-2.19120348373446,58.9058411058606));
#9836=CARTESIAN_POINT('Ctrl Pts',(-2.65306039369009,-2.10989943123671,58.8997574987964));
#9837=CARTESIAN_POINT('Ctrl Pts',(-2.71778571353709,-2.02851157927908,58.8936676214052));
#9838=CARTESIAN_POINT('Ctrl Pts',(-2.77872996416887,-1.94418362945578,58.8875777440141));
#9839=CARTESIAN_POINT('Ctrl Pts',(-2.83563218486111,-1.85730858359073,58.881487866623));
#9840=CARTESIAN_POINT('Ctrl Pts',(-2.89256517573887,-1.77038655957182,58.8753946960975));
#9841=CARTESIAN_POINT('Ctrl Pts',(-2.945451565345,-1.68091506381603,58.8693015255721));
#9842=CARTESIAN_POINT('Ctrl Pts',(-2.99407584872459,-1.58931270509744,58.8632083550466));
#9843=CARTESIAN_POINT('Ctrl Pts',(-3.04277809978119,-1.49756346456133,58.8571054142928));
#9844=CARTESIAN_POINT('Ctrl Pts',(-3.08720441007919,-1.4036769222985,58.851002473539));
#9845=CARTESIAN_POINT('Ctrl Pts',(-3.12718692467644,-1.30809288685196,58.8448995327852));
#9846=CARTESIAN_POINT('Ctrl Pts',(-3.15671128899992,-1.23751058570211,58.8403929266331));
#9847=CARTESIAN_POINT('Ctrl Pts',(-3.18381354062492,-1.16600310139847,58.835886320481));
#9848=CARTESIAN_POINT('Ctrl Pts',(-3.20844371669675,-1.09375224767274,58.831379714329));
#9849=CARTESIAN_POINT('Ctrl Pts',(-3.24747463784324,-0.97925784185478,58.8242381904987));
#9850=CARTESIAN_POINT('Ctrl Pts',(-3.28040259243278,-0.86258554788198,58.8170966666684));
#9851=CARTESIAN_POINT('Ctrl Pts',(-3.30701686360868,-0.744341673096319,
58.8099551428382));
#9852=CARTESIAN_POINT('Ctrl Pts',(-3.3343070306534,-0.623094877586172,58.8026322529122));
#9853=CARTESIAN_POINT('Ctrl Pts',(-3.35495839545225,-0.50019566529006,58.7953093629862));
#9854=CARTESIAN_POINT('Ctrl Pts',(-3.36879618663337,-0.376320761351867,
58.7879864730602));
#9855=CARTESIAN_POINT('Ctrl Pts',(-3.3826339778145,-0.252445857413681,58.7806635831342));
#9856=CARTESIAN_POINT('Ctrl Pts',(-3.389658006751,-0.127595374439921,58.7733406932083));
#9857=CARTESIAN_POINT('Ctrl Pts',(-3.38974910170284,-0.00246779350203549,
58.7660178032823));
#9858=CARTESIAN_POINT('Ctrl Pts',(-3.38974910170325,-0.00246779294397778,
58.7660178032496));
#9859=CARTESIAN_POINT('Ctrl Pts',(-3.38978279105707,0.0438077493895984,
58.7633096017465));
#9860=CARTESIAN_POINT('Ctrl Pts',(-3.38886871311492,0.0900941169352991,
58.7606014002435));
#9861=CARTESIAN_POINT('Ctrl Pts',(-3.38700661857411,0.136349654327206,58.7578931987404));
#9862=CARTESIAN_POINT('Origin',(0.,0.,0.));
#9863=CARTESIAN_POINT('',(-3.38700661857411,0.136349654327205,57.5081828107941));
#9864=CARTESIAN_POINT('',(-3.38700661857411,0.136349654327218,57.8510343478015));
#9865=CARTESIAN_POINT('',(-3.38700661857411,0.136349654327212,0.));
#9866=CARTESIAN_POINT('',(-3.39333846869908,0.00164290954011615,57.8589835450503));
#9867=CARTESIAN_POINT('Ctrl Pts',(-3.38700661857411,0.136349654327218,57.8510343478015));
#9868=CARTESIAN_POINT('Ctrl Pts',(-3.38881233164404,0.0914946662507057,
57.8536836307845));
#9869=CARTESIAN_POINT('Ctrl Pts',(-3.38972753681572,0.0465908495261081,
57.8563329137674));
#9870=CARTESIAN_POINT('Ctrl Pts',(-3.38974959155796,0.00166404104890279,
57.8589821967504));
#9871=CARTESIAN_POINT('Ctrl Pts',(-3.39400293157413,0.00163899714564557,
57.8589837946813));
#9872=CARTESIAN_POINT('Ctrl Pts',(-3.38782206386631,-1.00856606823546,57.9184795879854));
#9873=CARTESIAN_POINT('Ctrl Pts',(-2.37784689341624,-3.14025136115915,58.0433930088032));
#9874=CARTESIAN_POINT('Ctrl Pts',(1.22855586861976,-3.7978891647466,58.2337240571342));
#9875=CARTESIAN_POINT('Ctrl Pts',(3.84552201587359,-1.07034770082512,58.4299769396749));
#9876=CARTESIAN_POINT('Ctrl Pts',(3.01399994759664,2.6171086526788,58.6262298222154));
#9877=CARTESIAN_POINT('Ctrl Pts',(-0.520106131442002,3.9575204291085,58.8224827047562));
#9878=CARTESIAN_POINT('Ctrl Pts',(-2.99442679320825,2.17678596204204,58.9807570033809));
#9879=CARTESIAN_POINT('Ctrl Pts',(-3.36535655531616,0.604978518233871,59.0736136744922));
#9880=CARTESIAN_POINT('Ctrl Pts',(-3.3822802839685,0.136179104839289,59.1010527180899));
#9881=CARTESIAN_POINT('',(-3.38974888547239,0.00274880677970033,57.5160178032002));
#9882=CARTESIAN_POINT('Ctrl Pts',(-3.38700661857411,0.136349654327206,58.7578931987404));
#9883=CARTESIAN_POINT('Ctrl Pts',(-3.38282665423314,0.240182457997669,58.7518139232455));
#9884=CARTESIAN_POINT('Ctrl Pts',(-3.37386618535491,0.343859661797899,58.7457346477506));
#9885=CARTESIAN_POINT('Ctrl Pts',(-3.36016005561475,0.446911023752028,58.7396553722557));
#9886=CARTESIAN_POINT('Ctrl Pts',(-3.34645455965355,0.549957620554638,58.7335763778699));
#9887=CARTESIAN_POINT('Ctrl Pts',(-3.3280038956582,0.652378009419878,58.7274973834841));
#9888=CARTESIAN_POINT('Ctrl Pts',(-3.30489460670436,0.753708631419604,58.7214183890982));
#9889=CARTESIAN_POINT('Ctrl Pts',(-3.28178041472971,0.855060752399686,58.7153381049524));
#9890=CARTESIAN_POINT('Ctrl Pts',(-3.25400572848584,0.955322230365361,58.7092578208066));
#9891=CARTESIAN_POINT('Ctrl Pts',(-3.22170766277606,1.05404212349887,58.7031775366608));
#9892=CARTESIAN_POINT('Ctrl Pts',(-3.18937349363719,1.15287236771948,58.6970904558507));
#9893=CARTESIAN_POINT('Ctrl Pts',(-3.15250598156084,1.25015717926762,58.6910033750407));
#9894=CARTESIAN_POINT('Ctrl Pts',(-3.11129136442251,1.34546315749258,58.6849162942307));
#9895=CARTESIAN_POINT('Ctrl Pts',(-3.07005235229948,1.44082554744819,58.6788256104697));
#9896=CARTESIAN_POINT('Ctrl Pts',(-3.02446129818378,1.53420638755629,58.6727349267087));
#9897=CARTESIAN_POINT('Ctrl Pts',(-2.97475071023258,1.62519638027862,58.6666442429478));
#9898=CARTESIAN_POINT('Ctrl Pts',(-2.92495694619027,1.7163386180706,58.6605433682136));
#9899=CARTESIAN_POINT('Ctrl Pts',(-2.87103010251823,1.8050816529281,58.6544424934795));
#9900=CARTESIAN_POINT('Ctrl Pts',(-2.81324647326607,1.89104451115145,58.6483416187454));
#9901=CARTESIAN_POINT('Ctrl Pts',(-2.77152577017277,1.95311106756895,58.6439366897597));
#9902=CARTESIAN_POINT('Ctrl Pts',(-2.72779540413566,2.01372892167687,58.639531760774));
#9903=CARTESIAN_POINT('Ctrl Pts',(-2.68217193456761,2.07276597229833,58.6351268317883));
#9904=CARTESIAN_POINT('Ctrl Pts',(-2.61894095240248,2.15458725266719,58.6290219040226));
#9905=CARTESIAN_POINT('Ctrl Pts',(-2.55185713164622,2.23364896070159,58.6229169762569));
#9906=CARTESIAN_POINT('Ctrl Pts',(-2.48119001523206,2.30956731246628,58.6168120484912));
#9907=CARTESIAN_POINT('Ctrl Pts',(-2.4106150404825,2.38538667556893,58.6107150808381));
#9908=CARTESIAN_POINT('Ctrl Pts',(-2.33646634760533,2.45807052070856,58.6046181131851));
#9909=CARTESIAN_POINT('Ctrl Pts',(-2.25905490583226,2.52726650651157,58.598521145532));
#9910=CARTESIAN_POINT('Ctrl Pts',(-2.18172232341004,2.59639200208217,58.5924303888847));
#9911=CARTESIAN_POINT('Ctrl Pts',(-2.10113391854465,2.66203642071304,58.5863396322374));
#9912=CARTESIAN_POINT('Ctrl Pts',(-2.01763822366384,2.72388345215258,58.5802488755901));
#9913=CARTESIAN_POINT('Ctrl Pts',(-1.93420101584568,2.78568716098478,58.5741623853959));
#9914=CARTESIAN_POINT('Ctrl Pts',(-1.84786091017546,2.84369851883857,58.5680758952017));
#9915=CARTESIAN_POINT('Ctrl Pts',(-1.75899966580321,2.89764132324969,58.5619894050075));
#9916=CARTESIAN_POINT('Ctrl Pts',(-1.67017066097764,2.95156455679419,58.555905123039));
#9917=CARTESIAN_POINT('Ctrl Pts',(-1.5788227002225,3.00142194926522,58.5498208410706));
#9918=CARTESIAN_POINT('Ctrl Pts',(-1.4853660154705,3.04698094227471,58.5437365591021));
#9919=CARTESIAN_POINT('Ctrl Pts',(-1.39191910427867,3.09253517079293,58.5376529134187));
#9920=CARTESIAN_POINT('Ctrl Pts',(-1.29636429164641,3.13379170662789,58.5315692677353));
#9921=CARTESIAN_POINT('Ctrl Pts',(-1.19913505020843,3.17056464905884,58.5254856220519));
#9922=CARTESIAN_POINT('Ctrl Pts',(-1.10189086985465,3.20734324151733,58.5194010416387));
#9923=CARTESIAN_POINT('Ctrl Pts',(-1.00297214914811,3.23963672076132,58.5133164612255));
#9924=CARTESIAN_POINT('Ctrl Pts',(-0.902830048011686,3.26730821425026,58.5072318808123));
#9925=CARTESIAN_POINT('Ctrl Pts',(-0.802584679727155,3.29500824275279,58.5011410259425));
#9926=CARTESIAN_POINT('Ctrl Pts',(-0.701113824220023,3.31807665342246,58.4950501710727));
#9927=CARTESIAN_POINT('Ctrl Pts',(-0.598881396724873,3.33642715118386,58.4889593162029));
#9928=CARTESIAN_POINT('Ctrl Pts',(-0.496593632920135,3.35478758169214,58.4828651644787));
#9929=CARTESIAN_POINT('Ctrl Pts',(-0.393543899527129,3.36842495639041,58.4767710127545));
#9930=CARTESIAN_POINT('Ctrl Pts',(-0.290201880048848,3.37730483245385,58.4706768610302));
#9931=CARTESIAN_POINT('Ctrl Pts',(-0.186694246128748,3.38619893927961,58.4645729429057));
#9932=CARTESIAN_POINT('Ctrl Pts',(-0.0828938174908368,3.39032030050129,
58.4584690247811));
#9933=CARTESIAN_POINT('Ctrl Pts',(0.0207288678506607,3.38968661922273,58.4523651066565));
#9934=CARTESIAN_POINT('Ctrl Pts',(0.0970727249459632,3.38921975549676,58.4478680541869));
#9935=CARTESIAN_POINT('Ctrl Pts',(0.173320104370365,3.38617295840839,58.4433710017173));
#9936=CARTESIAN_POINT('Ctrl Pts',(0.249285366297637,3.38057123407418,58.4388739492476));
#9937=CARTESIAN_POINT('Ctrl Pts',(0.352408029035052,3.37296690658806,58.4327692111954));
#9938=CARTESIAN_POINT('Ctrl Pts',(0.455354476334407,3.36062703606681,58.4266644731431));
#9939=CARTESIAN_POINT('Ctrl Pts',(0.557655937346654,3.34356470223653,58.4205597350908));
#9940=CARTESIAN_POINT('Ctrl Pts',(0.659823944337117,3.32652462651525,58.4144629607747));
#9941=CARTESIAN_POINT('Ctrl Pts',(0.761348219898703,3.30477440501136,58.4083661864587));
#9942=CARTESIAN_POINT('Ctrl Pts',(0.861763362557287,3.27837901552794,58.4022694121426));
#9943=CARTESIAN_POINT('Ctrl Pts',(0.962076153657685,3.2520105304453,58.3961788521716));
#9944=CARTESIAN_POINT('Ctrl Pts',(1.06128164893468,3.22100640084455,58.3900882922006));
#9945=CARTESIAN_POINT('Ctrl Pts',(1.15892377503534,3.18548281209581,58.3839977322296));
#9946=CARTESIAN_POINT('Ctrl Pts',(1.25649743506835,3.14998413227243,58.3779114429224));
#9947=CARTESIAN_POINT('Ctrl Pts',(1.35250950557861,3.10997244097856,58.3718251536152));
#9948=CARTESIAN_POINT('Ctrl Pts',(1.44651903453195,3.06561376321884,58.365738864308));
#9949=CARTESIAN_POINT('Ctrl Pts',(1.54049441616414,3.02127119797486,58.3596547857392));
#9950=CARTESIAN_POINT('Ctrl Pts',(1.6324683159849,2.97258496663961,58.3535707071704));
#9951=CARTESIAN_POINT('Ctrl Pts',(1.7220204754936,2.91976891970594,58.3474866286016));
#9952=CARTESIAN_POINT('Ctrl Pts',(1.81156323605196,2.86695841608251,58.3414031885875));
#9953=CARTESIAN_POINT('Ctrl Pts',(1.8986843937914,2.81001917588827,58.3353197485733));
#9954=CARTESIAN_POINT('Ctrl Pts',(1.98298978407304,2.74921017362478,58.3292363085592));
#9955=CARTESIAN_POINT('Ctrl Pts',(2.06730809989726,2.68839184824035,58.3231519358436));
#9956=CARTESIAN_POINT('Ctrl Pts',(2.14880944403362,2.62370283195656,58.317067563128));
#9957=CARTESIAN_POINT('Ctrl Pts',(2.22713078689163,2.55544389893018,58.3109831904125));
#9958=CARTESIAN_POINT('Ctrl Pts',(2.30553287369099,2.48711459561795,58.3048925451252));
#9959=CARTESIAN_POINT('Ctrl Pts',(2.38074808968624,2.4152083071782,58.298801899838));
#9960=CARTESIAN_POINT('Ctrl Pts',(2.45244855371389,2.34006434823632,58.2927112545508));
#9961=CARTESIAN_POINT('Ctrl Pts',(2.52418781313072,2.26487973071333,58.2866173137625));
#9962=CARTESIAN_POINT('Ctrl Pts',(2.59240825199432,2.1864542755058,58.2805233729742));
#9963=CARTESIAN_POINT('Ctrl Pts',(2.65682205553713,2.10516071303629,58.2744294321859));
#9964=CARTESIAN_POINT('Ctrl Pts',(2.72133909036212,2.02373686733206,58.2683257250854));
#9965=CARTESIAN_POINT('Ctrl Pts',(2.78203705375953,1.93943607942494,58.2622220179848));
#9966=CARTESIAN_POINT('Ctrl Pts',(2.83867115315711,1.85266055896208,58.2561183108842));
#9967=CARTESIAN_POINT('Ctrl Pts',(2.88041650865635,1.78869776995535,58.2516192294918));
#9968=CARTESIAN_POINT('Ctrl Pts',(2.91995477631312,1.72339099862094,58.2471201480994));
#9969=CARTESIAN_POINT('Ctrl Pts',(2.95720429512956,1.65690911620622,58.242621066707));
#9970=CARTESIAN_POINT('Ctrl Pts',(3.007748760591,1.56669879091099,58.2365161914959));
#9971=CARTESIAN_POINT('Ctrl Pts',(3.05424592228751,1.47402311063358,58.2304113162848));
#9972=CARTESIAN_POINT('Ctrl Pts',(3.09644810697051,1.37928031354715,58.2243064410737));
#9973=CARTESIAN_POINT('Ctrl Pts',(3.13859525242559,1.284661078083,58.2182095277163));
#9974=CARTESIAN_POINT('Ctrl Pts',(3.17645838472971,1.18798047256889,58.2121126143588));
#9975=CARTESIAN_POINT('Ctrl Pts',(3.20983497811777,1.08966255132115,58.2060157010014));
#9976=CARTESIAN_POINT('Ctrl Pts',(3.24317756125452,0.99144481457008,58.1999250003078));
#9977=CARTESIAN_POINT('Ctrl Pts',(3.27204256008405,0.891593482270475,58.1938342996142));
#9978=CARTESIAN_POINT('Ctrl Pts',(3.29627530702397,0.790553073995696,58.1877435989206));
#9979=CARTESIAN_POINT('Ctrl Pts',(3.32049107022531,0.689583480799553,58.1816571669494));
#9980=CARTESIAN_POINT('Ctrl Pts',(3.34008093841483,0.587426883153269,58.1755707349782));
#9981=CARTESIAN_POINT('Ctrl Pts',(3.35494015657279,0.484542679560132,58.1694843030069));
#9982=CARTESIAN_POINT('Ctrl Pts',(3.3697939802863,0.38169582672904,58.1634000806351));
#9983=CARTESIAN_POINT('Ctrl Pts',(3.37992050636866,0.278122315325744,58.1573158582632));
#9984=CARTESIAN_POINT('Ctrl Pts',(3.38526628596686,0.174290664110741,58.1512316358914));
#9985=CARTESIAN_POINT('Ctrl Pts',(3.39061150535953,0.0704698938276971,58.1451480511094));
#9986=CARTESIAN_POINT('Ctrl Pts',(3.39117695263656,-0.0336085358387061,
58.1390644663274));
#9987=CARTESIAN_POINT('Ctrl Pts',(3.38696121061733,-0.137472980158313,58.1329808815454));
#9988=CARTESIAN_POINT('Ctrl Pts',(3.38274482171547,-0.241353361910595,58.1268963632705));
#9989=CARTESIAN_POINT('Ctrl Pts',(3.3737458032382,-0.345019266201955,58.1208118449956));
#9990=CARTESIAN_POINT('Ctrl Pts',(3.36001477761114,-0.448001960637173,58.1147273267207));
#9991=CARTESIAN_POINT('Ctrl Pts',(3.34626959581532,-0.551090826340421,58.1086365355373));
#9992=CARTESIAN_POINT('Ctrl Pts',(3.32778272108133,-0.653494651343808,58.1025457443539));
#9993=CARTESIAN_POINT('Ctrl Pts',(3.30465631083005,-0.754752760704529,58.0964549531705));
#9994=CARTESIAN_POINT('Ctrl Pts',(3.28151738621992,-0.856065663710415,58.0903608660866));
#9995=CARTESIAN_POINT('Ctrl Pts',(3.25373403933155,-0.956231204422519,58.0842667790027));
#9996=CARTESIAN_POINT('Ctrl Pts',(3.22145840105767,-1.05480369394259,58.0781726919189));
#9997=CARTESIAN_POINT('Ctrl Pts',(3.18913104260161,-1.15353414121003,58.072068839349));
#9998=CARTESIAN_POINT('Ctrl Pts',(3.1522971644833,-1.25066603830035,58.065964986779));
#9999=CARTESIAN_POINT('Ctrl Pts',(3.11115721811499,-1.34577331920016,58.0598611342091));
#10000=CARTESIAN_POINT('Ctrl Pts',(3.08084307172125,-1.41585352811672,58.0553634841949));
#10001=CARTESIAN_POINT('Ctrl Pts',(3.04819193518403,-1.48483489285143,58.0508658341806));
#10002=CARTESIAN_POINT('Ctrl Pts',(3.01329951819504,-1.55255630369579,58.0463681841664));
#10003=CARTESIAN_POINT('Ctrl Pts',(2.96593859253262,-1.64447738516647,58.0402633371434));
#10004=CARTESIAN_POINT('Ctrl Pts',(2.91428875370229,-1.73438266965953,58.0341584901204));
#10005=CARTESIAN_POINT('Ctrl Pts',(2.8585455375631,-1.82184589693478,58.0280536430974));
#10006=CARTESIAN_POINT('Ctrl Pts',(2.80287502211957,-1.90919505405212,58.0219567580589));
#10007=CARTESIAN_POINT('Ctrl Pts',(2.74312197083997,-1.99410812869571,58.0158598730205));
#10008=CARTESIAN_POINT('Ctrl Pts',(2.6795283575144,-2.07618227614441,58.009762987982));
#10009=CARTESIAN_POINT('Ctrl Pts',(2.61599954638329,-2.15817278964649,58.0036723156984));
#10010=CARTESIAN_POINT('Ctrl Pts',(2.54863821592229,-2.2373297927258,57.9975816434148));
#10011=CARTESIAN_POINT('Ctrl Pts',(2.47772981006929,-2.31327906893959,57.9914909711312));
#10012=CARTESIAN_POINT('Ctrl Pts',(2.40687110142809,-2.38917511497254,57.9854045675859));
#10013=CARTESIAN_POINT('Ctrl Pts',(2.33247055190456,-2.46186759358317,57.9793181640407));
#10014=CARTESIAN_POINT('Ctrl Pts',(2.25485354936579,-2.53101571180672,57.9732317604954));
#10015=CARTESIAN_POINT('Ctrl Pts',(2.17726472477847,-2.60013872660894,57.9671475665483));
#10016=CARTESIAN_POINT('Ctrl Pts',(2.09646208666316,-2.66571965459013,57.9610633726011));
#10017=CARTESIAN_POINT('Ctrl Pts',(2.01280693231826,-2.72745546539473,57.954979178654));
#10018=CARTESIAN_POINT('Ctrl Pts',(1.92916054406832,-2.78918480699866,57.9488956222602));
#10019=CARTESIAN_POINT('Ctrl Pts',(1.84266257777046,-2.84706957905873,57.9428120658663));
#10020=CARTESIAN_POINT('Ctrl Pts',(1.75370564057816,-2.90084842566866,57.9367285094725));
#10021=CARTESIAN_POINT('Ctrl Pts',(1.66473505231483,-2.95463552502288,57.930644019514));
#10022=CARTESIAN_POINT('Ctrl Pts',(1.57330510906221,-3.0043152260501,57.9245595295554));
#10023=CARTESIAN_POINT('Ctrl Pts',(1.47983469569119,-3.04967118488675,57.9184750395969));
#10024=CARTESIAN_POINT('Ctrl Pts',(1.38626791299425,-3.09507390636221,57.9123842764426));
#10025=CARTESIAN_POINT('Ctrl Pts',(1.29065684406284,-3.13614379654276,57.9062935132883));
#10026=CARTESIAN_POINT('Ctrl Pts',(1.19344208163425,-3.17271194095596,57.9002027501341));
#10027=CARTESIAN_POINT('Ctrl Pts',(1.09617471138763,-3.20929987423906,57.8941086909602));
#10028=CARTESIAN_POINT('Ctrl Pts',(0.997302325330367,-3.24138107727344,
57.8880146317864));
#10029=CARTESIAN_POINT('Ctrl Pts',(0.897280583532307,-3.26883658461477,
57.8819205726125));
#10030=CARTESIAN_POINT('Ctrl Pts',(0.797098553032237,-3.29633609046637,
57.8758167474736));
#10031=CARTESIAN_POINT('Ctrl Pts',(0.695763904434107,-3.31919499893302,
57.8697129223348));
#10032=CARTESIAN_POINT('Ctrl Pts',(0.593742585796657,-3.33734547272402,
57.8636090971959));
#10033=CARTESIAN_POINT('Ctrl Pts',(0.518562689793627,-3.35072062558655,
57.8591111653392));
#10034=CARTESIAN_POINT('Ctrl Pts',(0.443010110845109,-3.36154004818632,
57.8546132334825));
#10035=CARTESIAN_POINT('Ctrl Pts',(0.367272061257948,-3.36979469634566,
57.8501153016258));
#10036=CARTESIAN_POINT('Ctrl Pts',(0.264476422700178,-3.38099833617048,
57.8440104734724));
#10037=CARTESIAN_POINT('Ctrl Pts',(0.160996214210303,-3.38751270563579,
57.8379056453191));
#10038=CARTESIAN_POINT('Ctrl Pts',(0.0572948345254091,-3.38926575594725,
57.8318008171657));
#10039=CARTESIAN_POINT('Ctrl Pts',(-0.0462712898655252,-3.39101651979603,
57.8257039513975));
#10040=CARTESIAN_POINT('Ctrl Pts',(-0.150057588315461,-3.38801830365918,
57.8196070856293));
#10041=CARTESIAN_POINT('Ctrl Pts',(-0.25359457547218,-3.38025070871838,
57.8135102198611));
#10042=CARTESIAN_POINT('Ctrl Pts',(-0.35702605129341,-3.3724910294929,57.8074195672199));
#10043=CARTESIAN_POINT('Ctrl Pts',(-0.460208297240954,-3.35997166840492,
57.8013289145787));
#10044=CARTESIAN_POINT('Ctrl Pts',(-0.562671726406928,-3.34272427681409,
57.7952382619375));
#10045=CARTESIAN_POINT('Ctrl Pts',(-0.665063334264679,-3.3254889747096,
57.7891518785136));
#10046=CARTESIAN_POINT('Ctrl Pts',(-0.766736707231087,-3.30353230334752,
57.7830654950897));
#10047=CARTESIAN_POINT('Ctrl Pts',(-0.867228101709965,-3.27693766832763,
57.7769791116657));
#10048=CARTESIAN_POINT('Ctrl Pts',(-0.967683009098095,-3.25035268946652,
57.7708949381268));
#10049=CARTESIAN_POINT('Ctrl Pts',(-1.06695637841463,-3.21913320311101,
57.7648107645878));
#10050=CARTESIAN_POINT('Ctrl Pts',(-1.16459615416106,-3.18341339763049,
57.7587265910489));
#10051=CARTESIAN_POINT('Ctrl Pts',(-1.26222569413651,-3.14769733672789,
57.7526430553259));
#10052=CARTESIAN_POINT('Ctrl Pts',(-1.35822157991567,-3.10748204170256,
57.7465595196029));
#10053=CARTESIAN_POINT('Ctrl Pts',(-1.4521492442437,-3.06295080517831,57.7404759838799));
#10054=CARTESIAN_POINT('Ctrl Pts',(-1.54609131880207,-3.01841273674378,
57.7343915148307));
#10055=CARTESIAN_POINT('Ctrl Pts',(-1.63796415544571,-2.96955759429246,
57.7283070457815));
#10056=CARTESIAN_POINT('Ctrl Pts',(-1.72735623495422,-2.91661541860849,
57.7222225767323));
#10057=CARTESIAN_POINT('Ctrl Pts',(-1.81684047570835,-2.86361866071898,
57.7161318347308));
#10058=CARTESIAN_POINT('Ctrl Pts',(-1.90383848355673,-2.80652667310344,
57.7100410927294));
#10059=CARTESIAN_POINT('Ctrl Pts',(-1.98796632453116,-2.74561376654293,
57.7039503507279));
#10060=CARTESIAN_POINT('Ctrl Pts',(-2.07213968919168,-2.68466789847996,
57.6978563128731));
#10061=CARTESIAN_POINT('Ctrl Pts',(-2.15343945909388,-2.6198972591512,57.6917622750183));
#10062=CARTESIAN_POINT('Ctrl Pts',(-2.23151505029761,-2.551616280477,57.6856682371635));
#10063=CARTESIAN_POINT('Ctrl Pts',(-2.30971576035376,-2.48322587915787,
57.6795644334009));
#10064=CARTESIAN_POINT('Ctrl Pts',(-2.38468166214938,-2.4113141971973,57.6734606296383));
#10065=CARTESIAN_POINT('Ctrl Pts',(-2.45609914174325,-2.3362324517111,57.6673568258758));
#10066=CARTESIAN_POINT('Ctrl Pts',(-2.50872952104403,-2.28090172923287,
57.6628586902789));
#10067=CARTESIAN_POINT('Ctrl Pts',(-2.55943361250277,-2.22385016738898,
57.658360554682));
#10068=CARTESIAN_POINT('Ctrl Pts',(-2.60810058429678,-2.16522894971659,
57.6538624190851));
#10069=CARTESIAN_POINT('Ctrl Pts',(-2.67373571648578,-2.08616893777884,
57.6477959696303));
#10070=CARTESIAN_POINT('Ctrl Pts',(-2.73589066789206,-2.00397965075741,
57.6417295201755));
#10071=CARTESIAN_POINT('Ctrl Pts',(-2.79425071179814,-1.91900182962799,
57.6356630707207));
#10072=CARTESIAN_POINT('Ctrl Pts',(-2.85253886398197,-1.83412868974119,
57.6296040943154));
#10073=CARTESIAN_POINT('Ctrl Pts',(-2.90704115285841,-1.74647419305729,
57.6235451179101));
#10074=CARTESIAN_POINT('Ctrl Pts',(-2.95748218850592,-1.65641304244147,
57.6174861415049));
#10075=CARTESIAN_POINT('Ctrl Pts',(-3.00787453655392,-1.56643882226191,
57.6114330134533));
#10076=CARTESIAN_POINT('Ctrl Pts',(-3.05421321077881,-1.47406293961936,
57.6053798854017));
#10077=CARTESIAN_POINT('Ctrl Pts',(-3.09626591985976,-1.37968924617648,
57.5993267573502));
#10078=CARTESIAN_POINT('Ctrl Pts',(-3.13828924777158,-1.28538148925726,
57.5932778584668));
#10079=CARTESIAN_POINT('Ctrl Pts',(-3.17603238760129,-1.18907909040798,
57.5872289595834));
#10080=CARTESIAN_POINT('Ctrl Pts',(-3.20930930246251,-1.09120981650074,
57.5811800607));
#10081=CARTESIAN_POINT('Ctrl Pts',(-3.2425771234788,-0.993367288101756,
57.5751328148469));
#10082=CARTESIAN_POINT('Ctrl Pts',(-3.27138099973524,-0.893959142898774,
57.5690855689938));
#10083=CARTESIAN_POINT('Ctrl Pts',(-3.29558359012354,-0.793431700279532,
57.5630383231407));
#10084=CARTESIAN_POINT('Ctrl Pts',(-3.31978197071577,-0.69292174339323,
57.5569921291449));
#10085=CARTESIAN_POINT('Ctrl Pts',(-3.33938056028478,-0.591293298260086,
57.5509459351491));
#10086=CARTESIAN_POINT('Ctrl Pts',(-3.35429262218253,-0.489005181232123,
57.5448997411534));
#10087=CARTESIAN_POINT('Ctrl Pts',(-3.36921114701185,-0.386672732232781,
57.5388509267193));
#10088=CARTESIAN_POINT('Ctrl Pts',(-3.3794390275335,-0.283680469449326,
57.5328021122852));
#10089=CARTESIAN_POINT('Ctrl Pts',(-3.38494119867162,-0.180494166209239,
57.5267532978511));
#10090=CARTESIAN_POINT('Ctrl Pts',(-3.38819630092862,-0.119448815176464,
57.5231747996506));
#10091=CARTESIAN_POINT('Ctrl Pts',(-3.3897984199058,-0.0583356402219657,
57.5195963014501));
#10092=CARTESIAN_POINT('Ctrl Pts',(-3.38974888547307,0.00274880593522399,
57.5160178032496));
#10093=CARTESIAN_POINT('Ctrl Pts',(-3.38974888547239,0.00274880677971095,
57.5160178032001));
#10094=CARTESIAN_POINT('Ctrl Pts',(-3.38971273417821,0.0473295354305304,
57.5134061390648));
#10095=CARTESIAN_POINT('Ctrl Pts',(-3.38879708094694,0.0918735026493397,
57.5107944749295));
#10096=CARTESIAN_POINT('Ctrl Pts',(-3.38700661857411,0.136349654327205,
57.5081828107941));
#10097=CARTESIAN_POINT('Origin',(0.,0.,0.));
#10098=CARTESIAN_POINT('',(-3.38700661857411,0.13634965432721,56.2578983182294));
#10099=CARTESIAN_POINT('',(-3.3870066172248,0.136349687844955,56.6023307114865));
#10100=CARTESIAN_POINT('',(-3.38700661857411,0.136349654327212,0.));
#10101=CARTESIAN_POINT('',(-3.3897488059115,-0.00284522785732173,56.6089821967874));
#10102=CARTESIAN_POINT('Ctrl Pts',(-3.3870066172248,0.136349687844955,56.6023307114865));
#10103=CARTESIAN_POINT('Ctrl Pts',(-3.38887261232141,0.089997269736533,
56.6048299798626));
#10104=CARTESIAN_POINT('Ctrl Pts',(-3.38978720352182,0.0436035573379319,
56.6073139437703));
#10105=CARTESIAN_POINT('Ctrl Pts',(-3.38974884178032,-0.0028021686143346,
56.6097894001601));
#10106=CARTESIAN_POINT('Ctrl Pts',(-3.3897488059115,-0.00284522785732173,
56.6089821967874));
#10107=CARTESIAN_POINT('Ctrl Pts',(-3.38964186002974,-0.130258459125678,
56.6164508124252));
#10108=CARTESIAN_POINT('Ctrl Pts',(-3.38234738719693,-0.257365485074957,
56.6239194280629));
#10109=CARTESIAN_POINT('Ctrl Pts',(-3.36799108566911,-0.383459397268334,
56.6313880437007));
#10110=CARTESIAN_POINT('Ctrl Pts',(-3.35341785295837,-0.511458654057483,
56.6389695140052));
#10111=CARTESIAN_POINT('Ctrl Pts',(-3.33156780950142,-0.638414026791939,
56.6465509843097));
#10112=CARTESIAN_POINT('Ctrl Pts',(-3.30262132280961,-0.763608185277818,
56.6541324546142));
#10113=CARTESIAN_POINT('Ctrl Pts',(-3.29044357591801,-0.816277194494058,
56.6573219686791));
#10114=CARTESIAN_POINT('Ctrl Pts',(-3.27701043211885,-0.868634749644346,
56.6605114827441));
#10115=CARTESIAN_POINT('Ctrl Pts',(-3.26233783895011,-0.920628528264424,
56.663700996809));
#10116=CARTESIAN_POINT('Ctrl Pts',(-3.23425399410816,-1.02014639771804,
56.6698058357486));
#10117=CARTESIAN_POINT('Ctrl Pts',(-3.20156546326927,-1.11854402577515,
56.6759106746882));
#10118=CARTESIAN_POINT('Ctrl Pts',(-3.16437887173264,-1.21536472658707,
56.6820155136278));
#10119=CARTESIAN_POINT('Ctrl Pts',(-3.12724078050966,-1.31205914977679,
56.6881123903802));
#10120=CARTESIAN_POINT('Ctrl Pts',(-3.08561644387675,-1.40718033914296,
56.6942092671326));
#10121=CARTESIAN_POINT('Ctrl Pts',(-3.03966266118234,-1.50028529577341,
56.700306143885));
#10122=CARTESIAN_POINT('Ctrl Pts',(-2.99375570710999,-1.59329537497332,
56.7063968076921));
#10123=CARTESIAN_POINT('Ctrl Pts',(-2.94352826842955,-1.68429292610074,
56.7124874714992));
#10124=CARTESIAN_POINT('Ctrl Pts',(-2.88918544961746,-1.77285433699972,
56.7185781353063));
#10125=CARTESIAN_POINT('Ctrl Pts',(-2.83488072008213,-1.86135367456201,
56.7246645301229));
#10126=CARTESIAN_POINT('Ctrl Pts',(-2.77646656944074,-1.94741990442321,
56.7307509249395));
#10127=CARTESIAN_POINT('Ctrl Pts',(-2.71419390788892,-2.03065420317657,
56.736837319756));
#10128=CARTESIAN_POINT('Ctrl Pts',(-2.65194385528968,-2.11385828256455,
56.7429215048227));
#10129=CARTESIAN_POINT('Ctrl Pts',(-2.58583833174825,-2.1942321326681,56.7490056898893));
#10130=CARTESIAN_POINT('Ctrl Pts',(-2.5161709647831,-2.27140677521277,56.7550898749559));
#10131=CARTESIAN_POINT('Ctrl Pts',(-2.44651089978538,-2.34857332893838,
56.7611734223277));
#10132=CARTESIAN_POINT('Ctrl Pts',(-2.37329002005761,-2.42254102484428,
56.7672569696994));
#10133=CARTESIAN_POINT('Ctrl Pts',(-2.29684094310858,-2.49297548013616,
56.7733405170712));
#10134=CARTESIAN_POINT('Ctrl Pts',(-2.22038013614038,-2.5634207425894,56.7794249978764));
#10135=CARTESIAN_POINT('Ctrl Pts',(-2.14069046205971,-2.63033139785018,
56.7855094786817));
#10136=CARTESIAN_POINT('Ctrl Pts',(-2.05813926266371,-2.69341193247191,
56.7915939594869));
#10137=CARTESIAN_POINT('Ctrl Pts',(-1.97550295369874,-2.75655750257649,
56.797684713339));
#10138=CARTESIAN_POINT('Ctrl Pts',(-1.88999956796191,-2.81586480642358,
56.803775467191));
#10139=CARTESIAN_POINT('Ctrl Pts',(-1.80202717536295,-2.87108047984612,
56.8098662210431));
#10140=CARTESIAN_POINT('Ctrl Pts',(-1.71400717777831,-2.92632603243035,
56.8159602708183));
#10141=CARTESIAN_POINT('Ctrl Pts',(-1.62351588388813,-2.97747533393892,
56.8220543205936));
#10142=CARTESIAN_POINT('Ctrl Pts',(-1.53097608683248,-3.02432096247193,
56.8281483703689));
#10143=CARTESIAN_POINT('Ctrl Pts',(-1.43828799191684,-3.07124166255989,
56.8342521860456));
#10144=CARTESIAN_POINT('Ctrl Pts',(-1.34354522606689,-3.11384473766319,
56.8403560017223));
#10145=CARTESIAN_POINT('Ctrl Pts',(-1.24719085733065,-3.15197081647195,
56.8464598173991));
#10146=CARTESIAN_POINT('Ctrl Pts',(-1.17618544640889,-3.18006666649056,
56.8509578380493));
#10147=CARTESIAN_POINT('Ctrl Pts',(-1.1043052625122,-3.20573229902079,56.8554558586995));
#10148=CARTESIAN_POINT('Ctrl Pts',(-1.03173196761373,-3.22892152420958,
56.8599538793498));
#10149=CARTESIAN_POINT('Ctrl Pts',(-0.933233438622099,-3.26039459667716,
56.8660587202288));
#10150=CARTESIAN_POINT('Ctrl Pts',(-0.83312918691071,-3.28740899750557,
56.8721635611079));
#10151=CARTESIAN_POINT('Ctrl Pts',(-0.731858946297637,-3.30980173805382,
56.8782684019869));
#10152=CARTESIAN_POINT('Ctrl Pts',(-0.630720786782408,-3.33216527300587,
56.8843652806642));
#10153=CARTESIAN_POINT('Ctrl Pts',(-0.528420075449584,-3.34991904009002,
56.8904621593415));
#10154=CARTESIAN_POINT('Ctrl Pts',(-0.425412807722758,-3.36294945033752,
56.8965590380188));
#10155=CARTESIAN_POINT('Ctrl Pts',(-0.322510508502637,-3.37596658207822,
56.902649703734));
#10156=CARTESIAN_POINT('Ctrl Pts',(-0.218903506322892,-3.38426987525457,
56.9087403694492));
#10157=CARTESIAN_POINT('Ctrl Pts',(-0.115058273113641,-3.38779672593975,
56.9148310351644));
#10158=CARTESIAN_POINT('Ctrl Pts',(-0.0112858263194771,-3.39132110461144,
56.9209174318563));
#10159=CARTESIAN_POINT('Ctrl Pts',(0.0927240936923374,-3.3900756840317,
56.9270038285482));
#10160=CARTESIAN_POINT('Ctrl Pts',(0.196500422972065,-3.38404974051384,
56.93309022524));
#10161=CARTESIAN_POINT('Ctrl Pts',(0.300239074474865,-3.37802598481817,
56.9391744121612));
#10162=CARTESIAN_POINT('Ctrl Pts',(0.403743877766324,-3.36722518059719,
56.9452585990823));
#10163=CARTESIAN_POINT('Ctrl Pts',(0.506545097994257,-3.35168869768629,
56.9513427860034));
#10164=CARTESIAN_POINT('Ctrl Pts',(0.609335543050182,-3.33615384324122,
56.9574263352068));
#10165=CARTESIAN_POINT('Ctrl Pts',(0.71142212929874,-3.31588436108925,56.9635098844102));
#10166=CARTESIAN_POINT('Ctrl Pts',(0.812342469304759,-3.29097322612382,
56.9695934336136));
#10167=CARTESIAN_POINT('Ctrl Pts',(0.913278293676121,-3.26605826900407,
56.9756779162255));
#10168=CARTESIAN_POINT('Ctrl Pts',(1.01304710150471,-3.23650034651049,56.9817623988373));
#10169=CARTESIAN_POINT('Ctrl Pts',(1.11119977064915,-3.20244283824228,56.9878468814492));
#10170=CARTESIAN_POINT('Ctrl Pts',(1.20945363351478,-3.16835021726622,56.9939376370584));
#10171=CARTESIAN_POINT('Ctrl Pts',(1.30608762594269,-3.12974888679338,57.0000283926676));
#10172=CARTESIAN_POINT('Ctrl Pts',(1.4006708312588,-3.08683110729447,57.0061191482769));
#10173=CARTESIAN_POINT('Ctrl Pts',(1.49530521850413,-3.04389010364339,57.0122131997844));
#10174=CARTESIAN_POINT('Ctrl Pts',(1.58788622756578,-2.99662819249913,57.0183072512919));
#10175=CARTESIAN_POINT('Ctrl Pts',(1.67800762340419,-2.94528359895909,57.0244013027994));
#10176=CARTESIAN_POINT('Ctrl Pts',(1.76827344064313,-2.89385672464611,57.0305051201504));
#10177=CARTESIAN_POINT('Ctrl Pts',(1.85607140987124,-2.83833432715919,57.0366089375015));
#10178=CARTESIAN_POINT('Ctrl Pts',(1.94102419005542,-2.77899804895932,57.0427127548526));
#10179=CARTESIAN_POINT('Ctrl Pts',(2.00362727638359,-2.73527217985315,57.0472107571985));
#10180=CARTESIAN_POINT('Ctrl Pts',(2.06468591806405,-2.68947610120408,57.0517087595444));
#10181=CARTESIAN_POINT('Ctrl Pts',(2.12406137954748,-2.64173585326294,57.0562067618903));
#10182=CARTESIAN_POINT('Ctrl Pts',(2.20464782856905,-2.57694112222646,57.0623116076918));
#10183=CARTESIAN_POINT('Ctrl Pts',(2.28240112429059,-2.50834752067921,57.0684164534933));
#10184=CARTESIAN_POINT('Ctrl Pts',(2.35694274785019,-2.43623191544985,57.0745212992948));
#10185=CARTESIAN_POINT('Ctrl Pts',(2.43138715149251,-2.36421036603573,57.0806181829326));
#10186=CARTESIAN_POINT('Ctrl Pts',(2.50262790623314,-2.28867623998084,57.0867150665705));
#10187=CARTESIAN_POINT('Ctrl Pts',(2.57031872641208,-2.20994721818314,57.0928119502083));
#10188=CARTESIAN_POINT('Ctrl Pts',(2.63794056735124,-2.13129842392674,57.0989026209151));
#10189=CARTESIAN_POINT('Ctrl Pts',(2.70201939034689,-2.04946153042162,57.1049932916219));
#10190=CARTESIAN_POINT('Ctrl Pts',(2.76224565651917,-1.96479108190693,57.1110839623287));
#10191=CARTESIAN_POINT('Ctrl Pts',(2.82242970964086,-1.88017997955717,57.1171703640378));
#10192=CARTESIAN_POINT('Ctrl Pts',(2.87876632891486,-1.79273961889025,57.123256765747));
#10193=CARTESIAN_POINT('Ctrl Pts',(2.93098671498355,-1.70285699314122,57.1293431674561));
#10194=CARTESIAN_POINT('Ctrl Pts',(2.98318814167932,-1.61300700059061,57.1354273594083));
#10195=CARTESIAN_POINT('Ctrl Pts',(3.03127609108103,-1.52071687430974,57.1415115513605));
#10196=CARTESIAN_POINT('Ctrl Pts',(3.07502594752727,-1.42640123546429,57.1475957433127));
#10197=CARTESIAN_POINT('Ctrl Pts',(3.11877121836459,-1.33209548224291,57.1536792975548));
#10198=CARTESIAN_POINT('Ctrl Pts',(3.15817912073798,-1.23576502620311,57.1597628517969));
#10199=CARTESIAN_POINT('Ctrl Pts',(3.19307213516039,-1.13784682719699,57.165846406039));
#10200=CARTESIAN_POINT('Ctrl Pts',(3.22797050327646,-1.03991360443757,57.1719308936911));
#10201=CARTESIAN_POINT('Ctrl Pts',(3.25835246372619,-0.940392557154895,
57.1780153813431));
#10202=CARTESIAN_POINT('Ctrl Pts',(3.28408985649337,-0.839737385720894,
57.1840998689952));
#10203=CARTESIAN_POINT('Ctrl Pts',(3.30985378392782,-0.738978441091709,
57.1901906296157));
#10204=CARTESIAN_POINT('Ctrl Pts',(3.33096347518221,-0.63708345197482,57.1962813902363));
#10205=CARTESIAN_POINT('Ctrl Pts',(3.3473415838649,-0.534517898137028,57.2023721508569));
#10206=CARTESIAN_POINT('Ctrl Pts',(3.36372855522335,-0.431896843064933,
57.208466207367));
#10207=CARTESIAN_POINT('Ctrl Pts',(3.37537879595003,-0.328604925011197,
57.214560263877));
#10208=CARTESIAN_POINT('Ctrl Pts',(3.38226691334684,-0.225112392771277,
57.2206543203871));
#10209=CARTESIAN_POINT('Ctrl Pts',(3.38916606901154,-0.12145401285063,57.2267581426756));
#10210=CARTESIAN_POINT('Ctrl Pts',(3.39128784853051,-0.0175948038696428,
57.2328619649642));
#10211=CARTESIAN_POINT('Ctrl Pts',(3.38865901194834,0.0859951349860837,
57.2389657872527));
#10212=CARTESIAN_POINT('Ctrl Pts',(3.38672180256772,0.162331337339262,57.2434637396454));
#10213=CARTESIAN_POINT('Ctrl Pts',(3.38220594902991,0.238521339296662,57.2479616920382));
#10214=CARTESIAN_POINT('Ctrl Pts',(3.37514004745206,0.314379901687965,57.252459644431));
#10215=CARTESIAN_POINT('Ctrl Pts',(3.3655498818297,0.417338620995183,57.2585644716682));
#10216=CARTESIAN_POINT('Ctrl Pts',(3.3512282943769,0.520029839227596,57.2646692989055));
#10217=CARTESIAN_POINT('Ctrl Pts',(3.33219741053062,0.621985112163518,57.2707741261427));
#10218=CARTESIAN_POINT('Ctrl Pts',(3.31319134761721,0.723807410456397,57.2768709911903));
#10219=CARTESIAN_POINT('Ctrl Pts',(3.2894882771873,0.824895255252237,57.2829678562378));
#10220=CARTESIAN_POINT('Ctrl Pts',(3.26116214807592,0.924784572998947,57.2890647212854));
#10221=CARTESIAN_POINT('Ctrl Pts',(3.23286488434433,1.02457209981326,57.2951553734006));
#10222=CARTESIAN_POINT('Ctrl Pts',(3.19995404621545,1.12316311943898,57.3012460255157));
#10223=CARTESIAN_POINT('Ctrl Pts',(3.16255460053077,1.2201038731033,57.3073366776309));
#10224=CARTESIAN_POINT('Ctrl Pts',(3.12518136802837,1.31697668122459,57.3134230608225));
#10225=CARTESIAN_POINT('Ctrl Pts',(3.08332593766757,1.4122011261315,57.3195094440141));
#10226=CARTESIAN_POINT('Ctrl Pts',(3.03716281489217,1.50533952925453,57.3255958272058));
#10227=CARTESIAN_POINT('Ctrl Pts',(2.9910164519659,1.59844411781974,57.3316800006928));
#10228=CARTESIAN_POINT('Ctrl Pts',(2.94056569453136,1.68946378749746,57.3377641741799));
#10229=CARTESIAN_POINT('Ctrl Pts',(2.88603246536578,1.77798247217309,57.3438483476669));
#10230=CARTESIAN_POINT('Ctrl Pts',(2.83150495141147,1.86649187988141,57.3499318835182));
#10231=CARTESIAN_POINT('Ctrl Pts',(2.77289604067865,1.95250046012701,57.3560154193695));
#10232=CARTESIAN_POINT('Ctrl Pts',(2.71047226819966,2.03561910627224,57.3620989552208));
#10233=CARTESIAN_POINT('Ctrl Pts',(2.6480389169188,2.11875050680593,57.3681834245783));
#10234=CARTESIAN_POINT('Ctrl Pts',(2.58178979742299,2.19899075056465,57.3742678939359));
#10235=CARTESIAN_POINT('Ctrl Pts',(2.51203263613444,2.27598266634337,57.3803523632935));
#10236=CARTESIAN_POINT('Ctrl Pts',(2.44220355359522,2.35305396257238,57.3864431058801));
#10237=CARTESIAN_POINT('Ctrl Pts',(2.36885949378041,2.42686992552575,57.3925338484666));
#10238=CARTESIAN_POINT('Ctrl Pts',(2.29234603865026,2.49710926905181,57.3986245910532));
#10239=CARTESIAN_POINT('Ctrl Pts',(2.21579117822909,2.56738662263055,57.4047186296479));
#10240=CARTESIAN_POINT('Ctrl Pts',(2.13606383375847,2.63408322725902,57.4108126682425));
#10241=CARTESIAN_POINT('Ctrl Pts',(2.05354222432641,2.69691849995667,57.4169067068372));
#10242=CARTESIAN_POINT('Ctrl Pts',(1.97088836784478,2.75985447087725,57.4230105115844));
#10243=CARTESIAN_POINT('Ctrl Pts',(1.88543165288359,2.81891650580038,57.4291143163316));
#10244=CARTESIAN_POINT('Ctrl Pts',(1.79757894289601,2.87386760421507,57.4352181210788));
#10245=CARTESIAN_POINT('Ctrl Pts',(1.73283680382821,2.91436324351857,57.4397162563764));
#10246=CARTESIAN_POINT('Ctrl Pts',(1.66679403384351,2.95262724157718,57.4442143916741));
#10247=CARTESIAN_POINT('Ctrl Pts',(1.59962093464496,2.98858125670787,57.4487125269717));
#10248=CARTESIAN_POINT('Ctrl Pts',(1.50845391382177,3.03737788043381,57.4548173754785));
#10249=CARTESIAN_POINT('Ctrl Pts',(1.41489998978665,3.08208049854593,57.4609222239854));
#10250=CARTESIAN_POINT('Ctrl Pts',(1.31936209339541,3.12244915555262,57.4670270724923));
#10251=CARTESIAN_POINT('Ctrl Pts',(1.22394880286001,3.16276516150413,57.473123958715));
#10252=CARTESIAN_POINT('Ctrl Pts',(1.12655707469873,3.19875827943407,57.4792208449377));
#10253=CARTESIAN_POINT('Ctrl Pts',(1.0276147816758,3.23023419011399,57.4853177311605));
#10254=CARTESIAN_POINT('Ctrl Pts',(0.928773316141099,3.26167802515754,57.4914084043301));
#10255=CARTESIAN_POINT('Ctrl Pts',(0.828384832915229,3.28861367809401,57.4974990774997));
#10256=CARTESIAN_POINT('Ctrl Pts',(0.726896744520214,3.31089507313444,57.5035897506694));
#10257=CARTESIAN_POINT('Ctrl Pts',(0.625479793060733,3.33316085028131,57.50967615465));
#10258=CARTESIAN_POINT('Ctrl Pts',(0.522965185272561,3.35077876581744,57.5157625586307));
#10259=CARTESIAN_POINT('Ctrl Pts',(0.419814248494312,3.3636529338297,57.5218489626114));
#10260=CARTESIAN_POINT('Ctrl Pts',(0.316700764153846,3.37652242743966,57.5279331567172));
#10261=CARTESIAN_POINT('Ctrl Pts',(0.212951833497619,3.38465154396669,57.534017350823));
#10262=CARTESIAN_POINT('Ctrl Pts',(0.109036914208985,3.38799586980855,57.5401015449287));
#10263=CARTESIAN_POINT('Ctrl Pts',(0.00513288872784269,3.39133984505165,
57.5461851012046));
#10264=CARTESIAN_POINT('Ctrl Pts',(-0.0989366638004335,3.38990001342401,
57.5522686574806));
#10265=CARTESIAN_POINT('Ctrl Pts',(-0.202700162559035,3.3836840435535,57.5583522137565));
#10266=CARTESIAN_POINT('Ctrl Pts',(-0.306479579844468,3.37746712008095,
57.5644367033206));
#10267=CARTESIAN_POINT('Ctrl Pts',(-0.409952423606365,3.36647262816061,
57.5705211928848));
#10268=CARTESIAN_POINT('Ctrl Pts',(-0.512651027293548,3.35076021026794,
57.5766056824489));
#10269=CARTESIAN_POINT('Ctrl Pts',(-0.615455507529982,3.33503159374621,
57.5826964447835));
#10270=CARTESIAN_POINT('Ctrl Pts',(-0.717483730624558,3.31457540278575,
57.588787207118));
#10271=CARTESIAN_POINT('Ctrl Pts',(-0.818277078790952,3.28950265007118,
57.5948779694525));
#10272=CARTESIAN_POINT('Ctrl Pts',(-0.919124967402067,3.26441633020056,
57.6009720275689));
#10273=CARTESIAN_POINT('Ctrl Pts',(-1.01873624064291,3.23470859464613,57.6070660856853));
#10274=CARTESIAN_POINT('Ctrl Pts',(-1.11666822677616,3.20054013157289,57.6131601438017));
#10275=CARTESIAN_POINT('Ctrl Pts',(-1.21475714666922,3.16631691432188,57.6192639675063));
#10276=CARTESIAN_POINT('Ctrl Pts',(-1.31116100733615,3.1276188497666,57.6253677912109));
#10277=CARTESIAN_POINT('Ctrl Pts',(-1.40545768724504,3.08465455956803,57.6314716149155));
#10278=CARTESIAN_POINT('Ctrl Pts',(-1.47494527903619,3.05299400628238,57.6359695464478));
#10279=CARTESIAN_POINT('Ctrl Pts',(-1.5432890631108,3.01901777520069,57.6404674779801));
#10280=CARTESIAN_POINT('Ctrl Pts',(-1.61032977317947,2.98282468209443,57.6449654095124));
#10281=CARTESIAN_POINT('Ctrl Pts',(-1.70132164212005,2.93370113938277,57.651070285133));
#10282=CARTESIAN_POINT('Ctrl Pts',(-1.79021541915787,2.88032828602235,57.6571751607536));
#10283=CARTESIAN_POINT('Ctrl Pts',(-1.87658868844505,2.82290983860627,57.6632800363743));
#10284=CARTESIAN_POINT('Ctrl Pts',(-1.96284930980489,2.76556627626918,57.6693769500225));
#10285=CARTESIAN_POINT('Ctrl Pts',(-2.04659560599201,2.70418784422879,57.6754738636708));
#10286=CARTESIAN_POINT('Ctrl Pts',(-2.12742946736201,2.63902423708078,57.6815707773191));
#10287=CARTESIAN_POINT('Ctrl Pts',(-2.20818095867115,2.57392703193554,57.6876614781854));
#10288=CARTESIAN_POINT('Ctrl Pts',(-2.28602558597022,2.50505258858575,57.6937521790518));
#10289=CARTESIAN_POINT('Ctrl Pts',(-2.36059470035883,2.43269351196113,57.6998428799182));
#10290=CARTESIAN_POINT('Ctrl Pts',(-2.43511155014103,2.36038515095372,57.7059293118847));
#10291=CARTESIAN_POINT('Ctrl Pts',(-2.50635714674996,2.28459731025723,57.7120157438512));
#10292=CARTESIAN_POINT('Ctrl Pts',(-2.57399702834815,2.2056618871792,57.7181021758177));
#10293=CARTESIAN_POINT('Ctrl Pts',(-2.64161235296234,2.12675512198578,57.7241863980758));
#10294=CARTESIAN_POINT('Ctrl Pts',(-2.70562428671699,2.04470336971534,57.730270620334));
#10295=CARTESIAN_POINT('Ctrl Pts',(-2.7657368153539,1.95987370274108,57.7363548425921));
#10296=CARTESIAN_POINT('Ctrl Pts',(-2.82584304348597,1.87505292692047,57.7424384271517));
#10297=CARTESIAN_POINT('Ctrl Pts',(-2.88205043230161,1.78745516398121,57.7485220117113));
#10298=CARTESIAN_POINT('Ctrl Pts',(-2.93410523756445,1.69747798730849,57.7546055962709));
#10299=CARTESIAN_POINT('Ctrl Pts',(-2.9861680294256,1.60748700573221,57.7606901142149));
#10300=CARTESIAN_POINT('Ctrl Pts',(-3.03407675797104,1.51511625491464,57.766774632159));
#10301=CARTESIAN_POINT('Ctrl Pts',(-3.0776231889659,1.42078871379223,57.772859150103));
#10302=CARTESIAN_POINT('Ctrl Pts',(-3.12121451350251,1.32636392710206,57.7789499407899));
#10303=CARTESIAN_POINT('Ctrl Pts',(-3.16043438014796,1.22997871011556,57.7850407314767));
#10304=CARTESIAN_POINT('Ctrl Pts',(-3.19512239351121,1.13207683174914,57.7911315221635));
#10305=CARTESIAN_POINT('Ctrl Pts',(-3.22982917701831,1.03412197737859,57.7972256086579));
#10306=CARTESIAN_POINT('Ctrl Pts',(-3.25999909849915,0.93464923570353,57.8033196951523));
#10307=CARTESIAN_POINT('Ctrl Pts',(-3.28552199259297,0.834116477890183,
57.8094137816467));
#10308=CARTESIAN_POINT('Ctrl Pts',(-3.3110857853109,0.733422623476364,57.8155176334817));
#10309=CARTESIAN_POINT('Ctrl Pts',(-3.33198758973352,0.63166577852094,57.8216214853166));
#10310=CARTESIAN_POINT('Ctrl Pts',(-3.3481685573649,0.529313115247516,57.8277253371516));
#10311=CARTESIAN_POINT('Ctrl Pts',(-3.36009157867525,0.453894078933964,
57.8322229887854));
#10312=CARTESIAN_POINT('Ctrl Pts',(-3.36945248049841,0.378151716943184,
57.8367206404191));
#10313=CARTESIAN_POINT('Ctrl Pts',(-3.3762458274381,0.302273345180905,57.8412182920529));
#10314=CARTESIAN_POINT('Ctrl Pts',(-3.38118795262616,0.247072217423914,
57.8444903106358));
#10315=CARTESIAN_POINT('Ctrl Pts',(-3.38477645790119,0.191748173648244,
57.8477623292186));
#10316=CARTESIAN_POINT('Ctrl Pts',(-3.38700661857411,0.136349654327218,
57.8510343478015));
#10317=CARTESIAN_POINT('',(-3.3897497300897,-0.00135272198828424,56.2660178032046));
#10318=CARTESIAN_POINT('Ctrl Pts',(-3.38700661857411,0.136349654327205,
57.5081828107941));
#10319=CARTESIAN_POINT('Ctrl Pts',(-3.38197763548836,0.261272589263766,
57.5008472672152));
#10320=CARTESIAN_POINT('Ctrl Pts',(-3.37004365615613,0.385659014010383,
57.4935117236363));
#10321=CARTESIAN_POINT('Ctrl Pts',(-3.351341836764,0.508834900193837,57.4861761800574));
#10322=CARTESIAN_POINT('Ctrl Pts',(-3.33243756055803,0.633344228698431,
57.4787612254464));
#10323=CARTESIAN_POINT('Ctrl Pts',(-3.30661817902444,0.756616668127261,
57.4713462708354));
#10324=CARTESIAN_POINT('Ctrl Pts',(-3.27407407757502,0.877977218981941,
57.4639313162244));
#10325=CARTESIAN_POINT('Ctrl Pts',(-3.26482535208107,0.912466738454293,
57.4618240563311));
#10326=CARTESIAN_POINT('Ctrl Pts',(-3.2550338057071,0.946801975209491,57.4597167964378));
#10327=CARTESIAN_POINT('Ctrl Pts',(-3.24470450886454,0.980967742922328,
57.4576095365445));
#10328=CARTESIAN_POINT('Ctrl Pts',(-3.21478000253734,1.07994773620546,57.451504695821));
#10329=CARTESIAN_POINT('Ctrl Pts',(-3.18027237352543,1.17772228881658,57.4453998550974));
#10330=CARTESIAN_POINT('Ctrl Pts',(-3.14129669794409,1.27383677054227,57.4392950143739));
#10331=CARTESIAN_POINT('Ctrl Pts',(-3.10237185595529,1.36982589602131,57.4331981358212));
#10332=CARTESIAN_POINT('Ctrl Pts',(-3.05899071214014,1.46415886250153,57.4271012572685));
#10333=CARTESIAN_POINT('Ctrl Pts',(-3.01131825421448,1.55639565481745,57.4210043787158));
#10334=CARTESIAN_POINT('Ctrl Pts',(-2.96369437618153,1.64853845463394,57.4149137130943));
#10335=CARTESIAN_POINT('Ctrl Pts',(-2.91178807523235,1.73858895048893,57.4088230474729));
#10336=CARTESIAN_POINT('Ctrl Pts',(-2.85581227638309,1.82612740644229,57.4027323818515));
#10337=CARTESIAN_POINT('Ctrl Pts',(-2.79987571124005,1.91360450627149,57.3966459852069));
#10338=CARTESIAN_POINT('Ctrl Pts',(-2.73987554994441,1.99857270870129,57.3905595885622));
#10339=CARTESIAN_POINT('Ctrl Pts',(-2.67607005565742,2.08063791172652,57.3844731919176));
#10340=CARTESIAN_POINT('Ctrl Pts',(-2.61228772675038,2.16267331995697,57.3783890050151));
#10341=CARTESIAN_POINT('Ctrl Pts',(-2.54470307272899,2.2418074866813,57.3723048181126));
#10342=CARTESIAN_POINT('Ctrl Pts',(-2.47361651326741,2.31767694206738,57.3662206312101));
#10343=CARTESIAN_POINT('Ctrl Pts',(-2.40253740445278,2.39353844550684,57.3601370819968));
#10344=CARTESIAN_POINT('Ctrl Pts',(-2.3279574122225,2.46613560635786,57.3540535327835));
#10345=CARTESIAN_POINT('Ctrl Pts',(-2.25021529798158,2.5351402673678,57.3479699835701));
#10346=CARTESIAN_POINT('Ctrl Pts',(-2.17246125528165,2.60415551619462,57.3418855009198));
#10347=CARTESIAN_POINT('Ctrl Pts',(-2.09154444613331,2.66957688640996,57.3358010182694));
#10348=CARTESIAN_POINT('Ctrl Pts',(-2.0078376294502,2.73111572736562,57.3297165356191));
#10349=CARTESIAN_POINT('Ctrl Pts',(-1.92404451186821,2.79271801425675,57.3236257799274));
#10350=CARTESIAN_POINT('Ctrl Pts',(-1.83745598730845,2.85042952472751,57.3175350242357));
#10351=CARTESIAN_POINT('Ctrl Pts',(-1.74847475588216,2.90400431999383,57.311444268544));
#10352=CARTESIAN_POINT('Ctrl Pts',(-1.65944537357163,2.95760810647238,57.3053502169295));
#10353=CARTESIAN_POINT('Ctrl Pts',(-1.56802108103132,3.0070705154332,57.2992561653149));
#10354=CARTESIAN_POINT('Ctrl Pts',(-1.47462844538664,3.05219200093254,57.2931621137004));
#10355=CARTESIAN_POINT('Ctrl Pts',(-1.38108614551753,3.0973857948327,57.2870582962034));
#10356=CARTESIAN_POINT('Ctrl Pts',(-1.28556959457737,3.13822460130784,57.2809544787063));
#10357=CARTESIAN_POINT('Ctrl Pts',(-1.18852474005114,3.17455729272388,57.2748506612093));
#10358=CARTESIAN_POINT('Ctrl Pts',(-1.11701080816268,3.20133144403706,57.2703526588075));
#10359=CARTESIAN_POINT('Ctrl Pts',(-1.04466732731285,3.22565959362453,57.2658546564056));
#10360=CARTESIAN_POINT('Ctrl Pts',(-0.971676782487739,3.24749892884883,
57.2613566540038));
#10361=CARTESIAN_POINT('Ctrl Pts',(-0.872611577735475,3.27714000387892,
57.2552518149458));
#10362=CARTESIAN_POINT('Ctrl Pts',(-0.772023609033435,3.30229340003505,
57.2491469758878));
#10363=CARTESIAN_POINT('Ctrl Pts',(-0.670355556791719,3.32280431111711,
57.2430421368298));
#10364=CARTESIAN_POINT('Ctrl Pts',(-0.568820104711306,3.34328847092326,
57.2369452599844));
#10365=CARTESIAN_POINT('Ctrl Pts',(-0.466207785054198,3.35914209977304,
57.230848383139));
#10366=CARTESIAN_POINT('Ctrl Pts',(-0.362976620984671,3.37026008419507,
57.2247515062936));
#10367=CARTESIAN_POINT('Ctrl Pts',(-0.259850653755282,3.38136673892959,
57.2186608424187));
#10368=CARTESIAN_POINT('Ctrl Pts',(-0.156107518723505,3.38774730025256,
57.2125701785438));
#10369=CARTESIAN_POINT('Ctrl Pts',(-0.0522147683012444,3.38934782524179,
57.2064795146689));
#10370=CARTESIAN_POINT('Ctrl Pts',(0.0516051622878733,3.39094722840142,
57.2003931198226));
#10371=CARTESIAN_POINT('Ctrl Pts',(0.155574073778021,3.38777325138421,57.1943067249763));
#10372=CARTESIAN_POINT('Ctrl Pts',(0.25922078458868,3.37982390774094,57.1882203301301));
#10373=CARTESIAN_POINT('Ctrl Pts',(0.362829864626517,3.37187745024757,57.1821361450572));
#10374=CARTESIAN_POINT('Ctrl Pts',(0.466116550979529,3.35915910472149,57.1760519599843));
#10375=CARTESIAN_POINT('Ctrl Pts',(0.568611956956358,3.34171894463108,57.1699677749114));
#10376=CARTESIAN_POINT('Ctrl Pts',(0.671096619803711,3.32428061254356,57.1638842275567));
#10377=CARTESIAN_POINT('Ctrl Pts',(0.772789746067758,3.30212152180799,57.1578006802021));
#10378=CARTESIAN_POINT('Ctrl Pts',(0.873230752176608,3.27534320582639,57.1517171328474));
#10379=CARTESIAN_POINT('Ctrl Pts',(0.973687169137708,3.24856078119746,57.1456326520826));
#10380=CARTESIAN_POINT('Ctrl Pts',(1.07289067143477,3.21715783327026,57.1395481713179));
#10381=CARTESIAN_POINT('Ctrl Pts',(1.17039487321885,3.18128604549214,57.1334636905531));
#10382=CARTESIAN_POINT('Ctrl Pts',(1.26799960041298,3.14537727442397,57.1273729367774));
#10383=CARTESIAN_POINT('Ctrl Pts',(1.36390112678428,3.1049906105359,57.1212821830017));
#10384=CARTESIAN_POINT('Ctrl Pts',(1.45767217527427,3.06032627213688,57.115191429226));
#10385=CARTESIAN_POINT('Ctrl Pts',(1.55149396630011,3.01563776442516,57.1090973795472));
#10386=CARTESIAN_POINT('Ctrl Pts',(1.64318260613709,2.96666717254557,57.1030033298684));
#10387=CARTESIAN_POINT('Ctrl Pts',(1.73233634749698,2.91366021382742,57.0969092801895));
#10388=CARTESIAN_POINT('Ctrl Pts',(1.82163295999673,2.86056831010867,57.090805464641));
#10389=CARTESIAN_POINT('Ctrl Pts',(1.90838620250743,2.80342735365667,57.0847016490924));
#10390=CARTESIAN_POINT('Ctrl Pts',(1.99222402192131,2.74252593588095,57.0785978335439));
#10391=CARTESIAN_POINT('Ctrl Pts',(2.05400574576737,2.69764649362973,57.0740998128503));
#10392=CARTESIAN_POINT('Ctrl Pts',(2.11420488743103,2.65072582143083,57.0696017921567));
#10393=CARTESIAN_POINT('Ctrl Pts',(2.17268507085529,2.60189251226536,57.0651037714631));
#10394=CARTESIAN_POINT('Ctrl Pts',(2.25205603393367,2.53561456045648,57.0589989302419));
#10395=CARTESIAN_POINT('Ctrl Pts',(2.32852388960276,2.46559093453856,57.0528940890206));
#10396=CARTESIAN_POINT('Ctrl Pts',(2.4017153185982,2.39210547236336,57.0467892477993));
#10397=CARTESIAN_POINT('Ctrl Pts',(2.47481128838866,2.31871585288304,57.0406923687575));
#10398=CARTESIAN_POINT('Ctrl Pts',(2.54463902820995,2.24187367379535,57.0345954897156));
#10399=CARTESIAN_POINT('Ctrl Pts',(2.61085820328083,2.16190298229619,57.0284986106738));
#10400=CARTESIAN_POINT('Ctrl Pts',(2.67700989861407,2.08201378382797,57.0224079445725));
#10401=CARTESIAN_POINT('Ctrl Pts',(2.73956007066472,1.9990027400187,57.0163172784712));
#10402=CARTESIAN_POINT('Ctrl Pts',(2.79820580868445,1.91323007365675,57.0102266123699));
#10403=CARTESIAN_POINT('Ctrl Pts',(2.85681044147336,1.82751752599,57.0041402152614));
#10404=CARTESIAN_POINT('Ctrl Pts',(2.91151584199323,1.73904755671792,56.998053818153));
#10405=CARTESIAN_POINT('Ctrl Pts',(2.96206043373232,1.64821207659011,56.9919674210445));
#10406=CARTESIAN_POINT('Ctrl Pts',(3.01258667454523,1.55740957556319,56.9858832336883));
#10407=CARTESIAN_POINT('Ctrl Pts',(3.05895490152958,1.46424364355644,56.9797990463321));
#10408=CARTESIAN_POINT('Ctrl Pts',(3.10094822659828,1.36913299516773,56.9737148589758));
#10409=CARTESIAN_POINT('Ctrl Pts',(3.14293715023512,1.27403231557856,56.9676313093194));
#10410=CARTESIAN_POINT('Ctrl Pts',(3.18055191132357,1.17698771577332,56.961547759663));
#10411=CARTESIAN_POINT('Ctrl Pts',(3.2136231241003,1.0784393718461,56.9554642100066));
#10412=CARTESIAN_POINT('Ctrl Pts',(3.24669941113849,0.979875907213559,56.9493797269245));
#10413=CARTESIAN_POINT('Ctrl Pts',(3.27523062887567,0.879808645090815,56.9432952438423));
#10414=CARTESIAN_POINT('Ctrl Pts',(3.29909705297031,0.778693583884322,56.9372107607602));
#10415=CARTESIAN_POINT('Ctrl Pts',(3.32298808303049,0.677474274395736,56.931120004657));
#10416=CARTESIAN_POINT('Ctrl Pts',(3.34220461692821,0.575205425093327,56.9250292485538));
#10417=CARTESIAN_POINT('Ctrl Pts',(3.35667795364865,0.472353869454985,56.9189384924505));
#10418=CARTESIAN_POINT('Ctrl Pts',(3.3711591223764,0.369446657394704,56.9128444404352));
#10419=CARTESIAN_POINT('Ctrl Pts',(3.38089194118954,0.265956536251279,56.9067503884198));
#10420=CARTESIAN_POINT('Ctrl Pts',(3.38585974227279,0.162354144254032,56.9006563364044));
#10421=CARTESIAN_POINT('Ctrl Pts',(3.39083550437345,0.0585857270007194,
56.8945525185282));
#10422=CARTESIAN_POINT('Ctrl Pts',(3.39103099444868,-0.0452948930979188,
56.888448700652));
#10423=CARTESIAN_POINT('Ctrl Pts',(3.38648168568396,-0.148818194543216,
56.8823448827758));
#10424=CARTESIAN_POINT('Ctrl Pts',(3.38312922957903,-0.225106119123088,
56.8778468848247));
#10425=CARTESIAN_POINT('Ctrl Pts',(3.37720123175873,-0.301200046176631,
56.8733488868736));
#10426=CARTESIAN_POINT('Ctrl Pts',(3.36872971970812,-0.376915292944285,
56.8688508889225));
#10427=CARTESIAN_POINT('Ctrl Pts',(3.35723188668417,-0.479678679161534,
56.862746048479));
#10428=CARTESIAN_POINT('Ctrl Pts',(3.34100838685991,-0.58208686381503,56.8566412080356));
#10429=CARTESIAN_POINT('Ctrl Pts',(3.32009002990701,-0.683671891927732,
56.8505363675921));
#10430=CARTESIAN_POINT('Ctrl Pts',(3.2991989555468,-0.785124428614343,56.8444394893359));
#10431=CARTESIAN_POINT('Ctrl Pts',(3.2736252831753,-0.885755528207205,56.8383426110798));
#10432=CARTESIAN_POINT('Ctrl Pts',(3.24345155588875,-0.98510256679336,56.8322457328236));
#10433=CARTESIAN_POINT('Ctrl Pts',(3.21330857676029,-1.08434836702668,56.8261550675147));
#10434=CARTESIAN_POINT('Ctrl Pts',(3.17857498795036,-1.18231230166627,56.8200644022057));
#10435=CARTESIAN_POINT('Ctrl Pts',(3.139384150489,-1.27854300598708,56.8139737368968));
#10436=CARTESIAN_POINT('Ctrl Pts',(3.10022078222212,-1.37470626138096,56.8078873405875));
#10437=CARTESIAN_POINT('Ctrl Pts',(3.05660653873389,-1.46913830779342,56.8018009442782));
#10438=CARTESIAN_POINT('Ctrl Pts',(3.00872401291701,-1.56140477666638,56.7957145479689));
#10439=CARTESIAN_POINT('Ctrl Pts',(2.96085887155836,-1.65363774683502,56.7896303614157));
#10440=CARTESIAN_POINT('Ctrl Pts',(2.90872872446253,-1.7437063233682,56.7835461748625));
#10441=CARTESIAN_POINT('Ctrl Pts',(2.8525631728965,-1.83119862580078,56.7774619883092));
#10442=CARTESIAN_POINT('Ctrl Pts',(2.79640350821829,-1.91868175789041,56.7713784394587));
#10443=CARTESIAN_POINT('Ctrl Pts',(2.73620951100475,-2.0035887933858,56.7652948906082));
#10444=CARTESIAN_POINT('Ctrl Pts',(2.67225488715546,-2.08553563397362,56.7592113417577));
#10445=CARTESIAN_POINT('Ctrl Pts',(2.60829045048589,-2.16749504800135,56.7531268594833));
#10446=CARTESIAN_POINT('Ctrl Pts',(2.54056450364021,-2.24649302792661,56.7470423772089));
#10447=CARTESIAN_POINT('Ctrl Pts',(2.46939134461489,-2.32217816922843,56.7409578949345));
#10448=CARTESIAN_POINT('Ctrl Pts',(2.39814480697646,-2.39794134093913,56.734867139637));
#10449=CARTESIAN_POINT('Ctrl Pts',(2.3234442529993,-2.47038454153069,56.7287763843395));
#10450=CARTESIAN_POINT('Ctrl Pts',(2.24564116425911,-2.53919294735256,56.722685629042));
#10451=CARTESIAN_POINT('Ctrl Pts',(2.16779597365636,-2.60803858771219,56.7165915778324));
#10452=CARTESIAN_POINT('Ctrl Pts',(2.08684523675812,-2.67324524731672,56.7104975266229));
#10453=CARTESIAN_POINT('Ctrl Pts',(2.0031723119033,-2.73453940387115,56.7044034754133));
#10454=CARTESIAN_POINT('Ctrl Pts',(1.91936529910049,-2.79593178583949,56.6982996583347));
#10455=CARTESIAN_POINT('Ctrl Pts',(1.83282774027427,-2.85339890383266,56.6921958412561));
#10456=CARTESIAN_POINT('Ctrl Pts',(1.74397082505208,-2.90671134168276,56.6860920241775));
#10457=CARTESIAN_POINT('Ctrl Pts',(1.67849066294818,-2.94599817787158,56.6815940182456));
#10458=CARTESIAN_POINT('Ctrl Pts',(1.61175155109226,-2.98302976614351,56.6770960123138));
#10459=CARTESIAN_POINT('Ctrl Pts',(1.54392519925981,-3.01773094254451,56.6725980063819));
#10460=CARTESIAN_POINT('Ctrl Pts',(1.45186906274478,-3.06482851075654,56.6664931660518));
#10461=CARTESIAN_POINT('Ctrl Pts',(1.35750235757375,-3.10778852350133,56.6603883257217));
#10462=CARTESIAN_POINT('Ctrl Pts',(1.26123239426683,-3.14637853891612,56.6542834853916));
#10463=CARTESIAN_POINT('Ctrl Pts',(1.16508799032235,-3.18491822359883,56.6481866072527));
#10464=CARTESIAN_POINT('Ctrl Pts',(1.0670456566205,-3.21909908462528,56.6420897291139));
#10465=CARTESIAN_POINT('Ctrl Pts',(0.967536795021359,-3.24873477107316,
56.635992850975));
#10466=CARTESIAN_POINT('Ctrl Pts',(0.868129336742945,-3.27834025762759,
56.6299021857872));
#10467=CARTESIAN_POINT('Ctrl Pts',(0.767258729715019,-3.30340965881391,
56.6238115205995));
#10468=CARTESIAN_POINT('Ctrl Pts',(0.665375017554338,-3.32380522120574,
56.6177208554117));
#10469=CARTESIAN_POINT('Ctrl Pts',(0.563562716651571,-3.34418648815491,
56.6116344592288));
#10470=CARTESIAN_POINT('Ctrl Pts',(0.460739140447227,-3.35990034734694,
56.6055480630459));
#10471=CARTESIAN_POINT('Ctrl Pts',(0.357367314247439,-3.37085948464299,
56.599461666863));
#10472=CARTESIAN_POINT('Ctrl Pts',(0.254033018770817,-3.38181464305655,
56.5933774804393));
#10473=CARTESIAN_POINT('Ctrl Pts',(0.150151293299678,-3.38801846562094,
56.5872932940157));
#10474=CARTESIAN_POINT('Ctrl Pts',(0.0461923375375434,-3.38943525243555,
56.581209107592));
#10475=CARTESIAN_POINT('Ctrl Pts',(-0.0577557219079818,-3.39085189075157,
56.5751255588741));
#10476=CARTESIAN_POINT('Ctrl Pts',(-0.161780568384527,-3.38748248532737,
56.5690420101562));
#10477=CARTESIAN_POINT('Ctrl Pts',(-0.265410845296043,-3.37934344891123,
56.5629584614383));
#10478=CARTESIAN_POINT('Ctrl Pts',(-0.369057022577222,-3.37120316369317,
56.5568739792994));
#10479=CARTESIAN_POINT('Ctrl Pts',(-0.472308084088825,-3.35829182695691,
56.5507894971605));
#10480=CARTESIAN_POINT('Ctrl Pts',(-0.574697550708619,-3.3406777437684,
56.5447050150216));
#10481=CARTESIAN_POINT('Ctrl Pts',(-0.677192579494404,-3.3230455006965,
56.5386142598633));
#10482=CARTESIAN_POINT('Ctrl Pts',(-0.778823817675819,-3.30070090139576,
56.532523504705));
#10483=CARTESIAN_POINT('Ctrl Pts',(-0.879134786017541,-3.27376344449532,
56.5264327495467));
#10484=CARTESIAN_POINT('Ctrl Pts',(-0.979500035955152,-3.24681141084248,
56.5203386984785));
#10485=CARTESIAN_POINT('Ctrl Pts',(-1.07854318584358,-3.21526169858401,
56.5142446474103));
#10486=CARTESIAN_POINT('Ctrl Pts',(-1.175824621046,-3.17928317754837,56.5081505963421));
#10487=CARTESIAN_POINT('Ctrl Pts',(-1.273261952141,-3.14324700004786,56.5020467794072));
#10488=CARTESIAN_POINT('Ctrl Pts',(-1.3689315354293,-3.10276800306601,56.4959429624723));
#10489=CARTESIAN_POINT('Ctrl Pts',(-1.46241519191532,-3.05806260056188,
56.4898391455374));
#10490=CARTESIAN_POINT('Ctrl Pts',(-1.53130489936172,-3.02511842384106,
56.4853411383053));
#10491=CARTESIAN_POINT('Ctrl Pts',(-1.59900801369582,-2.9898801018946,56.4808431310733));
#10492=CARTESIAN_POINT('Ctrl Pts',(-1.66536712062625,-2.95244939262928,
56.4763451238412));
#10493=CARTESIAN_POINT('Ctrl Pts',(-1.75543184228785,-2.90164722594083,
56.470240283253));
#10494=CARTESIAN_POINT('Ctrl Pts',(-1.84332007246911,-2.84663542959565,
56.4641354426648));
#10495=CARTESIAN_POINT('Ctrl Pts',(-1.92861324830859,-2.78762551303947,
56.4580306020766));
#10496=CARTESIAN_POINT('Ctrl Pts',(-2.01379518123969,-2.72869255967145,
56.4519337236755));
#10497=CARTESIAN_POINT('Ctrl Pts',(-2.09638844032221,-2.66577209419138,
56.4458368452744));
#10498=CARTESIAN_POINT('Ctrl Pts',(-2.17599961693015,-2.59912114562208,
56.4397399668732));
#10499=CARTESIAN_POINT('Ctrl Pts',(-2.25552966676952,-2.53253811686392,
56.4336493014194));
#10500=CARTESIAN_POINT('Ctrl Pts',(-2.33208335126618,-2.46223243742888,
56.4275586359655));
#10501=CARTESIAN_POINT('Ctrl Pts',(-2.40529751288698,-2.38850349319395,
56.4214679705117));
#10502=CARTESIAN_POINT('Ctrl Pts',(-2.47846035806661,-2.3148262262158,56.4153815740581));
#10503=CARTESIAN_POINT('Ctrl Pts',(-2.54828803501001,-2.23773076824747,
56.4092951776045));
#10504=CARTESIAN_POINT('Ctrl Pts',(-2.61445229577363,-2.15755515702936,
56.4032087811509));
#10505=CARTESIAN_POINT('Ctrl Pts',(-2.68059253462078,-2.07740865475638,
56.3971245944538));
#10506=CARTESIAN_POINT('Ctrl Pts',(-2.74307172920056,-1.99418455104031,
56.3910404077568));
#10507=CARTESIAN_POINT('Ctrl Pts',(-2.80160072466742,-1.90825533984396,
56.3849562210597));
#10508=CARTESIAN_POINT('Ctrl Pts',(-2.86012358552046,-1.8223351351669,56.378872672066));
#10509=CARTESIAN_POINT('Ctrl Pts',(-2.91469683016211,-1.73371073995053,
56.3727891230723));
#10510=CARTESIAN_POINT('Ctrl Pts',(-2.9650741320207,-1.6427843602012,56.3667055740786));
#10511=CARTESIAN_POINT('Ctrl Pts',(-3.01545916346851,-1.55184402925683,
56.3606210916618));
#10512=CARTESIAN_POINT('Ctrl Pts',(-3.06164676598381,-1.45860138574944,
56.354536609245));
#10513=CARTESIAN_POINT('Ctrl Pts',(-3.10343658625327,-1.36348319300411,
56.3484521268283));
#10514=CARTESIAN_POINT('Ctrl Pts',(-3.14526949127501,-1.26826693465939,
56.3423613713906));
#10515=CARTESIAN_POINT('Ctrl Pts',(-3.18269538743489,-1.17117165741252,
56.3362706159529));
#10516=CARTESIAN_POINT('Ctrl Pts',(-3.21556213755194,-1.07264402391585,
56.3301798605151));
#10517=CARTESIAN_POINT('Ctrl Pts',(-3.24844667296481,-0.974063073827136,
56.3240858091663));
#10518=CARTESIAN_POINT('Ctrl Pts',(-3.27676703159179,-0.874048634611226,
56.3179917578175));
#10519=CARTESIAN_POINT('Ctrl Pts',(-3.30042155918176,-0.773060537207965,
56.3118977064687));
#10520=CARTESIAN_POINT('Ctrl Pts',(-3.32411399372917,-0.671910603915307,
56.3057938892539));
#10521=CARTESIAN_POINT('Ctrl Pts',(-3.34312558302879,-0.569784315802146,
56.2996900720391));
#10522=CARTESIAN_POINT('Ctrl Pts',(-3.35740615336754,-0.467149851578451,
56.2935862548243));
#10523=CARTESIAN_POINT('Ctrl Pts',(-3.36792974336041,-0.391516806468435,
56.2890882503164));
#10524=CARTESIAN_POINT('Ctrl Pts',(-3.37588525623752,-0.315607954960892,
56.2845902458085));
#10525=CARTESIAN_POINT('Ctrl Pts',(-3.3812707318465,-0.239610726926493,
56.2800922413006));
#10526=CARTESIAN_POINT('Ctrl Pts',(-3.38688785552139,-0.160344593382771,
56.2754007619502));
#10527=CARTESIAN_POINT('Ctrl Pts',(-3.38971799424802,-0.0808786711404675,
56.2707092825999));
#10528=CARTESIAN_POINT('Ctrl Pts',(-3.3897497300894,-0.00135272275167798,
56.2660178032496));
#10529=CARTESIAN_POINT('Ctrl Pts',(-3.3897497300897,-0.00135272198827972,
56.2660178032046));
#10530=CARTESIAN_POINT('Ctrl Pts',(-3.38976803835472,0.0445254680142906,
56.2633113082128));
#10531=CARTESIAN_POINT('Ctrl Pts',(-3.38885478857705,0.0904400107489448,
56.2606048132211));
#10532=CARTESIAN_POINT('Ctrl Pts',(-3.38700661857411,0.136349654327209,
56.2578983182294));
#10533=CARTESIAN_POINT('Origin',(0.,0.,0.));
#10534=CARTESIAN_POINT('',(-3.38700661857411,0.136349654327209,55.0079919592607));
#10535=CARTESIAN_POINT('',(-3.38700661431188,0.136349760203538,55.352502545304));
#10536=CARTESIAN_POINT('',(-3.38700661857411,0.136349654327212,0.));
#10537=CARTESIAN_POINT('Ctrl Pts',(-3.38700661431188,0.136349760203538,
55.352502545304));
#10538=CARTESIAN_POINT('Ctrl Pts',(-3.38880281242614,0.0917311639953066,
55.3553323773583));
#10539=CARTESIAN_POINT('Ctrl Pts',(-3.38971764573037,0.04706943732554,55.3581464239571));
#10540=CARTESIAN_POINT('Ctrl Pts',(-3.38981775511018,-0.0948718230840635,
55.3670241442622));
#10541=CARTESIAN_POINT('Ctrl Pts',(-3.38570021853797,-0.192098489435276,
55.3730055851047));
#10542=CARTESIAN_POINT('Ctrl Pts',(-3.37361926428369,-0.333272692528037,
55.3815389378329));
#10543=CARTESIAN_POINT('Ctrl Pts',(-3.36896296292172,-0.377447295195299,
55.3841876439945));
#10544=CARTESIAN_POINT('Ctrl Pts',(-3.35913793120111,-0.455844430543228,
55.3888523496557));
#10545=CARTESIAN_POINT('Ctrl Pts',(-3.35431085657523,-0.490102635728252,
55.3908784690254));
#10546=CARTESIAN_POINT('Ctrl Pts',(-3.34297290915396,-0.562526140321877,
55.3951379255789));
#10547=CARTESIAN_POINT('Ctrl Pts',(-3.3363309162693,-0.600666066013674,
55.3973669167801));
#10548=CARTESIAN_POINT('Ctrl Pts',(-3.31620064344492,-0.705591685659972,
55.4034655097463));
#10549=CARTESIAN_POINT('Ctrl Pts',(-3.3013497900379,-0.772098925274634,
55.4072930631311));
#10550=CARTESIAN_POINT('Ctrl Pts',(-3.24996096974156,-0.973487097817526,
55.4188137828708));
#10551=CARTESIAN_POINT('Ctrl Pts',(-3.20708058215176,-1.10659915118776,
55.4263266836567));
#10552=CARTESIAN_POINT('Ctrl Pts',(-3.06884593201819,-1.45938166653565,
55.4465108615667));
#10553=CARTESIAN_POINT('Ctrl Pts',(-2.95827328279954,-1.67218528840312,
55.4589658256642));
#10554=CARTESIAN_POINT('Ctrl Pts',(-2.80533079094595,-1.90314465635302,
55.474592369687));
#10555=CARTESIAN_POINT('Ctrl Pts',(-2.78388574653216,-1.93437853868915,
55.4767553418103));
#10556=CARTESIAN_POINT('Ctrl Pts',(-2.74942070224973,-1.98281513807268,
55.4801993479608));
#10557=CARTESIAN_POINT('Ctrl Pts',(-2.73675170902076,-2.00026500711701,
55.4814588430929));
#10558=CARTESIAN_POINT('Ctrl Pts',(-2.71183028863784,-2.03391099798975,
55.4839264865651));
#10559=CARTESIAN_POINT('Ctrl Pts',(-2.69959728825885,-2.0501199648902,55.4851334390427));
#10560=CARTESIAN_POINT('Ctrl Pts',(-2.66786323386809,-2.09139170281684,
55.4882515406727));
#10561=CARTESIAN_POINT('Ctrl Pts',(-2.64815451449506,-2.11629180375309,
55.4901758566423));
#10562=CARTESIAN_POINT('Ctrl Pts',(-2.5504389884697,-2.23624364747822,55.4996433378818));
#10563=CARTESIAN_POINT('Ctrl Pts',(-2.46765475187571,-2.32727299493945,
55.5074396122191));
#10564=CARTESIAN_POINT('Ctrl Pts',(-2.18047788780646,-2.61046643725383,
55.533283838457));
#10565=CARTESIAN_POINT('Ctrl Pts',(-1.95714454417599,-2.78184294702616,
55.551470872835));
#10566=CARTESIAN_POINT('Ctrl Pts',(-1.66255431199399,-2.95466559960069,
55.5723520284109));
#10567=CARTESIAN_POINT('Ctrl Pts',(-1.6090442926027,-2.98414356620845,55.5760391877437));
#10568=CARTESIAN_POINT('Ctrl Pts',(-1.52157296811918,-3.02929297571206,
55.5819012363272));
#10569=CARTESIAN_POINT('Ctrl Pts',(-1.48809988070516,-3.04587575920181,
55.5841067719575));
#10570=CARTESIAN_POINT('Ctrl Pts',(-1.42272979940289,-3.0769255844328,55.5883435730693));
#10571=CARTESIAN_POINT('Ctrl Pts',(-1.39086938580202,-3.09145817034851,
55.5903768468966));
#10572=CARTESIAN_POINT('Ctrl Pts',(-1.31453504042211,-3.12485775517422,
55.59517660708));
#10573=CARTESIAN_POINT('Ctrl Pts',(-1.26987119058267,-3.14327311089009,
55.5979279373855));
#10574=CARTESIAN_POINT('Ctrl Pts',(-1.09803808267832,-3.20986089594365,
55.6083151015919));
#10575=CARTESIAN_POINT('Ctrl Pts',(-0.968400955818843,-3.25132268966853,
55.6157378193699));
#10576=CARTESIAN_POINT('Ctrl Pts',(-0.697786346824847,-3.32024431414935,
55.6307362414596));
#10577=CARTESIAN_POINT('Ctrl Pts',(-0.556858385623788,-3.34676516665912,
55.6382836507556));
#10578=CARTESIAN_POINT('Ctrl Pts',(-0.278703994817397,-3.38104985318099,
55.6532280102531));
#10579=CARTESIAN_POINT('Ctrl Pts',(-0.141853269206001,-3.38954941346553,
55.6606053537901));
#10580=CARTESIAN_POINT('Ctrl Pts',(0.0343109744158353,-3.3898028743182,
55.6705286109024));
#10581=CARTESIAN_POINT('Ctrl Pts',(0.0734953391494766,-3.38917968422495,
55.672763226355));
#10582=CARTESIAN_POINT('Ctrl Pts',(0.134476779517066,-3.38715184635258,
55.6762954324407));
#10583=CARTESIAN_POINT('Ctrl Pts',(0.156287090053255,-3.38621557553222,
55.6775696230163));
#10584=CARTESIAN_POINT('Ctrl Pts',(0.198211625919492,-3.3840099538928,55.6800424057753));
#10585=CARTESIAN_POINT('Ctrl Pts',(0.218326150781844,-3.38277176774475,
55.6812394022601));
#10586=CARTESIAN_POINT('Ctrl Pts',(0.269280404435321,-3.37917885782386,
55.6842967597014));
#10587=CARTESIAN_POINT('Ctrl Pts',(0.300100799070864,-3.37658126702778,
55.6861693245666));
#10588=CARTESIAN_POINT('Ctrl Pts',(0.440105225867371,-3.36284958651597,
55.6947687799499));
#10589=CARTESIAN_POINT('Ctrl Pts',(0.548737075808639,-3.34683934463749,
55.7016976787149));
#10590=CARTESIAN_POINT('Ctrl Pts',(0.808585014055161,-3.29555164432306,
55.7186220205351));
#10591=CARTESIAN_POINT('Ctrl Pts',(0.958537651659366,-3.25510018163623,
55.7286744849725));
#10592=CARTESIAN_POINT('Ctrl Pts',(1.25736348858366,-3.15203930367955,55.7488581084028));
#10593=CARTESIAN_POINT('Ctrl Pts',(1.40561565967696,-3.08878139120974,55.7589506057311));
#10594=CARTESIAN_POINT('Ctrl Pts',(1.594071059493,-2.9919775640794,55.7717910396497));
#10595=CARTESIAN_POINT('Ctrl Pts',(1.63878865496302,-2.96772041259873,55.7748401040756));
#10596=CARTESIAN_POINT('Ctrl Pts',(1.7133985679064,-2.92504721228157,55.7799336968657));
#10597=CARTESIAN_POINT('Ctrl Pts',(1.74358044913255,-2.90715723699086,55.7819960444295));
#10598=CARTESIAN_POINT('Ctrl Pts',(1.8045874397261,-2.86970409864575,55.7861705128455));
#10599=CARTESIAN_POINT('Ctrl Pts',(1.83538517950259,-2.85010505656818,55.7882809955759));
#10600=CARTESIAN_POINT('Ctrl Pts',(1.91317657744602,-2.79881624116049,55.7936239139676));
#10601=CARTESIAN_POINT('Ctrl Pts',(1.9597038582622,-2.76643783023996,55.7968309384294));
#10602=CARTESIAN_POINT('Ctrl Pts',(2.13445581969581,-2.63820532358989,55.8089519765371));
#10603=CARTESIAN_POINT('Ctrl Pts',(2.25664964967774,-2.53447584893079,55.8175768828203));
#10604=CARTESIAN_POINT('Ctrl Pts',(2.54308768766548,-2.25411903199912,55.8389312186935));
#10605=CARTESIAN_POINT('Ctrl Pts',(2.69666924870136,-2.06792076541547,55.8514610143064));
#10606=CARTESIAN_POINT('Ctrl Pts',(2.84994352990845,-1.83565852459641,55.8671639727908));
#10607=CARTESIAN_POINT('Ctrl Pts',(2.87013951976179,-1.80391774631296,55.8693122946878));
#10608=CARTESIAN_POINT('Ctrl Pts',(2.90104523711558,-1.75351197349775,55.8727382585398));
#10609=CARTESIAN_POINT('Ctrl Pts',(2.91211316116165,-1.73506904523594,55.8739947342902));
#10610=CARTESIAN_POINT('Ctrl Pts',(2.93330578501534,-1.69898088908525,55.8764615298813));
#10611=CARTESIAN_POINT('Ctrl Pts',(2.94344847611743,-1.68134763994268,55.877670738164));
#10612=CARTESIAN_POINT('Ctrl Pts',(2.96910635766999,-1.63579723103008,55.8808023440801));
#10613=CARTESIAN_POINT('Ctrl Pts',(2.98438658993576,-1.6077504985349,55.882738123091));
#10614=CARTESIAN_POINT('Ctrl Pts',(3.05816346487137,-1.46765708426681,55.8924291476583));
#10615=CARTESIAN_POINT('Ctrl Pts',(3.11075323487543,-1.35262336918258,55.9004516674915));
#10616=CARTESIAN_POINT('Ctrl Pts',(3.26245885446327,-0.964826534104013,
55.9271509510384));
#10617=CARTESIAN_POINT('Ctrl Pts',(3.33304080208288,-0.682218090902137,
55.9459394379256));
#10618=CARTESIAN_POINT('Ctrl Pts',(3.37308522068366,-0.340079481245563,
55.9668837423022));
#10619=CARTESIAN_POINT('Ctrl Pts',(3.37810371588516,-0.28596109934416,55.9701496393307));
#10620=CARTESIAN_POINT('Ctrl Pts',(3.38428441609053,-0.195766326280985,
55.9755172405826));
#10621=CARTESIAN_POINT('Ctrl Pts',(3.38617557696697,-0.159751601037691,
55.9776406480183));
#10622=CARTESIAN_POINT('Ctrl Pts',(3.38880006037581,-0.0878880758427056,
55.9818401505056));
#10623=CARTESIAN_POINT('Ctrl Pts',(3.38954004312717,-0.0520442220928807,
55.9839161807035));
#10624=CARTESIAN_POINT('Ctrl Pts',(3.38996541981011,0.0369932491460334,
55.9890306157176));
#10625=CARTESIAN_POINT('Ctrl Pts',(3.38896766102692,0.0901813160466013,
55.99204805566));
#10626=CARTESIAN_POINT('Ctrl Pts',(3.38407446071835,0.205805093592326,55.9985396919981));
#10627=CARTESIAN_POINT('Ctrl Pts',(3.37970182287387,0.268201167569212,56.0019996490059));
#10628=CARTESIAN_POINT('Ctrl Pts',(3.36075269775636,0.46165923984409,56.012637151543));
#10629=CARTESIAN_POINT('Ctrl Pts',(3.34025515711655,0.592018612691681,56.0196716343036));
#10630=CARTESIAN_POINT('Ctrl Pts',(3.26610644093321,0.932719486350201,56.0381979578883));
#10631=CARTESIAN_POINT('Ctrl Pts',(3.19978173144393,1.13964588842961,56.0495836336144));
#10632=CARTESIAN_POINT('Ctrl Pts',(3.10001099804948,1.37172204303961,56.0638682740228));
#10633=CARTESIAN_POINT('Ctrl Pts',(3.08533521774873,1.40442014063747,56.065918459289));
#10634=CARTESIAN_POINT('Ctrl Pts',(3.06118341709256,1.45602474071922,56.0692235435943));
#10635=CARTESIAN_POINT('Ctrl Pts',(3.05204377953239,1.47508666695356,56.0704597045032));
#10636=CARTESIAN_POINT('Ctrl Pts',(3.03364057957295,1.51256565650118,56.072922975289));
#10637=CARTESIAN_POINT('Ctrl Pts',(3.02438616826005,1.53098604634607,56.074149563588));
#10638=CARTESIAN_POINT('Ctrl Pts',(2.99973962677736,1.5789480177251,56.0773829200129));
#10639=CARTESIAN_POINT('Ctrl Pts',(2.98407929569765,1.60834860898335,56.0794046962201));
#10640=CARTESIAN_POINT('Ctrl Pts',(2.88570846707277,1.78664559434733,56.0918888753432));
#10641=CARTESIAN_POINT('Ctrl Pts',(2.79231127632899,1.9293533093108,56.1028317612555));
#10642=CARTESIAN_POINT('Ctrl Pts',(2.54428152318409,2.25237380889502,56.1290482364958));
#10643=CARTESIAN_POINT('Ctrl Pts',(2.3806355117399,2.42469821129782,56.1442309296979));
#10644=CARTESIAN_POINT('Ctrl Pts',(2.15665389132087,2.61582603308636,56.1621803429106));
#10645=CARTESIAN_POINT('Ctrl Pts',(2.11203506676749,2.65198233670601,56.1656384560089));
#10646=CARTESIAN_POINT('Ctrl Pts',(2.03746995525649,2.70932907650006,56.1712315788607));
#10647=CARTESIAN_POINT('Ctrl Pts',(2.00806163105059,2.73119689977044,56.1733922464689));
#10648=CARTESIAN_POINT('Ctrl Pts',(1.9495621717022,2.7732409146765,56.1776044600269));
#10649=CARTESIAN_POINT('Ctrl Pts',(1.92049821387228,2.79344672040605,56.1796569491292));
#10650=CARTESIAN_POINT('Ctrl Pts',(1.84910307177839,2.84144089939737,56.1846054641413));
#10651=CARTESIAN_POINT('Ctrl Pts',(1.80645484846148,2.86874359420123,56.1874836230846));
#10652=CARTESIAN_POINT('Ctrl Pts',(1.62063315210809,2.98191572269229,56.199717988057));
#10653=CARTESIAN_POINT('Ctrl Pts',(1.47183097478437,3.05810310006835,56.2087373051968));
#10654=CARTESIAN_POINT('Ctrl Pts',(1.09951054676106,3.21523339141517,56.2302870631734));
#10655=CARTESIAN_POINT('Ctrl Pts',(0.871963317456202,3.28425123106222,56.2426242454246));
#10656=CARTESIAN_POINT('Ctrl Pts',(0.596626617109975,3.33711143644126,56.2583497419202));
#10657=CARTESIAN_POINT('Ctrl Pts',(0.553997151889645,3.34445254991414,56.2608076347832));
#10658=CARTESIAN_POINT('Ctrl Pts',(0.488858755129172,3.35439037750868,56.2646141438897));
#10659=CARTESIAN_POINT('Ctrl Pts',(0.466443546566341,3.35758068308,56.265933143475));
#10660=CARTESIAN_POINT('Ctrl Pts',(0.424352783082365,3.36314175720591,56.2684297835563));
#10661=CARTESIAN_POINT('Ctrl Pts',(0.404685716125779,3.3655649094346,56.2696046924258));
#10662=CARTESIAN_POINT('Ctrl Pts',(0.356269047383536,3.37109976620516,56.2725163626944));
#10663=CARTESIAN_POINT('Ctrl Pts',(0.327499133904528,3.37401622150589,56.2742630150445));
#10664=CARTESIAN_POINT('Ctrl Pts',(0.212666046209488,3.38417454836853,56.2812910947432));
#10665=CARTESIAN_POINT('Ctrl Pts',(0.126382319766553,3.38849369004091,56.2866973963907));
#10666=CARTESIAN_POINT('Ctrl Pts',(-0.140661911396912,3.3916478568469,56.3036415191862));
#10667=CARTESIAN_POINT('Ctrl Pts',(-0.321238670000045,3.37932941651606,
56.3153823977885));
#10668=CARTESIAN_POINT('Ctrl Pts',(-0.661177567651374,3.32863545646693,
56.3373372513491));
#10669=CARTESIAN_POINT('Ctrl Pts',(-0.820453630608091,3.29299820261443,
56.3475615430667));
#10670=CARTESIAN_POINT('Ctrl Pts',(-1.02532952170021,3.23136159150946,56.3605289390248));
#10671=CARTESIAN_POINT('Ctrl Pts',(-1.07375993274099,3.21559300717031,56.363581725251));
#10672=CARTESIAN_POINT('Ctrl Pts',(-1.15493389451528,3.18712476341028,56.3686796321921));
#10673=CARTESIAN_POINT('Ctrl Pts',(-1.1878676328728,3.17499719397437,56.3707426428394));
#10674=CARTESIAN_POINT('Ctrl Pts',(-1.25464724890001,3.14922159101854,56.3749169555051));
#10675=CARTESIAN_POINT('Ctrl Pts',(-1.28847299948785,3.13553405772326,56.3770266437697));
#10676=CARTESIAN_POINT('Ctrl Pts',(-1.37418542652807,3.09922933999873,56.382364404));
#10677=CARTESIAN_POINT('Ctrl Pts',(-1.42573962937739,3.07585355763925,56.3855671677636));
#10678=CARTESIAN_POINT('Ctrl Pts',(-1.53790080187587,3.02157096074304,56.3925357426453));
#10679=CARTESIAN_POINT('Ctrl Pts',(-1.59821183464366,2.99010862688449,56.3962831727273));
#10680=CARTESIAN_POINT('Ctrl Pts',(-1.79203410399074,2.88145665785104,56.4083901330433));
#10681=CARTESIAN_POINT('Ctrl Pts',(-1.92123351698479,2.79697035123722,56.4165542558339));
#10682=CARTESIAN_POINT('Ctrl Pts',(-2.18494660965102,2.59760080893612,56.4341125404148));
#10683=CARTESIAN_POINT('Ctrl Pts',(-2.31712704142991,2.48040959806604,56.4434885552329));
#10684=CARTESIAN_POINT('Ctrl Pts',(-2.46656255072167,2.3255074879639,56.4556168562031));
#10685=CARTESIAN_POINT('Ctrl Pts',(-2.49306499252338,2.29707260863191,56.457833941026));
#10686=CARTESIAN_POINT('Ctrl Pts',(-2.53363548422156,2.25201466146652,56.4613445710169));
#10687=CARTESIAN_POINT('Ctrl Pts',(-2.54804296401896,2.2357002930477,56.4626151774843));
#10688=CARTESIAN_POINT('Ctrl Pts',(-2.57550923013788,2.20398839499421,56.4650865620563));
#10689=CARTESIAN_POINT('Ctrl Pts',(-2.58858926817689,2.18861101273915,56.4662858404909));
#10690=CARTESIAN_POINT('Ctrl Pts',(-2.62148235162637,2.14923333011438,56.4693573025594));
#10691=CARTESIAN_POINT('Ctrl Pts',(-2.6411034158455,2.12507558089545,56.4712419134249));
#10692=CARTESIAN_POINT('Ctrl Pts',(-2.73013829121127,2.01231662123332,56.480026685157));
#10693=CARTESIAN_POINT('Ctrl Pts',(-2.79543984358782,1.92056896396365,56.4871392471992));
#10694=CARTESIAN_POINT('Ctrl Pts',(-3.01349154466822,1.57946741330266,56.5130253054));
#10695=CARTESIAN_POINT('Ctrl Pts',(-3.13844384182353,1.31379997801054,56.532040347514));
#10696=CARTESIAN_POINT('Ctrl Pts',(-3.24638103177779,0.977309656638154,
56.5536435438288));
#10697=CARTESIAN_POINT('Ctrl Pts',(-3.26343828280017,0.918746566271449,
56.5573247124549));
#10698=CARTESIAN_POINT('Ctrl Pts',(-3.2883759937193,0.823639586993963,56.5631797327621));
#10699=CARTESIAN_POINT('Ctrl Pts',(-3.29724799814706,0.787371989111304,
56.5653840963834));
#10700=CARTESIAN_POINT('Ctrl Pts',(-3.31327841594486,0.716810886868806,
56.5696201612203));
#10701=CARTESIAN_POINT('Ctrl Pts',(-3.32050793272171,0.682538578430042,
56.5716538443982));
#10702=CARTESIAN_POINT('Ctrl Pts',(-3.33382775125312,0.614163780496667,
56.5756664991972));
#10703=CARTESIAN_POINT('Ctrl Pts',(-3.3399290527832,0.580067814420547,56.5776455854605));
#10704=CARTESIAN_POINT('Ctrl Pts',(-3.35634839301707,0.479440074265641,
56.5834271050173));
#10705=CARTESIAN_POINT('Ctrl Pts',(-3.36520852940889,0.412685912169786,
56.5871861054862));
#10706=CARTESIAN_POINT('Ctrl Pts',(-3.37921317984871,0.276083387277213,
56.5947562725798));
#10707=CARTESIAN_POINT('Ctrl Pts',(-3.38419211761487,0.206263517159003,
56.5985610392712));
#10708=CARTESIAN_POINT('Ctrl Pts',(-3.3870066172248,0.136349687844955,56.6023307114865));
#10709=CARTESIAN_POINT('',(-3.38974984859561,-0.00101313674349031,55.0160178032937));
#10710=CARTESIAN_POINT('Ctrl Pts',(-3.38700661857411,0.136349654327209,
56.2578983182294));
#10711=CARTESIAN_POINT('Ctrl Pts',(-3.38288267634243,0.238790835438136,
56.2518591394859));
#10712=CARTESIAN_POINT('Ctrl Pts',(-3.37410030439886,0.341207785170065,
56.2458199607423));
#10713=CARTESIAN_POINT('Ctrl Pts',(-3.36065963653686,0.443138657591452,
56.2397807819988));
#10714=CARTESIAN_POINT('Ctrl Pts',(-3.34723386195637,0.544956582859223,
56.2337482951242));
#10715=CARTESIAN_POINT('Ctrl Pts',(-3.32916010725762,0.646289071186269,
56.2277158082497));
#10716=CARTESIAN_POINT('Ctrl Pts',(-3.3064905050191,0.746676370804987,56.2216833213752));
#10717=CARTESIAN_POINT('Ctrl Pts',(-3.28383903063338,0.846983395252976,
56.2156556584068));
#10718=CARTESIAN_POINT('Ctrl Pts',(-3.25659911068481,0.946346309143612,
56.2096279954385));
#10719=CARTESIAN_POINT('Ctrl Pts',(-3.22487430571405,1.04431354240254,56.2036003324701));
#10720=CARTESIAN_POINT('Ctrl Pts',(-3.19316270701911,1.14223999425065,56.1975751786734));
#10721=CARTESIAN_POINT('Ctrl Pts',(-3.15697006634594,1.23877150473748,56.1915500248766));
#10722=CARTESIAN_POINT('Ctrl Pts',(-3.11645011480498,1.3334705637666,56.1855248710799));
#10723=CARTESIAN_POINT('Ctrl Pts',(-3.07593603154595,1.42815590805135,56.1795005898731));
#10724=CARTESIAN_POINT('Ctrl Pts',(-3.03109605495282,1.52100892696445,56.1734763086662));
#10725=CARTESIAN_POINT('Ctrl Pts',(-2.98213209040148,1.61161200600446,56.1674520274594));
#10726=CARTESIAN_POINT('Ctrl Pts',(-2.93316192542893,1.702226558324,56.1614269833837));
#10727=CARTESIAN_POINT('Ctrl Pts',(-2.88006694368194,1.79059022110328,56.1554019393081));
#10728=CARTESIAN_POINT('Ctrl Pts',(-2.82309453404155,1.8763108256269,56.1493768952325));
#10729=CARTESIAN_POINT('Ctrl Pts',(-2.76606525586127,1.96211699447279,56.1433458370974));
#10730=CARTESIAN_POINT('Ctrl Pts',(-2.70515106505316,2.04527447374013,56.1373147789623));
#10731=CARTESIAN_POINT('Ctrl Pts',(-2.64064202260133,2.12542108086185,56.1312837208272));
#10732=CARTESIAN_POINT('Ctrl Pts',(-2.57609806547028,2.20561106629106,56.1252493984604));
#10733=CARTESIAN_POINT('Ctrl Pts',(-2.50795567258216,2.28278660859193,56.1192150760937));
#10734=CARTESIAN_POINT('Ctrl Pts',(-2.4365430563558,2.35662109746653,56.1131807537269));
#10735=CARTESIAN_POINT('Ctrl Pts',(-2.36501906131461,2.43057074243397,56.1071370199184));
#10736=CARTESIAN_POINT('Ctrl Pts',(-2.29021497689596,2.50116863066805,56.1010932861099));
#10737=CARTESIAN_POINT('Ctrl Pts',(-2.21249345498554,2.56812728931923,56.0950495523015));
#10738=CARTESIAN_POINT('Ctrl Pts',(-2.1644396452842,2.60952661554948,56.091312821121));
#10739=CARTESIAN_POINT('Ctrl Pts',(-2.11527120872906,2.64953558429001,56.0875760899405));
#10740=CARTESIAN_POINT('Ctrl Pts',(-2.06507922825687,2.68809464928637,56.08383935876));
#10741=CARTESIAN_POINT('Ctrl Pts',(-1.98307867243234,2.75109006672217,56.0777345182878));
#10742=CARTESIAN_POINT('Ctrl Pts',(-1.89805620863826,2.8104349818159,56.0716296778156));
#10743=CARTESIAN_POINT('Ctrl Pts',(-1.81037029782322,2.86582700930455,56.0655248373433));
#10744=CARTESIAN_POINT('Ctrl Pts',(-1.72279875064673,2.92114679219027,56.0594279590598));
#10745=CARTESIAN_POINT('Ctrl Pts',(-1.63257102091373,2.97252371094682,56.0533310807763));
#10746=CARTESIAN_POINT('Ctrl Pts',(-1.54007761224668,3.01969634413074,56.0472342024928));
#10747=CARTESIAN_POINT('Ctrl Pts',(-1.44767845784912,3.06682090662352,56.0411435371581));
#10748=CARTESIAN_POINT('Ctrl Pts',(-1.35301859437778,3.10974951017623,56.0350528718234));
#10749=CARTESIAN_POINT('Ctrl Pts',(-1.25651566281468,3.14826514950717,56.0289622064886));
#10750=CARTESIAN_POINT('Ctrl Pts',(-1.16008037102177,3.18675379288108,56.0228758101558));
#10751=CARTESIAN_POINT('Ctrl Pts',(-1.0618049757545,3.22083546515498,56.016789413823));
#10752=CARTESIAN_POINT('Ctrl Pts',(-0.962129022608679,3.25034041391884,
56.0107030174902));
#10753=CARTESIAN_POINT('Ctrl Pts',(-0.862489258313608,3.27983465046823,
56.004618830915));
#10754=CARTESIAN_POINT('Ctrl Pts',(-0.761450355998017,3.30475534496944,
55.9985346443398));
#10755=CARTESIAN_POINT('Ctrl Pts',(-0.659468267529887,3.32498220545932,
55.9924504577645));
#10756=CARTESIAN_POINT('Ctrl Pts',(-0.55749686814948,3.34520694590352,55.9863669088934));
#10757=CARTESIAN_POINT('Ctrl Pts',(-0.454582898256851,3.36073874762659,
55.9802833600223));
#10758=CARTESIAN_POINT('Ctrl Pts',(-0.351192888352274,3.37150835942472,
55.9741998111513));
#10759=CARTESIAN_POINT('Ctrl Pts',(-0.247787014920056,3.38227962364589,
55.9681153288578));
#10760=CARTESIAN_POINT('Ctrl Pts',(-0.143905381295408,3.38828720196697,
55.9620308465644));
#10761=CARTESIAN_POINT('Ctrl Pts',(-0.0400191221791434,3.38951376046182,
55.955946364271));
#10762=CARTESIAN_POINT('Ctrl Pts',(0.0639742422930276,3.39074158352222,
55.949855608957));
#10763=CARTESIAN_POINT('Ctrl Pts',(0.167971813812484,3.38717853820811,55.943764853643));
#10764=CARTESIAN_POINT('Ctrl Pts',(0.27150301771893,3.37885944867044,55.937674098329));
#10765=CARTESIAN_POINT('Ctrl Pts',(0.375090245811289,3.37053585739609,55.9315800471042));
#10766=CARTESIAN_POINT('Ctrl Pts',(0.478210179753243,3.35745114909732,55.9254859958795));
#10767=CARTESIAN_POINT('Ctrl Pts',(0.580399886191446,3.33969175742447,55.9193919446547));
#10768=CARTESIAN_POINT('Ctrl Pts',(0.682753354140988,3.32190390589082,55.9132881275634));
#10769=CARTESIAN_POINT('Ctrl Pts',(0.784173199516818,3.29942649913459,55.9071843104721));
#10770=CARTESIAN_POINT('Ctrl Pts',(0.884208956675721,3.272396611573,55.9010804933807));
#10771=CARTESIAN_POINT('Ctrl Pts',(0.95792699265596,3.25247783172469,55.8965824876602));
#10772=CARTESIAN_POINT('Ctrl Pts',(1.0308936847203,3.23008790258919,55.8920844819397));
#10773=CARTESIAN_POINT('Ctrl Pts',(1.10293578871009,3.20529838056965,55.8875864762192));
#10774=CARTESIAN_POINT('Ctrl Pts',(1.20071368887821,3.17165323037269,55.8814816357171));
#10775=CARTESIAN_POINT('Ctrl Pts',(1.29711374109057,3.13347380728671,55.875376795215));
#10776=CARTESIAN_POINT('Ctrl Pts',(1.39168599073097,3.09089229280206,55.8692719547129));
#10777=CARTESIAN_POINT('Ctrl Pts',(1.48613489528964,3.04836631490878,55.863175076399));
#10778=CARTESIAN_POINT('Ctrl Pts',(1.57876035039731,3.00144983409531,55.8570781980851));
#10779=CARTESIAN_POINT('Ctrl Pts',(1.66912889298272,2.95032435523796,55.8509813197712));
#10780=CARTESIAN_POINT('Ctrl Pts',(1.75940534662468,2.89925097516627,55.8448906544055));
#10781=CARTESIAN_POINT('Ctrl Pts',(1.84742909133248,2.84397733559493,55.8387999890399));
#10782=CARTESIAN_POINT('Ctrl Pts',(1.93278874106862,2.78473207775872,55.8327093236743));
#10783=CARTESIAN_POINT('Ctrl Pts',(2.0180885614691,2.72552834544925,55.8266229273101));
#10784=CARTESIAN_POINT('Ctrl Pts',(2.10072765029589,2.66235877362975,55.8205365309458));
#10785=CARTESIAN_POINT('Ctrl Pts',(2.18032195116577,2.59549634015629,55.8144501345816));
#10786=CARTESIAN_POINT('Ctrl Pts',(2.25988735413482,2.52865818208887,55.8083659479746));
#10787=CARTESIAN_POINT('Ctrl Pts',(2.33640983951913,2.45813010165325,55.8022817613675));
#10788=CARTESIAN_POINT('Ctrl Pts',(2.40953755496922,2.38422604500768,55.7961975747605));
#10789=CARTESIAN_POINT('Ctrl Pts',(2.48265760565956,2.31032973449277,55.7901140258573));
#10790=CARTESIAN_POINT('Ctrl Pts',(2.55238329355677,2.23305845513715,55.7840304769541));
#10791=CARTESIAN_POINT('Ctrl Pts',(2.61839950318521,2.15276313239972,55.777946928051));
#10792=CARTESIAN_POINT('Ctrl Pts',(2.68442584193768,2.07245548963835,55.7718624457252));
#10793=CARTESIAN_POINT('Ctrl Pts',(2.74674130029062,1.98912321165813,55.7657779633995));
#10794=CARTESIAN_POINT('Ctrl Pts',(2.8050715264326,1.90314970354333,55.7596934810737));
#10795=CARTESIAN_POINT('Ctrl Pts',(2.86346189026644,1.81708755787849,55.7536027257272));
#10796=CARTESIAN_POINT('Ctrl Pts',(2.91785857652049,1.72837909830563,55.7475119703806));
#10797=CARTESIAN_POINT('Ctrl Pts',(2.96803104666488,1.63743603494408,55.741421215034));
#10798=CARTESIAN_POINT('Ctrl Pts',(3.01823066680662,1.54644375925707,55.7353271637765));
#10799=CARTESIAN_POINT('Ctrl Pts',(3.06420132857478,1.45321485426518,55.7292331125191));
#10800=CARTESIAN_POINT('Ctrl Pts',(3.10575975542555,1.35818312612072,55.7231390612616));
#10801=CARTESIAN_POINT('Ctrl Pts',(3.14738478067409,1.26299910730234,55.7170352441376));
#10802=CARTESIAN_POINT('Ctrl Pts',(3.18458329376295,1.16600689329911,55.7109314270136));
#10803=CARTESIAN_POINT('Ctrl Pts',(3.2172211345348,1.0676578262733,55.7048276098895));
#10804=CARTESIAN_POINT('Ctrl Pts',(3.24127250782663,0.995182746182175,55.7003296044859));
#10805=CARTESIAN_POINT('Ctrl Pts',(3.26284826270117,0.921971182530229,55.6958315990823));
#10806=CARTESIAN_POINT('Ctrl Pts',(3.28191251605947,0.848207108807883,55.6913335936787));
#10807=CARTESIAN_POINT('Ctrl Pts',(3.30778714609861,0.74809208820494,55.6852287531929));
#10808=CARTESIAN_POINT('Ctrl Pts',(3.32911973321287,0.646625053760209,55.6791239127071));
#10809=CARTESIAN_POINT('Ctrl Pts',(3.34577231801947,0.544254222284597,55.6730190722213));
#10810=CARTESIAN_POINT('Ctrl Pts',(3.36240318382819,0.442016907130759,55.666922193924));
#10811=CARTESIAN_POINT('Ctrl Pts',(3.37436611445069,0.338878556663255,55.6608253156266));
#10812=CARTESIAN_POINT('Ctrl Pts',(3.3815733877642,0.235300840765542,55.6547284373292));
#10813=CARTESIAN_POINT('Ctrl Pts',(3.38877331659493,0.131828674458836,55.6486377719802));
#10814=CARTESIAN_POINT('Ctrl Pts',(3.39122719565924,0.027918457042437,55.6425471066313));
#10815=CARTESIAN_POINT('Ctrl Pts',(3.38889879706883,-0.0759605537462734,
55.6364564412824));
#10816=CARTESIAN_POINT('Ctrl Pts',(3.38657203047373,-0.17976675481124,55.630370044935));
#10817=CARTESIAN_POINT('Ctrl Pts',(3.37946966156913,-0.283541366856671,
55.6242836485877));
#10818=CARTESIAN_POINT('Ctrl Pts',(3.36760751900137,-0.386813469860425,
55.6181972522404));
#10819=CARTESIAN_POINT('Ctrl Pts',(3.35574968316203,-0.490048078381245,
55.6121130656503));
#10820=CARTESIAN_POINT('Ctrl Pts',(3.33913555703853,-0.592780116503111,
55.6060288790603));
#10821=CARTESIAN_POINT('Ctrl Pts',(3.31783290521502,-0.694542925651456,
55.5999446924703));
#10822=CARTESIAN_POINT('Ctrl Pts',(3.29653248619384,-0.796295068698662,
55.5938611435842));
#10823=CARTESIAN_POINT('Ctrl Pts',(3.2705446062986,-0.897077766664336,55.5877775946982));
#10824=CARTESIAN_POINT('Ctrl Pts',(3.23998813934696,-0.996434603670006,
55.5816940458121));
#10825=CARTESIAN_POINT('Ctrl Pts',(3.20942698399791,-1.09580668538112,55.5756095635035));
#10826=CARTESIAN_POINT('Ctrl Pts',(3.17429597448661,-1.19375206311132,55.5695250811949));
#10827=CARTESIAN_POINT('Ctrl Pts',(3.13476356205984,-1.28983040454236,55.5634405988864));
#10828=CARTESIAN_POINT('Ctrl Pts',(3.09519039223853,-1.38600780147312,55.557349843557));
#10829=CARTESIAN_POINT('Ctrl Pts',(3.05120692044458,-1.48031392231843,55.5512590882276));
#10830=CARTESIAN_POINT('Ctrl Pts',(3.0030293756567,-1.57232936480972,55.5451683328982));
#10831=CARTESIAN_POINT('Ctrl Pts',(2.9548257603921,-1.66439459992664,55.5390742816579));
#10832=CARTESIAN_POINT('Ctrl Pts',(2.90242376668504,-1.75416631857476,55.5329802304176));
#10833=CARTESIAN_POINT('Ctrl Pts',(2.84608412482369,-1.84125235014828,55.5268861791773));
#10834=CARTESIAN_POINT('Ctrl Pts',(2.78965419730395,-1.92847793922409,55.5207823620703));
#10835=CARTESIAN_POINT('Ctrl Pts',(2.72927426508139,-2.01300889616574,55.5146785449634));
#10836=CARTESIAN_POINT('Ctrl Pts',(2.66524677925035,-2.09448434422309,55.5085747278565));
#10837=CARTESIAN_POINT('Ctrl Pts',(2.61806384715454,-2.15452497338836,55.5040767222837));
#10838=CARTESIAN_POINT('Ctrl Pts',(2.5689009892064,-2.2129069919269,55.4995787167109));
#10839=CARTESIAN_POINT('Ctrl Pts',(2.51789186088322,-2.26949898422494,55.495080711138));
#10840=CARTESIAN_POINT('Ctrl Pts',(2.44866060121859,-2.34630748973206,55.4889758706512));
#10841=CARTESIAN_POINT('Ctrl Pts',(2.37579610082697,-2.42007335539983,55.4828710301644));
#10842=CARTESIAN_POINT('Ctrl Pts',(2.29959610820991,-2.49043425964346,55.4767661896776));
#10843=CARTESIAN_POINT('Ctrl Pts',(2.22349549881186,-2.56070339625146,55.4706693113792));
#10844=CARTESIAN_POINT('Ctrl Pts',(2.14406835733114,-2.62757611300103,55.4645724330808));
#10845=CARTESIAN_POINT('Ctrl Pts',(2.06165136586444,-2.69072456935475,55.4584755547824));
#10846=CARTESIAN_POINT('Ctrl Pts',(1.97931836041439,-2.7538086750544,55.4523848894325));
#10847=CARTESIAN_POINT('Ctrl Pts',(1.89400190108035,-2.81317580885546,55.4462942240826));
#10848=CARTESIAN_POINT('Ctrl Pts',(1.8060734048445,-2.86853689514592,55.4402035587327));
#10849=CARTESIAN_POINT('Ctrl Pts',(1.71820653847519,-2.92385917835768,55.4341171623844));
#10850=CARTESIAN_POINT('Ctrl Pts',(1.6277316364979,-2.97518077093345,55.4280307660361));
#10851=CARTESIAN_POINT('Ctrl Pts',(1.53505021852719,-3.02225509993773,55.4219443696878));
#10852=CARTESIAN_POINT('Ctrl Pts',(1.44240244993301,-3.06931233790202,55.4158601830968));
#10853=CARTESIAN_POINT('Ctrl Pts',(1.34755013807224,-3.11212518388724,55.4097759965059));
#10854=CARTESIAN_POINT('Ctrl Pts',(1.25091989776188,-3.15049273477712,55.4036918099149));
#10855=CARTESIAN_POINT('Ctrl Pts',(1.15429978559087,-3.18885626423539,55.3976082610279));
#10856=CARTESIAN_POINT('Ctrl Pts',(1.05590251261699,-3.2227752675427,55.3915247121409));
#10857=CARTESIAN_POINT('Ctrl Pts',(0.956174343943407,-3.25209712131793,
55.3854411632539));
#10858=CARTESIAN_POINT('Ctrl Pts',(0.85643087359044,-3.28142347405882,55.3793566809445));
#10859=CARTESIAN_POINT('Ctrl Pts',(0.755356511711694,-3.3061511553531,55.373272198635));
#10860=CARTESIAN_POINT('Ctrl Pts',(0.65341145691597,-3.32617776591555,55.3671877163256));
#10861=CARTESIAN_POINT('Ctrl Pts',(0.551361298117504,-3.34622502364853,
55.3610969609954));
#10862=CARTESIAN_POINT('Ctrl Pts',(0.448439073729685,-3.36156144925758,
55.3550062056651));
#10863=CARTESIAN_POINT('Ctrl Pts',(0.345113880702074,-3.37213603993771,
55.3489154503349));
#10864=CARTESIAN_POINT('Ctrl Pts',(0.241732774966303,-3.38271635288155,
55.3428213990938));
#10865=CARTESIAN_POINT('Ctrl Pts',(0.13794869279289,-3.38852967418034,55.3367273478528));
#10866=CARTESIAN_POINT('Ctrl Pts',(0.0342325659969947,-3.38957714087248,
55.3306332966117));
#10867=CARTESIAN_POINT('Ctrl Pts',(-0.0696497684363739,-3.39062628615569,
55.324529479504));
#10868=CARTESIAN_POINT('Ctrl Pts',(-0.173463502829106,-3.38689433600581,
55.3184256623963));
#10869=CARTESIAN_POINT('Ctrl Pts',(-0.276740792540085,-3.37843448896738,
55.3123218452886));
#10870=CARTESIAN_POINT('Ctrl Pts',(-0.352847565651834,-3.37220028529186,
55.3078238397249));
#10871=CARTESIAN_POINT('Ctrl Pts',(-0.428663108147057,-3.36339970668902,
55.3033258341611));
#10872=CARTESIAN_POINT('Ctrl Pts',(-0.5040040791703,-3.35207174008548,55.2988278285974));
#10873=CARTESIAN_POINT('Ctrl Pts',(-0.606259312987569,-3.3366970527409,
55.292722988105));
#10874=CARTESIAN_POINT('Ctrl Pts',(-0.707980940545628,-3.3166135056809,
55.2866181476127));
#10875=CARTESIAN_POINT('Ctrl Pts',(-0.808702506194882,-3.29186957806261,
55.2805133071204));
#10876=CARTESIAN_POINT('Ctrl Pts',(-0.90929270656509,-3.26715792250975,
55.2744164288164));
#10877=CARTESIAN_POINT('Ctrl Pts',(-1.00888502671304,-3.23779807174814,
55.2683195505124));
#10878=CARTESIAN_POINT('Ctrl Pts',(-1.1070202940763,-3.20388999982884,55.2622226722084));
#10879=CARTESIAN_POINT('Ctrl Pts',(-1.20505555790891,-3.17001648151091,
55.2561320068529));
#10880=CARTESIAN_POINT('Ctrl Pts',(-1.30163631988751,-3.13160409751842,
55.2500413414974));
#10881=CARTESIAN_POINT('Ctrl Pts',(-1.39631657981158,-3.08880317784143,
55.2439506761418));
#10882=CARTESIAN_POINT('Ctrl Pts',(-1.49093047749865,-3.04603225771003,
55.2378642797878));
#10883=CARTESIAN_POINT('Ctrl Pts',(-1.58364613397871,-2.99887909435195,
55.2317778834338));
#10884=CARTESIAN_POINT('Ctrl Pts',(-1.67403639432774,-2.94754257186663,
55.2256914870798));
#10885=CARTESIAN_POINT('Ctrl Pts',(-1.76439383714003,-2.89622468787408,
55.2196073004831));
#10886=CARTESIAN_POINT('Ctrl Pts',(-1.85242719075477,-2.84072667424631,
55.2135231138865));
#10887=CARTESIAN_POINT('Ctrl Pts',(-1.93773354946284,-2.7812935396657,55.2074389272898));
#10888=CARTESIAN_POINT('Ctrl Pts',(-2.02303096692565,-2.72186663447104,
55.201355378397));
#10889=CARTESIAN_POINT('Ctrl Pts',(-2.10560160738799,-2.65850567278295,
55.1952718295043));
#10890=CARTESIAN_POINT('Ctrl Pts',(-2.18507199485081,-2.59149868605383,
55.1891882806116));
#10891=CARTESIAN_POINT('Ctrl Pts',(-2.26455457576358,-2.5244814181827,55.1831037982964));
#10892=CARTESIAN_POINT('Ctrl Pts',(-2.34093563196606,-2.45381728921244,
55.1770193159811));
#10893=CARTESIAN_POINT('Ctrl Pts',(-2.41387589250341,-2.37983365765149,
55.1709348336659));
#10894=CARTESIAN_POINT('Ctrl Pts',(-2.48689135348432,-2.30577374994526,
55.1648440783299));
#10895=CARTESIAN_POINT('Ctrl Pts',(-2.55645863416792,-2.22838781000726,
55.1587533229939));
#10896=CARTESIAN_POINT('Ctrl Pts',(-2.62227642408051,-2.14803897036612,
55.1526625676579));
#10897=CARTESIAN_POINT('Ctrl Pts',(-2.68812983019447,-2.06764665128794,
55.146568516411));
#10898=CARTESIAN_POINT('Ctrl Pts',(-2.75022944869206,-1.98428858138369,
55.1404744651642));
#10899=CARTESIAN_POINT('Ctrl Pts',(-2.80831644606139,-1.89835818571762,
55.1343804139173));
#10900=CARTESIAN_POINT('Ctrl Pts',(-2.86649652926843,-1.8122900844853,55.1282765968039));
#10901=CARTESIAN_POINT('Ctrl Pts',(-2.92065092356286,-1.72364178784119,
55.1221727796905));
#10902=CARTESIAN_POINT('Ctrl Pts',(-2.97056592221792,-1.63283286476528,
55.1160689625771));
#10903=CARTESIAN_POINT('Ctrl Pts',(-3.00734912437631,-1.56591424180047,
55.1115709570703));
#10904=CARTESIAN_POINT('Ctrl Pts',(-3.04183109545327,-1.49782283125494,
55.1070729515635));
#10905=CARTESIAN_POINT('Ctrl Pts',(-3.07394321690758,-1.42873306174663,
55.1025749460567));
#10906=CARTESIAN_POINT('Ctrl Pts',(-3.12107749964318,-1.32732285953447,
55.0959727580448));
#10907=CARTESIAN_POINT('Ctrl Pts',(-3.16324201953652,-1.22346548226534,
55.0893705700329));
#10908=CARTESIAN_POINT('Ctrl Pts',(-3.20019768663299,-1.11764924236938,
55.082768382021));
#10909=CARTESIAN_POINT('Ctrl Pts',(-3.23702807947291,-1.01219170390749,
55.0761885744519));
#10910=CARTESIAN_POINT('Ctrl Pts',(-3.2686847197901,-0.904788838507579,
55.0696087668829));
#10911=CARTESIAN_POINT('Ctrl Pts',(-3.29497673585062,-0.795948096739492,
55.0630289593138));
#10912=CARTESIAN_POINT('Ctrl Pts',(-3.3212116362351,-0.687343796046599,
55.0564634454435));
#10913=CARTESIAN_POINT('Ctrl Pts',(-3.34210505503976,-0.577308145988027,
55.0498979315732));
#10914=CARTESIAN_POINT('Ctrl Pts',(-3.35751524924152,-0.466365107625599,
55.0433324177029));
#10915=CARTESIAN_POINT('Ctrl Pts',(-3.37287660872133,-0.355773646430945,
55.0367877098679));
#10916=CARTESIAN_POINT('Ctrl Pts',(-3.38278933482319,-0.244280839478064,
55.0302430020329));
#10917=CARTESIAN_POINT('Ctrl Pts',(-3.38716249140841,-0.132420992655877,
55.0236982941979));
#10918=CARTESIAN_POINT('Ctrl Pts',(-3.3888731860247,-0.0886635753286188,
55.0211381305631));
#10919=CARTESIAN_POINT('Ctrl Pts',(-3.3897367464864,-0.0448501340533459,
55.0185779669284));
#10920=CARTESIAN_POINT('Ctrl Pts',(-3.38974984859561,-0.00101313674349148,
55.0160178032937));
#10921=CARTESIAN_POINT('Ctrl Pts',(-3.38974984859583,-0.00101313598912749,
55.0160178032496));
#10922=CARTESIAN_POINT('Ctrl Pts',(-3.38976353983086,0.0447949908273649,
55.01334252192));
#10923=CARTESIAN_POINT('Ctrl Pts',(-3.38884852420672,0.0905956214387927,
55.0106672405903));
#10924=CARTESIAN_POINT('Ctrl Pts',(-3.38700661857411,0.136349654327207,
55.0079919592607));
#10925=CARTESIAN_POINT('Origin',(0.,0.,0.));
#10926=CARTESIAN_POINT('',(-3.38700661857411,0.136349654327214,53.7581562375148));
#10927=CARTESIAN_POINT('',(-3.38700661852469,0.136349655555037,54.0981108245895));
#10928=CARTESIAN_POINT('',(-3.38700661857411,0.136349654327212,0.));
#10929=CARTESIAN_POINT('',(-3.38974995993599,-0.000521165956363422,54.1059382181378));
#10930=CARTESIAN_POINT('Ctrl Pts',(-3.38700661852469,0.136349655555037,
54.0981108245895));
#10931=CARTESIAN_POINT('Ctrl Pts',(-3.38713784720114,0.133089857106149,
54.0982944673588));
#10932=CARTESIAN_POINT('Ctrl Pts',(-3.38726437466028,0.129829749115,54.0984783058417));
#10933=CARTESIAN_POINT('Ctrl Pts',(-3.38836760212715,0.10030397733956,54.1001449274906));
#10934=CARTESIAN_POINT('Ctrl Pts',(-3.38904345575389,0.0740288444827477,
54.1016399154169));
#10935=CARTESIAN_POINT('Ctrl Pts',(-3.38964034157982,0.0316597707542363,
54.1040734266578));
#10936=CARTESIAN_POINT('Ctrl Pts',(-3.38975243379317,0.0155692120963263,
54.105002909413));
#10937=CARTESIAN_POINT('Ctrl Pts',(-3.38974995993599,-0.000521165956363422,
54.1059382181378));
#10938=CARTESIAN_POINT('Ctrl Pts',(-3.38974995973272,-0.000522486388896574,
54.1059382948925));
#10939=CARTESIAN_POINT('Ctrl Pts',(-3.38974880577691,-0.00800903866730812,
54.1063734767157));
#10940=CARTESIAN_POINT('Ctrl Pts',(-3.38972284979861,-0.0154955041731149,
54.1068099170362));
#10941=CARTESIAN_POINT('Ctrl Pts',(-3.38959716225012,-0.0340336658808944,
54.1078939026009));
#10942=CARTESIAN_POINT('Ctrl Pts',(-3.38946818111483,-0.0450849686866558,
54.1085429784608));
#10943=CARTESIAN_POINT('Ctrl Pts',(-3.38895074179065,-0.076326456836172,
54.1103864888572));
#10944=CARTESIAN_POINT('Ctrl Pts',(-3.38843591336309,-0.0965135311733807,
54.1115879235587));
#10945=CARTESIAN_POINT('Ctrl Pts',(-3.38664827058089,-0.148410506838658,
54.1147008318373));
#10946=CARTESIAN_POINT('Ctrl Pts',(-3.3851104633099,-0.180108805124303,
54.1166254674601));
#10947=CARTESIAN_POINT('Ctrl Pts',(-3.37493640676949,-0.342636920141599,
54.1265977433721));
#10948=CARTESIAN_POINT('Ctrl Pts',(-3.3591601978656,-0.472898229193909,
54.1349325326575));
#10949=CARTESIAN_POINT('Ctrl Pts',(-3.31169581089374,-0.735955193926571,
54.1520851067243));
#10950=CARTESIAN_POINT('Ctrl Pts',(-3.27945019515363,-0.868427938849285,
54.1608925568338));
#10951=CARTESIAN_POINT('Ctrl Pts',(-3.1929216021003,-1.14911426306114,54.1796275628981));
#10952=CARTESIAN_POINT('Ctrl Pts',(-3.13608446160491,-1.29622403395978,
54.1894887486311));
#10953=CARTESIAN_POINT('Ctrl Pts',(-3.04797467126933,-1.4841695627637,54.202059048543));
#10954=CARTESIAN_POINT('Ctrl Pts',(-3.02573333417236,-1.52900198653648,
54.2050565907763));
#10955=CARTESIAN_POINT('Ctrl Pts',(-2.98612508286627,-1.60458958345322,
54.210111289979));
#10956=CARTESIAN_POINT('Ctrl Pts',(-2.96925586114434,-1.63559484956421,
54.2121849584143));
#10957=CARTESIAN_POINT('Ctrl Pts',(-2.93381192753878,-1.69838373641629,
54.2163870317253));
#10958=CARTESIAN_POINT('Ctrl Pts',(-2.91519755166542,-1.73013962724154,
54.2185136934568));
#10959=CARTESIAN_POINT('Ctrl Pts',(-2.86579346193715,-1.81136051545903,
54.2239609838004));
#10960=CARTESIAN_POINT('Ctrl Pts',(-2.83423855765408,-1.86034712754012,
54.2272540888061));
#10961=CARTESIAN_POINT('Ctrl Pts',(-2.67311869122726,-2.09685083209188,
54.2432357359045));
#10962=CARTESIAN_POINT('Ctrl Pts',(-2.52613379266629,-2.27178448441025,
54.2552704524063));
#10963=CARTESIAN_POINT('Ctrl Pts',(-2.23571499774619,-2.55408347108543,
54.2767917177553));
#10964=CARTESIAN_POINT('Ctrl Pts',(-2.09927092886332,-2.66736052272165,
54.2862324075508));
#10965=CARTESIAN_POINT('Ctrl Pts',(-1.92713688883577,-2.78884926911087,
54.2981790584023));
#10966=CARTESIAN_POINT('Ctrl Pts',(-1.89936510527903,-2.80783704134662,
54.3001078847219));
#10967=CARTESIAN_POINT('Ctrl Pts',(-1.85407155270942,-2.83782513331666,
54.303263683091));
#10968=CARTESIAN_POINT('Ctrl Pts',(-1.83672290795452,-2.84908436711678,
54.3044747676869));
#10969=CARTESIAN_POINT('Ctrl Pts',(-1.80369647837574,-2.87009143663667,
54.3067868111644));
#10970=CARTESIAN_POINT('Ctrl Pts',(-1.78803997479763,-2.87987132601829,
54.3078855384055));
#10971=CARTESIAN_POINT('Ctrl Pts',(-1.74448566013589,-2.9065856075163,54.3109477343445));
#10972=CARTESIAN_POINT('Ctrl Pts',(-1.7164226706873,-2.92324531258167,54.3129271508577));
#10973=CARTESIAN_POINT('Ctrl Pts',(-1.57046898984507,-3.00706511142262,
54.3232375389886));
#10974=CARTESIAN_POINT('Ctrl Pts',(-1.44887217252678,-3.06750331888508,
54.331874494367));
#10975=CARTESIAN_POINT('Ctrl Pts',(-1.08780944721153,-3.22069878443769,
54.3570592495246));
#10976=CARTESIAN_POINT('Ctrl Pts',(-0.840974019556434,-3.29378615324854,
54.3736484844233));
#10977=CARTESIAN_POINT('Ctrl Pts',(-0.523109897505935,-3.34979615622988,
54.3934548207542));
#10978=CARTESIAN_POINT('Ctrl Pts',(-0.457658201182087,-3.35936424404907,
54.3974587073065));
#10979=CARTESIAN_POINT('Ctrl Pts',(-0.353893554028891,-3.37144382832758,
54.4036916061082));
#10980=CARTESIAN_POINT('Ctrl Pts',(-0.31574864856133,-3.37522993364654,
54.4059586768766));
#10981=CARTESIAN_POINT('Ctrl Pts',(-0.24298056056052,-3.38120812435767,
54.410239568183));
#10982=CARTESIAN_POINT('Ctrl Pts',(-0.208372156989474,-3.38351726861837,
54.4122567031306));
#10983=CARTESIAN_POINT('Ctrl Pts',(-0.12865618115829,-3.38760829510363,
54.4168623881268));
#10984=CARTESIAN_POINT('Ctrl Pts',(-0.0835358145798179,-3.38902115837409,
54.419439438951));
#10985=CARTESIAN_POINT('Ctrl Pts',(0.0635201227786067,-3.39068711676852,
54.4277534010708));
#10986=CARTESIAN_POINT('Ctrl Pts',(0.165444568737296,-3.38724437886605,
54.433380786759));
#10987=CARTESIAN_POINT('Ctrl Pts',(0.322278966059611,-3.3748494623226,54.441927826291));
#10988=CARTESIAN_POINT('Ctrl Pts',(0.377378235597982,-3.36913320449526,
54.4449095825132));
#10989=CARTESIAN_POINT('Ctrl Pts',(0.682306715048204,-3.32992377976773,
54.4613681608745));
#10990=CARTESIAN_POINT('Ctrl Pts',(0.927907043754976,-3.26999979278323,
54.4744086677195));
#10991=CARTESIAN_POINT('Ctrl Pts',(1.20926823591909,-3.16707130870517,54.4911431835702));
#10992=CARTESIAN_POINT('Ctrl Pts',(1.25361457885408,-3.1497810030207,54.4938384630331));
#10993=CARTESIAN_POINT('Ctrl Pts',(1.31925672331664,-3.12258183566324,54.4979352529181));
#10994=CARTESIAN_POINT('Ctrl Pts',(1.34083904836122,-3.1133753710381,54.4992998354579));
#10995=CARTESIAN_POINT('Ctrl Pts',(1.38028847470216,-3.0960609982444,54.5018296021112));
#10996=CARTESIAN_POINT('Ctrl Pts',(1.39818347898119,-3.08802086634257,54.5029909856056));
#10997=CARTESIAN_POINT('Ctrl Pts',(1.44090391316207,-3.06837935004555,54.5057961115482));
#10998=CARTESIAN_POINT('Ctrl Pts',(1.46565982623667,-3.05663165774957,54.5074480160356));
#10999=CARTESIAN_POINT('Ctrl Pts',(1.53727271824638,-3.02157843891935,54.512297997835));
#11000=CARTESIAN_POINT('Ctrl Pts',(1.5837342098592,-2.99748712117677,54.5155345968511));
#11001=CARTESIAN_POINT('Ctrl Pts',(1.82279279452032,-2.86642034419381,54.5325941538459));
#11002=CARTESIAN_POINT('Ctrl Pts',(2.00517936774663,-2.74193245144112,54.5469688649951));
#11003=CARTESIAN_POINT('Ctrl Pts',(2.29869609373423,-2.4965447123013,54.5713981010247));
#11004=CARTESIAN_POINT('Ctrl Pts',(2.4155735618601,-2.38364323040263,54.5815715723823));
#11005=CARTESIAN_POINT('Ctrl Pts',(2.55753489657486,-2.22529896696241,54.5944540617795));
#11006=CARTESIAN_POINT('Ctrl Pts',(2.59030760254701,-2.18706359480978,54.5974710702015));
#11007=CARTESIAN_POINT('Ctrl Pts',(2.64461718845796,-2.12076740422357,54.6025483245134));
#11008=CARTESIAN_POINT('Ctrl Pts',(2.66658824507123,-2.09307470655296,54.6046254465186));
#11009=CARTESIAN_POINT('Ctrl Pts',(2.70783106859896,-2.03938778901376,54.6085715967526));
#11010=CARTESIAN_POINT('Ctrl Pts',(2.72717155828645,-2.01345152556354,54.6104431306776));
#11011=CARTESIAN_POINT('Ctrl Pts',(2.77760456368372,-1.94375894268725,54.6153832920784));
#11012=CARTESIAN_POINT('Ctrl Pts',(2.80803474200271,-1.89953343415626,54.6184271631954));
#11013=CARTESIAN_POINT('Ctrl Pts',(2.99791245774716,-1.60903468323097,54.6378859481037));
#11014=CARTESIAN_POINT('Ctrl Pts',(3.12585818965196,-1.34368354630474,54.6530925818413));
#11015=CARTESIAN_POINT('Ctrl Pts',(3.25723869027443,-0.946761436681349,
54.6755087321998));
#11016=CARTESIAN_POINT('Ctrl Pts',(3.28986257115198,-0.826292746792135,
54.6822935886086));
#11017=CARTESIAN_POINT('Ctrl Pts',(3.3223905741613,-0.673157060422188,54.691191787781));
#11018=CARTESIAN_POINT('Ctrl Pts',(3.32856880262191,-0.641910528181548,
54.6930215753848));
#11019=CARTESIAN_POINT('Ctrl Pts',(3.33796669455495,-0.590589980391987,
54.6960567635597));
#11020=CARTESIAN_POINT('Ctrl Pts',(3.34144785640518,-0.57056496634148,54.6972485036451));
#11021=CARTESIAN_POINT('Ctrl Pts',(3.3482461056926,-0.529260660227407,54.6997240012835));
#11022=CARTESIAN_POINT('Ctrl Pts',(3.3515408487459,-0.507979050074281,54.7010087569635));
#11023=CARTESIAN_POINT('Ctrl Pts',(3.36005180360068,-0.449312529690876,
54.7045732481889));
#11024=CARTESIAN_POINT('Ctrl Pts',(3.36484653321403,-0.411870642975198,
54.7068735996792));
#11025=CARTESIAN_POINT('Ctrl Pts',(3.39054340421553,-0.180613164224188,
54.721206785352));
#11026=CARTESIAN_POINT('Ctrl Pts',(3.39531774969034,0.0146151083274236,
54.7338252575582));
#11027=CARTESIAN_POINT('Ctrl Pts',(3.37009123008838,0.422675504427868,54.7601239349573));
#11028=CARTESIAN_POINT('Ctrl Pts',(3.33670690008856,0.634492524859602,54.773715686223));
#11029=CARTESIAN_POINT('Ctrl Pts',(3.27048444522901,0.892811715667228,54.7899055750597));
#11030=CARTESIAN_POINT('Ctrl Pts',(3.25621133986964,0.943540904387663,54.7930684490225));
#11031=CARTESIAN_POINT('Ctrl Pts',(3.23027614745665,1.02810489802438,54.7983155171613));
#11032=CARTESIAN_POINT('Ctrl Pts',(3.21925099286312,1.062123749796,54.8004193780254));
#11033=CARTESIAN_POINT('Ctrl Pts',(3.19599757127383,1.13018240403059,54.8046164028191));
#11034=CARTESIAN_POINT('Ctrl Pts',(3.18375870078436,1.16421364986842,54.8067089029626));
#11035=CARTESIAN_POINT('Ctrl Pts',(3.15158110395465,1.24938119740011,54.8119339696722));
#11036=CARTESIAN_POINT('Ctrl Pts',(3.13094039559436,1.30024210781025,54.8150434473145));
#11037=CARTESIAN_POINT('Ctrl Pts',(2.9945574572102,1.61419910488277,54.834215131494));
#11038=CARTESIAN_POINT('Ctrl Pts',(2.84698723680335,1.86217098632353,54.8491332806216));
#11039=CARTESIAN_POINT('Ctrl Pts',(2.59115729411746,2.18920982655896,54.871376049095));
#11040=CARTESIAN_POINT('Ctrl Pts',(2.50679787605289,2.28532146109677,54.8783190943877));
#11041=CARTESIAN_POINT('Ctrl Pts',(2.39478347763971,2.39925858605941,54.8873986450716));
#11042=CARTESIAN_POINT('Ctrl Pts',(2.37202145863168,2.42176458598733,54.88923719627));
#11043=CARTESIAN_POINT('Ctrl Pts',(2.33426889581641,2.45804966250731,54.8922829875356));
#11044=CARTESIAN_POINT('Ctrl Pts',(2.31946623613915,2.47202260882605,54.8934763735748));
#11045=CARTESIAN_POINT('Ctrl Pts',(2.28878032926301,2.50047023948265,54.8959506358887));
#11046=CARTESIAN_POINT('Ctrl Pts',(2.27288378142486,2.51492864232572,54.8972324407925));
#11047=CARTESIAN_POINT('Ctrl Pts',(2.22885656753686,2.55421439294252,54.9007799885008));
#11048=CARTESIAN_POINT('Ctrl Pts',(2.2004502217732,2.57872668885708,54.903066043987));
#11049=CARTESIAN_POINT('Ctrl Pts',(1.98638557325339,2.75733401771856,54.9202356966448));
#11050=CARTESIAN_POINT('Ctrl Pts',(1.78516251673025,2.89167877040181,54.9360034257713));
#11051=CARTESIAN_POINT('Ctrl Pts',(1.42983663024125,3.07757940838737,54.9616605820086));
#11052=CARTESIAN_POINT('Ctrl Pts',(1.28320970882871,3.14154597608366,54.9717181023114));
#11053=CARTESIAN_POINT('Ctrl Pts',(1.07922710513936,3.21385762159498,54.9849025248142));
#11054=CARTESIAN_POINT('Ctrl Pts',(1.02538427509494,3.23143924841082,54.9883113785962));
#11055=CARTESIAN_POINT('Ctrl Pts',(0.93616002117095,3.25811927970467,54.9938466638021));
#11056=CARTESIAN_POINT('Ctrl Pts',(0.901028839199804,3.26800918160687,54.995997719879));
#11057=CARTESIAN_POINT('Ctrl Pts',(0.831819202934741,3.28629168828837,55.0001819539615));
#11058=CARTESIAN_POINT('Ctrl Pts',(0.797756683395567,3.29472618808492,55.0022162225077));
#11059=CARTESIAN_POINT('Ctrl Pts',(0.713978129941297,3.31409579507144,55.0071617323388));
#11060=CARTESIAN_POINT('Ctrl Pts',(0.664134252535824,3.32444307863524,55.0100544643011));
#11061=CARTESIAN_POINT('Ctrl Pts',(0.454624170950834,3.36303567616586,55.0220305446317));
#11062=CARTESIAN_POINT('Ctrl Pts',(0.293264970952798,3.38093109274095,55.0307997891587));
#11063=CARTESIAN_POINT('Ctrl Pts',(-0.0228479750814905,3.39317831493441,
55.0476804168612));
#11064=CARTESIAN_POINT('Ctrl Pts',(-0.177150706255401,3.38862753910714,
55.0557859318033));
#11065=CARTESIAN_POINT('Ctrl Pts',(-0.439572508580142,3.36291084421065,
55.0699916897318));
#11066=CARTESIAN_POINT('Ctrl Pts',(-0.547951202497927,3.34695962480425,
55.0759863434842));
#11067=CARTESIAN_POINT('Ctrl Pts',(-0.685686008744834,3.31981855805869,
55.0839760542949));
#11068=CARTESIAN_POINT('Ctrl Pts',(-0.715929645054314,3.31342800755006,
55.085753798977));
#11069=CARTESIAN_POINT('Ctrl Pts',(-0.765735602672148,3.30219018829066,
55.088726369199));
#11070=CARTESIAN_POINT('Ctrl Pts',(-0.785350445078205,3.29758028193596,
55.08990867058));
#11071=CARTESIAN_POINT('Ctrl Pts',(-0.826135171697292,3.28761046747775,
55.0923932576763));
#11072=CARTESIAN_POINT('Ctrl Pts',(-0.847296154261183,3.28222044933866,
55.0936969774007));
#11073=CARTESIAN_POINT('Ctrl Pts',(-0.906312991594718,3.26657924185801,
55.097371074524));
#11074=CARTESIAN_POINT('Ctrl Pts',(-0.944044118462808,3.25587524376736,
55.0997640738037));
#11075=CARTESIAN_POINT('Ctrl Pts',(-1.11363388109118,3.20456848173543,55.1106941666996));
#11076=CARTESIAN_POINT('Ctrl Pts',(-1.24311688582502,3.15659537264405,55.1195142622557));
#11077=CARTESIAN_POINT('Ctrl Pts',(-1.53407295516866,3.02811280572796,55.1399669935222));
#11078=CARTESIAN_POINT('Ctrl Pts',(-1.69279058480409,2.94233164856218,55.1515927918168));
#11079=CARTESIAN_POINT('Ctrl Pts',(-1.93337539575698,2.78636383652742,55.1695807582493));
#11080=CARTESIAN_POINT('Ctrl Pts',(-2.02002687427742,2.72419875000878,55.1761488222825));
#11081=CARTESIAN_POINT('Ctrl Pts',(-2.13888236041718,2.63013506578544,55.1852783433681));
#11082=CARTESIAN_POINT('Ctrl Pts',(-2.17359480176549,2.60152150533854,55.1879607375157));
#11083=CARTESIAN_POINT('Ctrl Pts',(-2.23396281006884,2.54970791407216,55.1926568608095));
#11084=CARTESIAN_POINT('Ctrl Pts',(-2.25985153606307,2.52679074102485,55.1946814066929));
#11085=CARTESIAN_POINT('Ctrl Pts',(-2.31405445044402,2.47730980619854,55.1989452426932));
#11086=CARTESIAN_POINT('Ctrl Pts',(-2.34227217060202,2.45064749230435,55.2011800539229));
#11087=CARTESIAN_POINT('Ctrl Pts',(-2.4178215658101,2.3767652303288,55.207210801943));
#11088=CARTESIAN_POINT('Ctrl Pts',(-2.46422537632135,2.32861937312651,55.2109671265601));
#11089=CARTESIAN_POINT('Ctrl Pts',(-2.70227790250621,2.06653872232165,55.2305992917445));
#11090=CARTESIAN_POINT('Ctrl Pts',(-2.86756756174876,1.83028406060423,55.2454174956946));
#11091=CARTESIAN_POINT('Ctrl Pts',(-3.05059734322658,1.48175497423973,55.266649775665));
#11092=CARTESIAN_POINT('Ctrl Pts',(-3.09562848939659,1.38521565185532,55.2724870155394));
#11093=CARTESIAN_POINT('Ctrl Pts',(-3.14768948445942,1.25833143351853,55.2802951126124));
#11094=CARTESIAN_POINT('Ctrl Pts',(-3.15895349862581,1.22978036261847,55.2820607422084));
#11095=CARTESIAN_POINT('Ctrl Pts',(-3.17695326808241,1.18227636129799,55.2850188315253));
#11096=CARTESIAN_POINT('Ctrl Pts',(-3.18391108312619,1.16340863942326,55.2861990285575));
#11097=CARTESIAN_POINT('Ctrl Pts',(-3.19809913188291,1.12385372406835,55.2886862049741));
#11098=CARTESIAN_POINT('Ctrl Pts',(-3.20529727230949,1.10315664768894,55.2899947260406));
#11099=CARTESIAN_POINT('Ctrl Pts',(-3.22493723041621,1.04486969813699,55.2936967859319));
#11100=CARTESIAN_POINT('Ctrl Pts',(-3.23692146017324,1.00713057643775,55.296113470759));
#11101=CARTESIAN_POINT('Ctrl Pts',(-3.29631979681536,0.808057398542282,
55.3089336589346));
#11102=CARTESIAN_POINT('Ctrl Pts',(-3.33233827125783,0.643579686550158,
55.3197609200745));
#11103=CARTESIAN_POINT('Ctrl Pts',(-3.37207139070138,0.364103150086197,
55.3379338239378));
#11104=CARTESIAN_POINT('Ctrl Pts',(-3.38241663982499,0.250367371407375,
55.3452712400108));
#11105=CARTESIAN_POINT('Ctrl Pts',(-3.38700661431188,0.136349760203539,
55.352502545304));
#11106=CARTESIAN_POINT('',(-3.38974886845295,0.00276971513483697,53.766017803298));
#11107=CARTESIAN_POINT('Ctrl Pts',(-3.38700661857411,0.136349654327207,
55.0079919592607));
#11108=CARTESIAN_POINT('Ctrl Pts',(-3.38271306911003,0.243003980102895,
55.0017557805359));
#11109=CARTESIAN_POINT('Ctrl Pts',(-3.37337953946629,0.349404568150216,
54.9955196018111));
#11110=CARTESIAN_POINT('Ctrl Pts',(-3.35906611853581,0.455060296889049,
54.9892834230863));
#11111=CARTESIAN_POINT('Ctrl Pts',(-3.34474203433446,0.560794737464861,
54.9830425985075));
#11112=CARTESIAN_POINT('Ctrl Pts',(-3.32543072307948,0.665782821158282,
54.9768017739288));
#11113=CARTESIAN_POINT('Ctrl Pts',(-3.30124349820878,0.76954299947065,54.97056094935));
#11114=CARTESIAN_POINT('Ctrl Pts',(-3.27701548930977,0.873478136178295,
54.9643096016142));
#11115=CARTESIAN_POINT('Ctrl Pts',(-3.24789523580502,0.976180845668962,
54.9580582538784));
#11116=CARTESIAN_POINT('Ctrl Pts',(-3.21404426870813,1.07718359683223,54.9518069061426));
#11117=CARTESIAN_POINT('Ctrl Pts',(-3.18016135519291,1.17828166805332,54.9455496587772));
#11118=CARTESIAN_POINT('Ctrl Pts',(-3.14153897217313,1.27767621427922,54.9392924114117));
#11119=CARTESIAN_POINT('Ctrl Pts',(-3.09838652197303,1.37492036967814,54.9330351640462));
#11120=CARTESIAN_POINT('Ctrl Pts',(-3.05515295714101,1.47234731710473,54.926766154792));
#11121=CARTESIAN_POINT('Ctrl Pts',(-3.00737249175788,1.56761544493229,54.9204971455379));
#11122=CARTESIAN_POINT('Ctrl Pts',(-2.95530035426293,1.66030264668626,54.9142281362837));
#11123=CARTESIAN_POINT('Ctrl Pts',(-2.93341033988125,1.6992663665756,54.9115927786945));
#11124=CARTESIAN_POINT('Ctrl Pts',(-2.91076243068349,1.73777434941002,54.9089574211053));
#11125=CARTESIAN_POINT('Ctrl Pts',(-2.88737778668006,1.77579688576327,54.9063220635161));
#11126=CARTESIAN_POINT('Ctrl Pts',(-2.83320695155512,1.86387659086898,54.9002172230302));
#11127=CARTESIAN_POINT('Ctrl Pts',(-2.77491178083767,1.94962221129783,54.8941123825444));
#11128=CARTESIAN_POINT('Ctrl Pts',(-2.71271945693791,2.0326234797548,54.8880075420585));
#11129=CARTESIAN_POINT('Ctrl Pts',(-2.65060824686941,2.11551649448426,54.8819106637611));
#11130=CARTESIAN_POINT('Ctrl Pts',(-2.5846102429144,2.19567193422446,54.8758137854636));
#11131=CARTESIAN_POINT('Ctrl Pts',(-2.51499716353766,2.27270638884515,54.8697169071662));
#11132=CARTESIAN_POINT('Ctrl Pts',(-2.44545502250916,2.34966234245685,54.8636262418172));
#11133=CARTESIAN_POINT('Ctrl Pts',(-2.3723054167313,2.423503320107,54.8575355764682));
#11134=CARTESIAN_POINT('Ctrl Pts',(-2.29586124756975,2.49387774247406,54.8514449111193));
#11135=CARTESIAN_POINT('Ctrl Pts',(-2.21947065880728,2.56420283878162,54.8453585147719));
#11136=CARTESIAN_POINT('Ctrl Pts',(-2.13979041221341,2.63106592315446,54.8392721184245));
#11137=CARTESIAN_POINT('Ctrl Pts',(-2.05717071359343,2.69415176217553,54.8331857220772));
#11138=CARTESIAN_POINT('Ctrl Pts',(-1.97458101129209,2.75721469693816,54.8271015354871));
#11139=CARTESIAN_POINT('Ctrl Pts',(-1.88905431727527,2.8165028530403,54.8210173488971));
#11140=CARTESIAN_POINT('Ctrl Pts',(-1.80097379098454,2.87174136486676,54.814933162307));
#11141=CARTESIAN_POINT('Ctrl Pts',(-1.71290249670896,2.92697408695967,54.808849613421));
#11142=CARTESIAN_POINT('Ctrl Pts',(-1.62227826440829,2.97815778192843,54.8027660645349));
#11143=CARTESIAN_POINT('Ctrl Pts',(-1.52951232516102,3.02506150510705,54.7966825156489));
#11144=CARTESIAN_POINT('Ctrl Pts',(-1.4367321524759,3.07197242490583,54.7905980333403));
#11145=CARTESIAN_POINT('Ctrl Pts',(-1.3418100012344,3.11460187542676,54.7845135510318));
#11146=CARTESIAN_POINT('Ctrl Pts',(-1.24517990421265,3.15276578080976,54.7784290687232));
#11147=CARTESIAN_POINT('Ctrl Pts',(-1.1484501828388,3.1909690326745,54.7723383133939));
#11148=CARTESIAN_POINT('Ctrl Pts',(-1.05000939732259,3.22469738820762,54.7662475580645));
#11149=CARTESIAN_POINT('Ctrl Pts',(-0.950309642682163,3.25381570552564,
54.7601568027352));
#11150=CARTESIAN_POINT('Ctrl Pts',(-0.850555937178876,3.28294977973644,
54.7540627514949));
#11151=CARTESIAN_POINT('Ctrl Pts',(-0.749542320676296,3.30746874575644,
54.7479687002547));
#11152=CARTESIAN_POINT('Ctrl Pts',(-0.647732138507999,3.32728840638197,
54.7418746490145));
#11153=CARTESIAN_POINT('Ctrl Pts',(-0.545758803024913,3.34713982849992,
54.7357708319076));
#11154=CARTESIAN_POINT('Ctrl Pts',(-0.442986774797963,3.36227683979656,
54.7296670148008));
#11155=CARTESIAN_POINT('Ctrl Pts',(-0.339885794689353,3.3726670023986,54.7235631976939));
#11156=CARTESIAN_POINT('Ctrl Pts',(-0.263908946927662,3.38032368811976,
54.7190651921211));
#11157=CARTESIAN_POINT('Ctrl Pts',(-0.187753578591885,3.38540370428563,
54.7145671865483));
#11158=CARTESIAN_POINT('Ctrl Pts',(-0.111607059801464,3.38791217812718,
54.7100691809754));
#11159=CARTESIAN_POINT('Ctrl Pts',(-0.00825851019702291,3.39131676099405,
54.7039643404726));
#11160=CARTESIAN_POINT('Ctrl Pts',(0.0954183339104613,3.38999373153248,
54.6978594999697));
#11161=CARTESIAN_POINT('Ctrl Pts',(0.198955952643701,3.38390626220757,54.6917546594668));
#11162=CARTESIAN_POINT('Ctrl Pts',(0.302358533283741,3.3778267324148,54.6856577811523));
#11163=CARTESIAN_POINT('Ctrl Pts',(0.405621826601226,3.36699514171919,54.6795609028378));
#11164=CARTESIAN_POINT('Ctrl Pts',(0.508276146323263,3.35142662482394,54.6734640245232));
#11165=CARTESIAN_POINT('Ctrl Pts',(0.610825857430051,3.33587397283334,54.6673733591572));
#11166=CARTESIAN_POINT('Ctrl Pts',(0.7127674087945,3.31559405745615,54.6612826937911));
#11167=CARTESIAN_POINT('Ctrl Pts',(0.813634945909873,3.29065392244372,54.655192028425));
#11168=CARTESIAN_POINT('Ctrl Pts',(0.914431784070129,3.26573126819404,54.6491056320606));
#11169=CARTESIAN_POINT('Ctrl Pts',(1.01415569145816,3.23615499222817,54.6430192356961));
#11170=CARTESIAN_POINT('Ctrl Pts',(1.1123505508037,3.20204330305302,54.6369328393316));
#11171=CARTESIAN_POINT('Ctrl Pts',(1.21050975903522,3.16794399863741,54.6308486527245));
#11172=CARTESIAN_POINT('Ctrl Pts',(1.30714061946752,3.12931269383448,54.6247644661173));
#11173=CARTESIAN_POINT('Ctrl Pts',(1.40180250672691,3.0863173515752,54.6186802795102));
#11174=CARTESIAN_POINT('Ctrl Pts',(1.49645447215617,3.04332651580206,54.6125967306071));
#11175=CARTESIAN_POINT('Ctrl Pts',(1.58913748587239,2.99597272889506,54.606513181704));
#11176=CARTESIAN_POINT('Ctrl Pts',(1.67943207110619,2.9444715962359,54.6004296328009));
#11177=CARTESIAN_POINT('Ctrl Pts',(1.7697405105878,2.89296256155855,54.5943451504753));
#11178=CARTESIAN_POINT('Ctrl Pts',(1.85765942238197,2.83730512851825,54.5882606681498));
#11179=CARTESIAN_POINT('Ctrl Pts',(1.94279584416735,2.77775977550005,54.5821761858242));
#11180=CARTESIAN_POINT('Ctrl Pts',(2.02802004047452,2.71815303201257,54.576085430478));
#11181=CARTESIAN_POINT('Ctrl Pts',(2.11045566726323,2.65465060912955,54.5699946751318));
#11182=CARTESIAN_POINT('Ctrl Pts',(2.1897406136349,2.58755504434164,54.5639039197857));
#11183=CARTESIAN_POINT('Ctrl Pts',(2.26906846373453,2.52042317190655,54.5578098685287));
#11184=CARTESIAN_POINT('Ctrl Pts',(2.34524192418938,2.44969457519158,54.5517158172718));
#11185=CARTESIAN_POINT('Ctrl Pts',(2.41793517031265,2.37570927822938,54.5456217660148));
#11186=CARTESIAN_POINT('Ctrl Pts',(2.49074490914241,2.30160541801759,54.5395179488916));
#11187=CARTESIAN_POINT('Ctrl Pts',(2.56006300777758,2.22423475072808,54.5334141317683));
#11188=CARTESIAN_POINT('Ctrl Pts',(2.62560328529656,2.14397118701253,54.527310314645));
#11189=CARTESIAN_POINT('Ctrl Pts',(2.67390101710397,2.08482361820466,54.5228123092416));
#11190=CARTESIAN_POINT('Ctrl Pts',(2.72014806194289,2.0241057699486,54.5183143038382));
#11191=CARTESIAN_POINT('Ctrl Pts',(2.76424533668976,1.96197675345273,54.5138162984348));
#11192=CARTESIAN_POINT('Ctrl Pts',(2.82409560438845,1.87765321440233,54.5077114579645));
#11193=CARTESIAN_POINT('Ctrl Pts',(2.88018373319809,1.79044793869892,54.5016066174942));
#11194=CARTESIAN_POINT('Ctrl Pts',(2.93222110601276,1.70073056300913,54.4955017770239));
#11195=CARTESIAN_POINT('Ctrl Pts',(2.98419060950876,1.61113020047412,54.4894048987419));
#11196=CARTESIAN_POINT('Ctrl Pts',(3.03211964795986,1.51902461827581,54.48330802046));
#11197=CARTESIAN_POINT('Ctrl Pts',(3.07576175020044,1.42481392416833,54.477211142178));
#11198=CARTESIAN_POINT('Ctrl Pts',(3.1193593794969,1.33069923430259,54.4711204768444));
#11199=CARTESIAN_POINT('Ctrl Pts',(3.15867858115272,1.23448408403791,54.4650298115108));
#11200=CARTESIAN_POINT('Ctrl Pts',(3.19351829436629,1.13659401988918,54.4589391461772));
#11201=CARTESIAN_POINT('Ctrl Pts',(3.22833358811568,1.03877256775513,54.452852749845));
#11202=CARTESIAN_POINT('Ctrl Pts',(3.25867549433964,0.93927893765865,54.4467663535128));
#11203=CARTESIAN_POINT('Ctrl Pts',(3.28439099945326,0.838558778625809,54.4406799571806));
#11204=CARTESIAN_POINT('Ctrl Pts',(3.31009716816831,0.737875187552442,54.4345957706055));
#11205=CARTESIAN_POINT('Ctrl Pts',(3.33118016863909,0.635966366107156,54.4285115840305));
#11206=CARTESIAN_POINT('Ctrl Pts',(3.34753703262397,0.533292487956728,54.4224273974555));
#11207=CARTESIAN_POINT('Ctrl Pts',(3.36389218219153,0.430629371397037,54.4163438485843));
#11208=CARTESIAN_POINT('Ctrl Pts',(3.37552211319775,0.327201779484954,54.4102602997131));
#11209=CARTESIAN_POINT('Ctrl Pts',(3.38237526160712,0.223478527308951,54.4041767508419));
#11210=CARTESIAN_POINT('Ctrl Pts',(3.38922946152187,0.119739360468459,54.3980922685479));
#11211=CARTESIAN_POINT('Ctrl Pts',(3.3913053945124,0.015704869540343,54.392007786254));
#11212=CARTESIAN_POINT('Ctrl Pts',(3.38860355077158,-0.0881534922635265,
54.3859233039601));
#11213=CARTESIAN_POINT('Ctrl Pts',(3.38589892146543,-0.192118930670961,
54.3798325486451));
#11214=CARTESIAN_POINT('Ctrl Pts',(3.37840668973926,-0.295907449474564,
54.37374179333));
#11215=CARTESIAN_POINT('Ctrl Pts',(3.36617944540213,-0.399050126991812,
54.367651038015));
#11216=CARTESIAN_POINT('Ctrl Pts',(3.35394558449486,-0.502248618455593,
54.3615569867889));
#11217=CARTESIAN_POINT('Ctrl Pts',(3.33697167683054,-0.604800150975558,
54.3554629355627));
#11218=CARTESIAN_POINT('Ctrl Pts',(3.31536159593447,-0.706245389863055,
54.3493688843366));
#11219=CARTESIAN_POINT('Ctrl Pts',(3.29371688435196,-0.807853197242361,
54.3432650672435));
#11220=CARTESIAN_POINT('Ctrl Pts',(3.26742126667447,-0.90835075610087,54.3371612501503));
#11221=CARTESIAN_POINT('Ctrl Pts',(3.23662874963644,-1.00729310507264,54.3310574330571));
#11222=CARTESIAN_POINT('Ctrl Pts',(3.21393722469607,-1.08020539011184,54.3265594273362));
#11223=CARTESIAN_POINT('Ctrl Pts',(3.18880472242233,-1.15227344406592,54.3220614216151));
#11224=CARTESIAN_POINT('Ctrl Pts',(3.16130929773415,-1.22332685189184,54.3175634158941));
#11225=CARTESIAN_POINT('Ctrl Pts',(3.12399160808946,-1.31976286084666,54.3114585754191));
#11226=CARTESIAN_POINT('Ctrl Pts',(3.08219497809912,-1.41465058412122,54.3053537349439));
#11227=CARTESIAN_POINT('Ctrl Pts',(3.03606850574177,-1.50754538603087,54.2992488944689));
#11228=CARTESIAN_POINT('Ctrl Pts',(2.99000219346137,-1.60031903064957,54.2931520161824));
#11229=CARTESIAN_POINT('Ctrl Pts',(2.93961745443416,-1.69110454202663,54.2870551378959));
#11230=CARTESIAN_POINT('Ctrl Pts',(2.8851120512839,-1.77947562895265,54.2809582596094));
#11231=CARTESIAN_POINT('Ctrl Pts',(2.83066219119295,-1.86775666241169,54.2748675942716));
#11232=CARTESIAN_POINT('Ctrl Pts',(2.77210024035554,-1.95362780237237,54.2687769289338));
#11233=CARTESIAN_POINT('Ctrl Pts',(2.70967022941156,-2.03668660091353,54.262686263596));
#11234=CARTESIAN_POINT('Ctrl Pts',(2.64728397622073,-2.11968718279976,54.25659986726));
#11235=CARTESIAN_POINT('Ctrl Pts',(2.5810353103908,-2.19987900273196,54.250513470924));
#11236=CARTESIAN_POINT('Ctrl Pts',(2.51121153426146,-2.27688859909575,54.244427074588));
#11237=CARTESIAN_POINT('Ctrl Pts',(2.44141310870103,-2.35387023597084,54.2383428880095));
#11238=CARTESIAN_POINT('Ctrl Pts',(2.36804243931463,-2.4276716294355,54.2322587014309));
#11239=CARTESIAN_POINT('Ctrl Pts',(2.29142654994989,-2.49795304773424,54.2261745148524));
#11240=CARTESIAN_POINT('Ctrl Pts',(2.21481869095487,-2.56822709960051,54.220090965978));
#11241=CARTESIAN_POINT('Ctrl Pts',(2.13496660323843,-2.63498162123575,54.2140074171035));
#11242=CARTESIAN_POINT('Ctrl Pts',(2.05223287463767,-2.69791498953477,54.2079238682291));
#11243=CARTESIAN_POINT('Ctrl Pts',(1.96948645188116,-2.76085801394373,54.2018393859323));
#11244=CARTESIAN_POINT('Ctrl Pts',(1.88385784983554,-2.81997846151331,54.1957549036354));
#11245=CARTESIAN_POINT('Ctrl Pts',(1.79574057163204,-2.87501667158551,54.1896704213386));
#11246=CARTESIAN_POINT('Ctrl Pts',(1.70753244568139,-2.93011162532359,54.183579666021));
#11247=CARTESIAN_POINT('Ctrl Pts',(1.61683088271967,-2.98111571003608,54.1774889107035));
#11248=CARTESIAN_POINT('Ctrl Pts',(1.52405601427245,-3.02781411712476,54.171398155386));
#11249=CARTESIAN_POINT('Ctrl Pts',(1.43123094225041,-3.07453779427863,54.1653041041577));
#11250=CARTESIAN_POINT('Ctrl Pts',(1.3363307199609,-3.1169509783585,54.1592100529293));
#11251=CARTESIAN_POINT('Ctrl Pts',(1.23979577237874,-3.15488692432737,54.153116001701));
#11252=CARTESIAN_POINT('Ctrl Pts',(1.14310612517395,-3.19288366358066,54.147012184606));
#11253=CARTESIAN_POINT('Ctrl Pts',(1.04477692425027,-3.22638869459226,54.1409083675111));
#11254=CARTESIAN_POINT('Ctrl Pts',(0.945264261161252,-3.2552850165648,54.1348045504161));
#11255=CARTESIAN_POINT('Ctrl Pts',(0.871931702601138,-3.27657920322853,
54.1303065447286));
#11256=CARTESIAN_POINT('Ctrl Pts',(0.797956780170471,-3.29537169747829,
54.125808539041));
#11257=CARTESIAN_POINT('Ctrl Pts',(0.723524692469719,-3.3116335971672,54.1213105333535));
#11258=CARTESIAN_POINT('Ctrl Pts',(0.622503025979026,-3.33370477987382,
54.1152056927601));
#11259=CARTESIAN_POINT('Ctrl Pts',(0.520302028742421,-3.35118605235059,
54.1091008521669));
#11260=CARTESIAN_POINT('Ctrl Pts',(0.417374812849767,-3.36395649913887,
54.1029960115735));
#11261=CARTESIAN_POINT('Ctrl Pts',(0.314581838931188,-3.37671029017705,
54.0968991331683));
#11262=CARTESIAN_POINT('Ctrl Pts',(0.21106494988949,-3.38476541843064,54.0908022547631));
#11263=CARTESIAN_POINT('Ctrl Pts',(0.107288801997741,-3.38805167839363,
54.0847053763579));
#11264=CARTESIAN_POINT('Ctrl Pts',(0.00361840590228503,-3.39133458953417,
54.078614710901));
#11265=CARTESIAN_POINT('Ctrl Pts',(-0.100310298885308,-3.38985828274735,
54.072524045444));
#11266=CARTESIAN_POINT('Ctrl Pts',(-0.204027020455333,-3.38360429681488,
54.0664333799871));
#11267=CARTESIAN_POINT('Ctrl Pts',(-0.307671046049174,-3.37735469435699,
54.060346983532));
#11268=CARTESIAN_POINT('Ctrl Pts',(-0.411102958675252,-3.36633409778358,
54.0542605870769));
#11269=CARTESIAN_POINT('Ctrl Pts',(-0.513852773378347,-3.35057612803998,
54.0481741906218));
#11270=CARTESIAN_POINT('Ctrl Pts',(-0.616565283220748,-3.33482387946354,
54.0420900039242));
#11271=CARTESIAN_POINT('Ctrl Pts',(-0.718595765519508,-3.31433774092562,
54.0360058172266));
#11272=CARTESIAN_POINT('Ctrl Pts',(-0.819480457211773,-3.28920307107177,
54.0299216305289));
#11273=CARTESIAN_POINT('Ctrl Pts',(-0.920354574836653,-3.26407103566809,
54.0238380815356));
#11274=CARTESIAN_POINT('Ctrl Pts',(-1.02008272615848,-3.23429154118383,
54.0177545325423));
#11275=CARTESIAN_POINT('Ctrl Pts',(-1.11821331572462,-3.20000063172434,
54.0116709835489));
#11276=CARTESIAN_POINT('Ctrl Pts',(-1.21635896184113,-3.16570446087991,
54.0055865011335));
#11277=CARTESIAN_POINT('Ctrl Pts',(-1.31290615587972,-3.12689564073215,
53.999502018718));
#11278=CARTESIAN_POINT('Ctrl Pts',(-1.40742124877484,-3.08375914931712,
53.9934175363026));
#11279=CARTESIAN_POINT('Ctrl Pts',(-1.50203378545856,-3.04057818476007,
53.9873267808677));
#11280=CARTESIAN_POINT('Ctrl Pts',(-1.59460964780646,-2.99306081653175,
53.9812360254328));
#11281=CARTESIAN_POINT('Ctrl Pts',(-1.68473790812533,-2.941438974962,53.9751452699978));
#11282=CARTESIAN_POINT('Ctrl Pts',(-1.77491493984307,-2.88978919909709,
53.9690512186526));
#11283=CARTESIAN_POINT('Ctrl Pts',(-1.86264137067453,-2.83403075481871,
53.9629571673074));
#11284=CARTESIAN_POINT('Ctrl Pts',(-1.94753516753801,-2.77443901243165,
53.9568631159621));
#11285=CARTESIAN_POINT('Ctrl Pts',(-2.03256500876364,-2.71475177283652,
53.9507592987523));
#11286=CARTESIAN_POINT('Ctrl Pts',(-2.11475281020638,-2.65121922559731,
53.9446554815424));
#11287=CARTESIAN_POINT('Ctrl Pts',(-2.19374938756521,-2.58415724890287,
53.9385516643325));
#11288=CARTESIAN_POINT('Ctrl Pts',(-2.25196328040394,-2.534738161958,53.934053659826));
#11289=CARTESIAN_POINT('Ctrl Pts',(-2.30844489606716,-2.48340327098839,
53.9295556553194));
#11290=CARTESIAN_POINT('Ctrl Pts',(-2.36306796596053,-2.43029110411719,
53.9250576508129));
#11291=CARTESIAN_POINT('Ctrl Pts',(-2.43614074560596,-2.35923955623008,
53.9190403820509));
#11292=CARTESIAN_POINT('Ctrl Pts',(-2.50614531578541,-2.28475379901223,
53.913023113289));
#11293=CARTESIAN_POINT('Ctrl Pts',(-2.57273549547598,-2.20713323857396,
53.907005844527));
#11294=CARTESIAN_POINT('Ctrl Pts',(-2.63922143882549,-2.12963418078441,
53.9009979948428));
#11295=CARTESIAN_POINT('Ctrl Pts',(-2.70230333681151,-2.04901041047589,
53.8949901451586));
#11296=CARTESIAN_POINT('Ctrl Pts',(-2.76167070345194,-1.96559914229613,
53.8889822954743));
#11297=CARTESIAN_POINT('Ctrl Pts',(-2.82098532482678,-1.8822619813194,53.8829797834974));
#11298=CARTESIAN_POINT('Ctrl Pts',(-2.87659171419398,-1.7961425973199,53.8769772715205));
#11299=CARTESIAN_POINT('Ctrl Pts',(-2.92821901061884,-1.70761192557046,
53.8709747595436));
#11300=CARTESIAN_POINT('Ctrl Pts',(-2.97981472197077,-1.61913541601653,
53.8649759198446));
#11301=CARTESIAN_POINT('Ctrl Pts',(-3.0274359546713,-1.5282509288324,53.8589770801455));
#11302=CARTESIAN_POINT('Ctrl Pts',(-3.0708552501005,-1.43535817670371,53.8529782404465));
#11303=CARTESIAN_POINT('Ctrl Pts',(-3.11425999142334,-1.34249656213682,
53.8469814115528));
#11304=CARTESIAN_POINT('Ctrl Pts',(-3.15346540869544,-1.24762841971144,
53.8409845826591));
#11305=CARTESIAN_POINT('Ctrl Pts',(-3.18829058916242,-1.15117686806083,
53.8349877537654));
#11306=CARTESIAN_POINT('Ctrl Pts',(-3.22312809554013,-1.05469117866279,
53.8289888023737));
#11307=CARTESIAN_POINT('Ctrl Pts',(-3.25358211035393,-0.956621372797933,
53.8229898509819));
#11308=CARTESIAN_POINT('Ctrl Pts',(-3.27952057482157,-0.857408806708909,
53.8169908995902));
#11309=CARTESIAN_POINT('Ctrl Pts',(-3.30546295820986,-0.758181251059746,
53.8109910418451));
#11310=CARTESIAN_POINT('Ctrl Pts',(-3.3268883330814,-0.657811021334741,
53.8049911841));
#11311=CARTESIAN_POINT('Ctrl Pts',(-3.34371548730905,-0.556751113541406,
53.7989913263549));
#11312=CARTESIAN_POINT('Ctrl Pts',(-3.36056098266848,-0.455581053249218,
53.7929849289311));
#11313=CARTESIAN_POINT('Ctrl Pts',(-3.3727981863967,-0.353720250879779,
53.7869785315074));
#11314=CARTESIAN_POINT('Ctrl Pts',(-3.38039766334347,-0.251628098911874,
53.7809721340836));
#11315=CARTESIAN_POINT('Ctrl Pts',(-3.38670455492597,-0.166900671169774,
53.7759873571551));
#11316=CARTESIAN_POINT('Ctrl Pts',(-3.3898181440983,-0.082014108835823,
53.7710025802265));
#11317=CARTESIAN_POINT('Ctrl Pts',(-3.38974886845295,0.00276971513482787,
53.766017803298));
#11318=CARTESIAN_POINT('Ctrl Pts',(-3.38974886845228,0.00276971595823088,
53.7660178032496));
#11319=CARTESIAN_POINT('Ctrl Pts',(-3.3897124498917,0.0473409919946466,
53.763397281338));
#11320=CARTESIAN_POINT('Ctrl Pts',(-3.38879693886487,0.0918770320527466,
53.7607767594264));
#11321=CARTESIAN_POINT('Ctrl Pts',(-3.38700661857411,0.136349654327203,
53.7581562375148));
#11322=CARTESIAN_POINT('Origin',(0.,0.,0.));
#11323=CARTESIAN_POINT('',(-3.38743469189442,0.136371088936278,52.5078428482942));
#11324=CARTESIAN_POINT('',(-3.3870066183502,0.136349659889395,52.8536715661706));
#11325=CARTESIAN_POINT('',(-3.38700661857411,0.136349654327212,0.));
#11326=CARTESIAN_POINT('Ctrl Pts',(-3.3870066183502,0.136349659889395,52.8536715661706));
#11327=CARTESIAN_POINT('Ctrl Pts',(-3.38885798329129,0.090360654023626,
52.8562620823228));
#11328=CARTESIAN_POINT('Ctrl Pts',(-3.38977266289487,0.0443345664023467,
52.8588265392501));
#11329=CARTESIAN_POINT('Ctrl Pts',(-3.38962280610553,-0.254445741724597,
52.8753257019146));
#11330=CARTESIAN_POINT('Ctrl Pts',(-3.3612305356205,-0.50637572230606,52.8884778259417));
#11331=CARTESIAN_POINT('Ctrl Pts',(-3.27688841398311,-0.876665695222036,
52.9088225462481));
#11332=CARTESIAN_POINT('Ctrl Pts',(-3.24174102107433,-0.998824148034817,
52.9157237313064));
#11333=CARTESIAN_POINT('Ctrl Pts',(-3.18915375802687,-1.14923855903693,
52.9247744573728));
#11334=CARTESIAN_POINT('Ctrl Pts',(-3.17804464081704,-1.17961140085019,
52.9266313154987));
#11335=CARTESIAN_POINT('Ctrl Pts',(-3.15993345097052,-1.22701445647214,
52.9295822425549));
#11336=CARTESIAN_POINT('Ctrl Pts',(-3.15322400662735,-1.24415522370565,
52.9306602736426));
#11337=CARTESIAN_POINT('Ctrl Pts',(-3.13865471048719,-1.28050078342945,
52.9329712903503));
#11338=CARTESIAN_POINT('Ctrl Pts',(-3.13075750988737,-1.2996895806954,52.9342065064485));
#11339=CARTESIAN_POINT('Ctrl Pts',(-3.10946731904312,-1.35010082885317,
52.9374892526451));
#11340=CARTESIAN_POINT('Ctrl Pts',(-3.09578051594554,-1.38119588156737,
52.9395525888828));
#11341=CARTESIAN_POINT('Ctrl Pts',(-3.00851727444757,-1.57163354422528,
52.9524048891755));
#11342=CARTESIAN_POINT('Ctrl Pts',(-2.9231296558358,-1.72525696214465,52.9636985676011));
#11343=CARTESIAN_POINT('Ctrl Pts',(-2.69980866555869,-2.06249284571376,
52.9897377104267));
#11344=CARTESIAN_POINT('Ctrl Pts',(-2.55433591656216,-2.24014269858376,
53.0043896339951));
#11345=CARTESIAN_POINT('Ctrl Pts',(-2.35082654683572,-2.44282686540813,
53.0219095429194));
#11346=CARTESIAN_POINT('Ctrl Pts',(-2.30856082778187,-2.48280810181074,
53.0254145565268));
#11347=CARTESIAN_POINT('Ctrl Pts',(-2.23791751802748,-2.54626857259377,
53.031062758679));
#11348=CARTESIAN_POINT('Ctrl Pts',(-2.2101508069525,-2.57040697745637,53.0332326016579));
#11349=CARTESIAN_POINT('Ctrl Pts',(-2.15497811275992,-2.61681501248026,
53.0374491577784));
#11350=CARTESIAN_POINT('Ctrl Pts',(-2.12760633045955,-2.63911782888246,
53.0394970426046));
#11351=CARTESIAN_POINT('Ctrl Pts',(-2.06056113415274,-2.69202580007891,
53.044411405192));
#11352=CARTESIAN_POINT('Ctrl Pts',(-2.02054737518682,-2.72218731236242,
53.0472606428668));
#11353=CARTESIAN_POINT('Ctrl Pts',(-1.85128611980178,-2.84398361657381,
53.0589926042189));
#11354=CARTESIAN_POINT('Ctrl Pts',(-1.71635952028096,-2.92739135329188,
53.0675755975238));
#11355=CARTESIAN_POINT('Ctrl Pts',(-1.39292525994255,-3.0972508890093,53.0870878916235));
#11356=CARTESIAN_POINT('Ctrl Pts',(-1.20135985671553,-3.17646472593229,
53.0978835547358));
#11357=CARTESIAN_POINT('Ctrl Pts',(-0.937176706167467,-3.25836887632998,
53.1130638783348));
#11358=CARTESIAN_POINT('Ctrl Pts',(-0.869953025628567,-3.27695718339984,
53.1169533846755));
#11359=CARTESIAN_POINT('Ctrl Pts',(-0.775403481268927,-3.29998721937711,
53.1225202139044));
#11360=CARTESIAN_POINT('Ctrl Pts',(-0.748520558821123,-3.30618860241921,
53.1241137448057));
#11361=CARTESIAN_POINT('Ctrl Pts',(-0.702376320504877,-3.31624159008216,
53.1268719367306));
#11362=CARTESIAN_POINT('Ctrl Pts',(-0.683152160469688,-3.3202550936674,
53.128027914092));
#11363=CARTESIAN_POINT('Ctrl Pts',(-0.640995870128654,-3.32867459540301,
53.1305790841751));
#11364=CARTESIAN_POINT('Ctrl Pts',(-0.618052515149012,-3.33301084428786,
53.1319776609449));
#11365=CARTESIAN_POINT('Ctrl Pts',(-0.54881970116538,-3.34535630569313,
53.136224632438));
#11366=CARTESIAN_POINT('Ctrl Pts',(-0.502408386572499,-3.35264033715182,
53.1391074229554));
#11367=CARTESIAN_POINT('Ctrl Pts',(-0.226705302833743,-3.39005757404586,
53.1563864938663));
#11368=CARTESIAN_POINT('Ctrl Pts',(0.0050255618206228,-3.39762513213806,
53.1714903160061));
#11369=CARTESIAN_POINT('Ctrl Pts',(0.401305076754971,-3.37000181387177,
53.196880230899));
#11370=CARTESIAN_POINT('Ctrl Pts',(0.565838787195996,-3.3463108943855,53.2073004596762));
#11371=CARTESIAN_POINT('Ctrl Pts',(0.777804374637566,-3.29970099556454,
53.2204556983712));
#11372=CARTESIAN_POINT('Ctrl Pts',(0.827364991889574,-3.28762435433156,
53.2235133426087));
#11373=CARTESIAN_POINT('Ctrl Pts',(0.910547954114985,-3.26535448506558,
53.2286168824168));
#11374=CARTESIAN_POINT('Ctrl Pts',(0.944317431691197,-3.25574910196942,
53.230680760338));
#11375=CARTESIAN_POINT('Ctrl Pts',(1.01284941787929,-3.23509984260165,53.2348548808183));
#11376=CARTESIAN_POINT('Ctrl Pts',(1.04759514365871,-3.22401605124798,53.2369635412927));
#11377=CARTESIAN_POINT('Ctrl Pts',(1.13569381875675,-3.19433814031534,53.2422946214143));
#11378=CARTESIAN_POINT('Ctrl Pts',(1.1887741018071,-3.1749666529573,53.245491866065));
#11379=CARTESIAN_POINT('Ctrl Pts',(1.41178798794155,-3.08720080825328,53.2588960860065));
#11380=CARTESIAN_POINT('Ctrl Pts',(1.57651739515791,-3.00641903721444,53.26870476174));
#11381=CARTESIAN_POINT('Ctrl Pts',(1.92504928497801,-2.79893975976317,53.2902628690432));
#11382=CARTESIAN_POINT('Ctrl Pts',(2.10448949170084,-2.666642059985,53.3019240501951));
#11383=CARTESIAN_POINT('Ctrl Pts',(2.29579079117951,-2.49419074111917,53.3164999363096));
#11384=CARTESIAN_POINT('Ctrl Pts',(2.32155267502854,-2.4702299049804,53.3185138071492));
#11385=CARTESIAN_POINT('Ctrl Pts',(2.3620902765292,-2.43133208245837,53.3217741676592));
#11386=CARTESIAN_POINT('Ctrl Pts',(2.37710875644105,-2.41665059102843,53.3230027877577));
#11387=CARTESIAN_POINT('Ctrl Pts',(2.40668067456327,-2.38719984390909,53.3254658686477));
#11388=CARTESIAN_POINT('Ctrl Pts',(2.42123690728599,-2.37243477168986,53.3267000386163));
#11389=CARTESIAN_POINT('Ctrl Pts',(2.45922896035533,-2.33318382467216,53.3299768281626));
#11390=CARTESIAN_POINT('Ctrl Pts',(2.48243408742767,-2.30847886103826,53.3320351572997));
#11391=CARTESIAN_POINT('Ctrl Pts',(2.53372104529874,-2.2522094334881,53.3367059232514));
#11392=CARTESIAN_POINT('Ctrl Pts',(2.56159092738067,-2.2204597041786,53.3393294895995));
#11393=CARTESIAN_POINT('Ctrl Pts',(2.6506195517551,-2.11512989733755,53.3479729135561));
#11394=CARTESIAN_POINT('Ctrl Pts',(2.70925611841536,-2.03948230091072,53.3540862939258));
#11395=CARTESIAN_POINT('Ctrl Pts',(2.9156333825492,-1.74860052015084,53.3769999900173));
#11396=CARTESIAN_POINT('Ctrl Pts',(3.04159073019534,-1.51897523051815,53.3938516392515));
#11397=CARTESIAN_POINT('Ctrl Pts',(3.16298865604935,-1.22051071625204,53.413551782908));
#11398=CARTESIAN_POINT('Ctrl Pts',(3.18449008889452,-1.16325716686628,53.4172430416015));
#11399=CARTESIAN_POINT('Ctrl Pts',(3.21661719117919,-1.07012850821992,53.4231098999423));
#11400=CARTESIAN_POINT('Ctrl Pts',(3.22821787227389,-1.03460655006405,53.4253162380643));
#11401=CARTESIAN_POINT('Ctrl Pts',(3.24954597043363,-0.965443800308088,
53.4295535471454));
#11402=CARTESIAN_POINT('Ctrl Pts',(3.2593440758806,-0.931829959601022,53.4315865444558));
#11403=CARTESIAN_POINT('Ctrl Pts',(3.28140793265502,-0.851526186780927,
53.4363840131463));
#11404=CARTESIAN_POINT('Ctrl Pts',(3.29320075221251,-0.804713613622579,
53.4391333699168));
#11405=CARTESIAN_POINT('Ctrl Pts',(3.33429680626021,-0.625503486553928,
53.4494971391396));
#11406=CARTESIAN_POINT('Ctrl Pts',(3.35664823094535,-0.491637535292613,
53.4568997854144));
#11407=CARTESIAN_POINT('Ctrl Pts',(3.38594981301633,-0.214792454780028,
53.4718536075304));
#11408=CARTESIAN_POINT('Ctrl Pts',(3.39199186502904,-0.0719958942982847,
53.4793767791466));
#11409=CARTESIAN_POINT('Ctrl Pts',(3.38613296549362,0.20862635739138,53.4943414166087));
#11410=CARTESIAN_POINT('Ctrl Pts',(3.37484426580657,0.346180651397624,53.5017648360333));
#11411=CARTESIAN_POINT('Ctrl Pts',(3.34962880555744,0.521468955304257,53.5117400661906));
#11412=CARTESIAN_POINT('Ctrl Pts',(3.34337196287359,0.560184479288933,53.5139762506026));
#11413=CARTESIAN_POINT('Ctrl Pts',(3.33258790360751,0.62027393360538,53.517510387474));
#11414=CARTESIAN_POINT('Ctrl Pts',(3.32852315444243,0.64172848019871,53.5187848983954));
#11415=CARTESIAN_POINT('Ctrl Pts',(3.32030952213742,0.682902459952344,53.5212578106338));
#11416=CARTESIAN_POINT('Ctrl Pts',(3.31619160074067,0.702626703030152,53.5224546077159));
#11417=CARTESIAN_POINT('Ctrl Pts',(3.30531120535703,0.752514769831181,53.5255107260587));
#11418=CARTESIAN_POINT('Ctrl Pts',(3.29831156883901,0.782624617058191,53.5273822316073));
#11419=CARTESIAN_POINT('Ctrl Pts',(3.26464852653738,0.918949018263562,53.5359657875073));
#11420=CARTESIAN_POINT('Ctrl Pts',(3.23326114171657,1.02392174267986,53.5428789673085));
#11421=CARTESIAN_POINT('Ctrl Pts',(3.14555808507566,1.27266038465735,53.5597311700279));
#11422=CARTESIAN_POINT('Ctrl Pts',(3.08439317204763,1.41446811678783,53.5697265280043));
#11423=CARTESIAN_POINT('Ctrl Pts',(2.93961036044075,1.69568657637012,53.5899274326136));
#11424=CARTESIAN_POINT('Ctrl Pts',(2.85519664450187,1.83426429852382,53.6000900035199));
#11425=CARTESIAN_POINT('Ctrl Pts',(2.73165818452038,2.00774479450128,53.6129980068788));
#11426=CARTESIAN_POINT('Ctrl Pts',(2.70120316788931,2.04853544265164,53.6160490993045));
#11427=CARTESIAN_POINT('Ctrl Pts',(2.64821995555896,2.11626257858412,53.6211450430547));
#11428=CARTESIAN_POINT('Ctrl Pts',(2.62617174886801,2.14356206270229,53.6232077521041));
#11429=CARTESIAN_POINT('Ctrl Pts',(2.58033553382868,2.19854619657751,53.6273821356807));
#11430=CARTESIAN_POINT('Ctrl Pts',(2.55651629028332,2.22619887976334,53.6294921853701));
#11431=CARTESIAN_POINT('Ctrl Pts',(2.4946069398356,2.29576748384065,53.6348322910165));
#11432=CARTESIAN_POINT('Ctrl Pts',(2.45590381723638,2.3371241036674,53.6380369919694));
#11433=CARTESIAN_POINT('Ctrl Pts',(2.30411993784524,2.49137788343762,53.6501392043006));
#11434=CARTESIAN_POINT('Ctrl Pts',(2.18414084450859,2.59720382163998,53.6587487917959));
#11435=CARTESIAN_POINT('Ctrl Pts',(1.86536944513923,2.84060146606205,53.6801182829856));
#11436=CARTESIAN_POINT('Ctrl Pts',(1.65853954576827,2.9661152993283,53.6926755684377));
#11437=CARTESIAN_POINT('Ctrl Pts',(1.40620340821925,3.08454290767146,53.7084066274108));
#11438=CARTESIAN_POINT('Ctrl Pts',(1.37197524368227,3.09991881551319,53.7105495486316));
#11439=CARTESIAN_POINT('Ctrl Pts',(1.31775493481248,3.12320168593756,53.7139688610426));
#11440=CARTESIAN_POINT('Ctrl Pts',(1.29792984466635,3.13149244033557,53.7152242227484));
#11441=CARTESIAN_POINT('Ctrl Pts',(1.25917405728812,3.14726867674767,53.7176907248316));
#11442=CARTESIAN_POINT('Ctrl Pts',(1.24025238214931,3.1547731118327,53.7189007849583));
#11443=CARTESIAN_POINT('Ctrl Pts',(1.19140707186828,3.17363809059535,53.7220374696585));
#11444=CARTESIAN_POINT('Ctrl Pts',(1.16138842798264,3.18474587665938,53.7239775563707));
#11445=CARTESIAN_POINT('Ctrl Pts',(1.01079097960334,3.23805912851354,53.7337565137636));
#11446=CARTESIAN_POINT('Ctrl Pts',(0.888059672820282,3.27384632969777,53.7418683450188));
#11447=CARTESIAN_POINT('Ctrl Pts',(0.483561204869113,3.36737225583087,53.7684938398514));
#11448=CARTESIAN_POINT('Ctrl Pts',(0.196352309392905,3.39625175660232,53.787107687746));
#11449=CARTESIAN_POINT('Ctrl Pts',(-0.145920713740234,3.3870521458296,53.8079352164141));
#11450=CARTESIAN_POINT('Ctrl Pts',(-0.200722974356862,3.38424672584363,
53.8112337773401));
#11451=CARTESIAN_POINT('Ctrl Pts',(-0.291491544816678,3.37738733451354,
53.8166396593038));
#11452=CARTESIAN_POINT('Ctrl Pts',(-0.327502701276744,3.37408575150571,
53.8187693411268));
#11453=CARTESIAN_POINT('Ctrl Pts',(-0.399009248509365,3.36637423260744,
53.8229703357184));
#11454=CARTESIAN_POINT('Ctrl Pts',(-0.434501321906444,3.36197748305969,
53.82504176409));
#11455=CARTESIAN_POINT('Ctrl Pts',(-0.522113281326584,3.34971349433156,
53.8301246383504));
#11456=CARTESIAN_POINT('Ctrl Pts',(-0.574132686689068,3.34119063346354,
53.8331157161812));
#11457=CARTESIAN_POINT('Ctrl Pts',(-0.836960791282227,3.29180891568344,
53.8481235844396));
#11458=CARTESIAN_POINT('Ctrl Pts',(-1.04374769815246,3.23219913396659,53.8595485025921));
#11459=CARTESIAN_POINT('Ctrl Pts',(-1.42404672304241,3.08223187924565,53.8812546604134));
#11460=CARTESIAN_POINT('Ctrl Pts',(-1.59810771360037,2.99567998575996,53.8915139594138));
#11461=CARTESIAN_POINT('Ctrl Pts',(-1.79606439957106,2.87506280281147,53.9045920959586));
#11462=CARTESIAN_POINT('Ctrl Pts',(-1.8280066086371,2.85485989831206,53.9067499878424));
#11463=CARTESIAN_POINT('Ctrl Pts',(-1.87761648768503,2.8223085543644,53.9101877376386));
#11464=CARTESIAN_POINT('Ctrl Pts',(-1.89551640211223,2.81031791192903,53.9114461861937));
#11465=CARTESIAN_POINT('Ctrl Pts',(-1.93007366748487,2.7866886422809,53.9139135270737));
#11466=CARTESIAN_POINT('Ctrl Pts',(-1.94674280044033,2.77506943107268,53.9151212526667));
#11467=CARTESIAN_POINT('Ctrl Pts',(-1.98924410726643,2.7448725595004,53.9182439921702));
#11468=CARTESIAN_POINT('Ctrl Pts',(-2.01492065489445,2.7260799844922,53.9201722465617));
#11469=CARTESIAN_POINT('Ctrl Pts',(-2.13944206965429,2.63222290170996,53.9297149221311));
#11470=CARTESIAN_POINT('Ctrl Pts',(-2.23437044782411,2.55213503843991,53.9375871708117));
#11471=CARTESIAN_POINT('Ctrl Pts',(-2.53296903998981,2.27076533082989,53.9638827342647));
#11472=CARTESIAN_POINT('Ctrl Pts',(-2.71559968869029,2.04887199185127,53.9824370793653));
#11473=CARTESIAN_POINT('Ctrl Pts',(-2.89879238953796,1.7580408283262,54.003390690979));
#11474=CARTESIAN_POINT('Ctrl Pts',(-2.92816929547138,1.70866323326224,54.0068504527771));
#11475=CARTESIAN_POINT('Ctrl Pts',(-2.9742104486785,1.62659781187271,54.0124455118186));
#11476=CARTESIAN_POINT('Ctrl Pts',(-2.99162343331729,1.59434551587221,54.014606501733));
#11477=CARTESIAN_POINT('Ctrl Pts',(-3.0248168476347,1.53040538362912,54.0188188610676));
#11478=CARTESIAN_POINT('Ctrl Pts',(-3.04063072914205,1.49874030639207,54.0208711817759));
#11479=CARTESIAN_POINT('Ctrl Pts',(-3.07784726944555,1.42120469938868,54.0258184597566));
#11480=CARTESIAN_POINT('Ctrl Pts',(-3.09872438510022,1.37509060441782,54.0286955728289));
#11481=CARTESIAN_POINT('Ctrl Pts',(-3.18385868700254,1.17524741255232,54.0409104488996));
#11482=CARTESIAN_POINT('Ctrl Pts',(-3.23776973060225,1.01735812739505,54.0499128157608));
#11483=CARTESIAN_POINT('Ctrl Pts',(-3.34130616867213,0.62070800530699,54.0717742388552));
#11484=CARTESIAN_POINT('Ctrl Pts',(-3.37722260790877,0.379390304076916,
54.0844189787722));
#11485=CARTESIAN_POINT('Ctrl Pts',(-3.38700661852469,0.136349655555036,
54.0981108245895));
#11486=CARTESIAN_POINT('',(-3.38974892034748,-0.00270545801625161,52.5160178032496));
#11487=CARTESIAN_POINT('Ctrl Pts',(-3.38700661857411,0.136349654327203,
53.7581562375148));
#11488=CARTESIAN_POINT('Ctrl Pts',(-3.38089832230461,0.288083371549333,
53.7492154215617));
#11489=CARTESIAN_POINT('Ctrl Pts',(-3.3646031929328,0.439076737459294,53.7402746056086));
#11490=CARTESIAN_POINT('Ctrl Pts',(-3.33832120308359,0.588231763459373,
53.7313337896555));
#11491=CARTESIAN_POINT('Ctrl Pts',(-3.33584314013142,0.6022952170328,53.7304907825277));
#11492=CARTESIAN_POINT('Ctrl Pts',(-3.33327632582759,0.616342345712101,
53.7296477753999));
#11493=CARTESIAN_POINT('Ctrl Pts',(-3.33062094849041,0.630372239218109,
53.7288047682721));
#11494=CARTESIAN_POINT('Ctrl Pts',(-3.31139138984876,0.731973113840281,
53.7226999278141));
#11495=CARTESIAN_POINT('Ctrl Pts',(-3.28747651147585,0.832862740521183,
53.7165950873561));
#11496=CARTESIAN_POINT('Ctrl Pts',(-3.25894239268673,0.932576829890859,
53.7104902468981));
#11497=CARTESIAN_POINT('Ctrl Pts',(-3.23044548929775,1.03216086794328,53.7043933686303));
#11498=CARTESIAN_POINT('Ctrl Pts',(-3.19734143965255,1.13057200949136,53.6982964903625));
#11499=CARTESIAN_POINT('Ctrl Pts',(-3.15974750580198,1.22735518986076,53.6921996120947));
#11500=CARTESIAN_POINT('Ctrl Pts',(-3.12219188159578,1.32403974449882,53.6861089467771));
#11501=CARTESIAN_POINT('Ctrl Pts',(-3.08015562554104,1.41909924075953,53.6800182814594));
#11502=CARTESIAN_POINT('Ctrl Pts',(-3.03380582163393,1.51209368066932,53.6739276161418));
#11503=CARTESIAN_POINT('Ctrl Pts',(-2.98748850473577,1.60502293991064,53.6678412198282));
#11504=CARTESIAN_POINT('Ctrl Pts',(-2.93686384247436,1.69588963992659,53.6617548235146));
#11505=CARTESIAN_POINT('Ctrl Pts',(-2.88214672577944,1.78427445018384,53.655668427201));
#11506=CARTESIAN_POINT('Ctrl Pts',(-2.82744947496616,1.87262717099111,53.6495842406461));
#11507=CARTESIAN_POINT('Ctrl Pts',(-2.76866294749466,1.95849943013418,53.6435000540913));
#11508=CARTESIAN_POINT('Ctrl Pts',(-2.70604720913747,2.04149787274425,53.6374158675365));
#11509=CARTESIAN_POINT('Ctrl Pts',(-2.64343803376025,2.12448761599007,53.631332318687));
#11510=CARTESIAN_POINT('Ctrl Pts',(-2.57700070295938,2.20460380069758,53.6252487698376));
#11511=CARTESIAN_POINT('Ctrl Pts',(-2.50703716190101,2.2814841071871,53.6191652209882));
#11512=CARTESIAN_POINT('Ctrl Pts',(-2.43706288608055,2.35837620970335,53.6130807387176));
#11513=CARTESIAN_POINT('Ctrl Pts',(-2.36356161262207,2.43203113159341,53.606996256447));
#11514=CARTESIAN_POINT('Ctrl Pts',(-2.2868732924771,2.50212222056696,53.6009117741764));
#11515=CARTESIAN_POINT('Ctrl Pts',(-2.21010590771101,2.57228557250551,53.5948210188868));
#11516=CARTESIAN_POINT('Ctrl Pts',(-2.1301452304708,2.63887746531716,53.5887302635973));
#11517=CARTESIAN_POINT('Ctrl Pts',(-2.04736552501942,2.70161053252721,53.5826395083078));
#11518=CARTESIAN_POINT('Ctrl Pts',(-1.96454102472262,2.76437754668154,53.5765454571084));
#11519=CARTESIAN_POINT('Ctrl Pts',(-1.87889480957758,2.82328133367252,53.5704514059091));
#11520=CARTESIAN_POINT('Ctrl Pts',(-1.79082980884284,2.87807811885986,53.5643573547097));
#11521=CARTESIAN_POINT('Ctrl Pts',(-1.70262368180194,2.93296271722858,53.5582535376451));
#11522=CARTESIAN_POINT('Ctrl Pts',(-1.61199139918918,2.98372695783321,53.5521497205805));
#11523=CARTESIAN_POINT('Ctrl Pts',(-1.51936030942531,3.0301731489542,53.5460459035158));
#11524=CARTESIAN_POINT('Ctrl Pts',(-1.45109889423784,3.06440013196897,53.5415478975878));
#11525=CARTESIAN_POINT('Ctrl Pts',(-1.38175253004824,3.09628319019804,53.5370498916597));
#11526=CARTESIAN_POINT('Ctrl Pts',(-1.31149811501989,3.12576034858709,53.5325518857317));
#11527=CARTESIAN_POINT('Ctrl Pts',(-1.21614651747083,3.16576771527668,53.5264470444794));
#11528=CARTESIAN_POINT('Ctrl Pts',(-1.11880358129998,3.20147477068205,53.5203422032271));
#11529=CARTESIAN_POINT('Ctrl Pts',(-1.01989301568441,3.2326805129889,53.5142373619747));
#11530=CARTESIAN_POINT('Ctrl Pts',(-0.921111453306506,3.26384555548005,
53.508140482908));
#11531=CARTESIAN_POINT('Ctrl Pts',(-0.82076673036726,3.29052082920096,53.5020436038414));
#11532=CARTESIAN_POINT('Ctrl Pts',(-0.719303095967168,3.31255311182056,
53.4959467247747));
#11533=CARTESIAN_POINT('Ctrl Pts',(-0.617942856788223,3.33456294272386,
53.4898560586548));
#11534=CARTESIAN_POINT('Ctrl Pts',(-0.515466388872144,3.35193910107061,
53.4837653925349));
#11535=CARTESIAN_POINT('Ctrl Pts',(-0.412332857848781,3.36457823164186,
53.477674726415));
#11536=CARTESIAN_POINT('Ctrl Pts',(-0.309271614037571,3.37720850333371,
53.4715883292973));
#11537=CARTESIAN_POINT('Ctrl Pts',(-0.205554645802275,3.385108298159,53.4655019321796));
#11538=CARTESIAN_POINT('Ctrl Pts',(-0.101650252254103,3.38822553687276,
53.4594155350619));
#11539=CARTESIAN_POINT('Ctrl Pts',(0.00221641724162593,3.39134164382613,
53.4533313477022));
#11540=CARTESIAN_POINT('Ctrl Pts',(0.10626995023665,3.3896786329916,53.4472471603425));
#11541=CARTESIAN_POINT('Ctrl Pts',(0.210038793604787,3.38323643390187,53.4411629729828));
#11542=CARTESIAN_POINT('Ctrl Pts',(0.313796760586779,3.37679491004223,53.4350794233287));
#11543=CARTESIAN_POINT('Ctrl Pts',(0.417269670903458,3.36557522059296,53.4289958736746));
#11544=CARTESIAN_POINT('Ctrl Pts',(0.519988755373871,3.34962934617918,53.4229123240205));
#11545=CARTESIAN_POINT('Ctrl Pts',(0.622723600387313,3.33368102513494,53.4168278409464));
#11546=CARTESIAN_POINT('Ctrl Pts',(0.724703967579495,3.31300514393209,53.4107433578723));
#11547=CARTESIAN_POINT('Ctrl Pts',(0.825469872181442,3.28770505864208,53.4046588747982));
#11548=CARTESIAN_POINT('Ctrl Pts',(0.926339664943076,3.26237888933774,53.3985681187119));
#11549=CARTESIAN_POINT('Ctrl Pts',(1.02599207958538,3.23241909955356,53.3924773626257));
#11550=CARTESIAN_POINT('Ctrl Pts',(1.12398097072417,3.1979793370111,53.3863866065394));
#11551=CARTESIAN_POINT('Ctrl Pts',(1.22202288685473,3.16352093798746,53.3802925545459));
#11552=CARTESIAN_POINT('Ctrl Pts',(1.3183990902397,3.12457789727113,53.3741985025524));
#11553=CARTESIAN_POINT('Ctrl Pts',(1.41268398227067,3.08135181839657,53.3681044505589));
#11554=CARTESIAN_POINT('Ctrl Pts',(1.50711996792513,3.03805646877518,53.3620006327124));
#11555=CARTESIAN_POINT('Ctrl Pts',(1.59945756773846,2.99046456621031,53.3558968148659));
#11556=CARTESIAN_POINT('Ctrl Pts',(1.68929614980463,2.93882350282477,53.3497929970194));
#11557=CARTESIAN_POINT('Ctrl Pts',(1.75549959287608,2.90076840309629,53.3452949990765));
#11558=CARTESIAN_POINT('Ctrl Pts',(1.8203464993356,2.86051538189802,53.3407970011337));
#11559=CARTESIAN_POINT('Ctrl Pts',(1.8836875944295,2.81817779941089,53.3362990031909));
#11560=CARTESIAN_POINT('Ctrl Pts',(1.96965632723492,2.76071576293887,53.3301941642592));
#11561=CARTESIAN_POINT('Ctrl Pts',(2.05313672094171,2.69922058348168,53.3240893253275));
#11562=CARTESIAN_POINT('Ctrl Pts',(2.13372739052763,2.6339347914123,53.3179844863958));
#11563=CARTESIAN_POINT('Ctrl Pts',(2.21421295037924,2.56873414781351,53.3118876096513));
#11564=CARTESIAN_POINT('Ctrl Pts',(2.2918159498874,2.49975298727891,53.3057907329068));
#11565=CARTESIAN_POINT('Ctrl Pts',(2.36616352571386,2.42727732904202,53.2996938561623));
#11566=CARTESIAN_POINT('Ctrl Pts',(2.44043533858205,2.35487552620941,53.2936031923631));
#11567=CARTESIAN_POINT('Ctrl Pts',(2.51145802035402,2.27898660371923,53.2875125285638));
#11568=CARTESIAN_POINT('Ctrl Pts',(2.57889207269775,2.19993653087463,53.2814218647646));
#11569=CARTESIAN_POINT('Ctrl Pts',(2.64627886002463,2.12094186479998,53.2753354699558));
#11570=CARTESIAN_POINT('Ctrl Pts',(2.71008174346828,2.03879077863847,53.2692490751471));
#11571=CARTESIAN_POINT('Ctrl Pts',(2.7699989549438,1.95384514537623,53.2631626803383));
#11572=CARTESIAN_POINT('Ctrl Pts',(2.82989441264589,1.86893035280257,53.2570784952795));
#11573=CARTESIAN_POINT('Ctrl Pts',(2.8859067563119,1.78122337841738,53.2509943102206));
#11574=CARTESIAN_POINT('Ctrl Pts',(2.93777580264318,1.69111749914198,53.2449101251618));
#11575=CARTESIAN_POINT('Ctrl Pts',(2.98963941248285,1.60102106403206,53.2388265777978));
#11576=CARTESIAN_POINT('Ctrl Pts',(3.03736037549326,1.50852659430234,53.2327430304337));
#11577=CARTESIAN_POINT('Ctrl Pts',(3.08072345920221,1.41405375796721,53.2266594830697));
#11578=CARTESIAN_POINT('Ctrl Pts',(3.12409319635748,1.31956642612366,53.2205750022722));
#11579=CARTESIAN_POINT('Ctrl Pts',(3.16310354751013,1.22310051286622,53.2144905214746));
#11580=CARTESIAN_POINT('Ctrl Pts',(3.19758697752962,1.12509669968097,53.208406040677));
#11581=CARTESIAN_POINT('Ctrl Pts',(3.23210595966656,1.02699184541382,53.2023152868325));
#11582=CARTESIAN_POINT('Ctrl Pts',(3.26208855823222,0.927346328604415,53.196224532988));
#11583=CARTESIAN_POINT('Ctrl Pts',(3.28741681995202,0.826617030066845,53.1901337791435));
#11584=CARTESIAN_POINT('Ctrl Pts',(3.31275878769398,0.725833223327642,53.1840397293757));
#11585=CARTESIAN_POINT('Ctrl Pts',(3.33344131661272,0.623964885329891,53.1779456796079));
#11586=CARTESIAN_POINT('Ctrl Pts',(3.34939778702454,0.521478213135649,53.1718516298401));
#11587=CARTESIAN_POINT('Ctrl Pts',(3.36537982816956,0.41882730290603,53.1657478141707));
#11588=CARTESIAN_POINT('Ctrl Pts',(3.37662063571285,0.31555650399105,53.1596439985013));
#11589=CARTESIAN_POINT('Ctrl Pts',(3.3831055540886,0.21213644758713,53.1535401828318));
#11590=CARTESIAN_POINT('Ctrl Pts',(3.38788441682756,0.13592419241689,53.1490421621047));
#11591=CARTESIAN_POINT('Ctrl Pts',(3.39008168558463,0.0596309572089956,
53.1445441413775));
#11592=CARTESIAN_POINT('Ctrl Pts',(3.38970956783697,-0.0165562137738431,
53.1400461206503));
#11593=CARTESIAN_POINT('Ctrl Pts',(3.38920451911107,-0.119959595837954,
53.1339412797724));
#11594=CARTESIAN_POINT('Ctrl Pts',(3.38396282606339,-0.22351230565078,53.1278364388946));
#11595=CARTESIAN_POINT('Ctrl Pts',(3.37396536250715,-0.326745765239541,
53.1217315980167));
#11596=CARTESIAN_POINT('Ctrl Pts',(3.36398093808233,-0.429844583212729,
53.1156347193406));
#11597=CARTESIAN_POINT('Ctrl Pts',(3.34925311562263,-0.532624557058128,
53.1095378406646));
#11598=CARTESIAN_POINT('Ctrl Pts',(3.32981477593396,-0.634616908435232,
53.1034409619885));
#11599=CARTESIAN_POINT('Ctrl Pts',(3.31039624468753,-0.736505325544588,
53.0973502962746));
#11600=CARTESIAN_POINT('Ctrl Pts',(3.28627682136983,-0.837607298772716,
53.0912596305607));
#11601=CARTESIAN_POINT('Ctrl Pts',(3.25754111386167,-0.937459841273676,
53.0851689648468));
#11602=CARTESIAN_POINT('Ctrl Pts',(3.22882554756865,-1.0372423958845,53.0790825681564));
#11603=CARTESIAN_POINT('Ctrl Pts',(3.1955002493585,-1.13577685192026,53.0729961714659));
#11604=CARTESIAN_POINT('Ctrl Pts',(3.15770058716458,-1.23261188714066,53.0669097747754));
#11605=CARTESIAN_POINT('Ctrl Pts',(3.11991464878697,-1.32941176473906,53.0608255878558));
#11606=CARTESIAN_POINT('Ctrl Pts',(3.07765773035409,-1.42451305029741,53.0547414009361));
#11607=CARTESIAN_POINT('Ctrl Pts',(3.03111433296921,-1.51748178340586,53.0486572140165));
#11608=CARTESIAN_POINT('Ctrl Pts',(2.98457581405908,-1.61044077193951,53.0425736648146));
#11609=CARTESIAN_POINT('Ctrl Pts',(2.93375190095082,-1.70126727054694,53.0364901156127));
#11610=CARTESIAN_POINT('Ctrl Pts',(2.87887390359773,-1.78955025346704,53.0304065664109));
#11611=CARTESIAN_POINT('Ctrl Pts',(2.8239874862283,-1.87784678178231,53.0243220838006));
#11612=CARTESIAN_POINT('Ctrl Pts',(2.76504597433088,-1.96359865620777,53.0182376011903));
#11613=CARTESIAN_POINT('Ctrl Pts',(2.70232451638145,-2.04642304293706,53.01215311858));
#11614=CARTESIAN_POINT('Ctrl Pts',(2.63953839368367,-2.12933282018978,53.0060623629725));
#11615=CARTESIAN_POINT('Ctrl Pts',(2.57296480093383,-2.20930874125264,52.9999716073649));
#11616=CARTESIAN_POINT('Ctrl Pts',(2.50291974928054,-2.28600039176756,52.9938808517573));
#11617=CARTESIAN_POINT('Ctrl Pts',(2.43283679406054,-2.36273354253157,52.9877868002515));
#11618=CARTESIAN_POINT('Ctrl Pts',(2.35927894036816,-2.43617858074976,52.9816927487457));
#11619=CARTESIAN_POINT('Ctrl Pts',(2.28259828726525,-2.50602276954416,52.9755986972399));
#11620=CARTESIAN_POINT('Ctrl Pts',(2.20579475183068,-2.57597888509483,52.9694948798906));
#11621=CARTESIAN_POINT('Ctrl Pts',(2.1258587493692,-2.6423223514547,52.9633910625413));
#11622=CARTESIAN_POINT('Ctrl Pts',(2.04317474257019,-2.70478132828206,52.9572872451919));
#11623=CARTESIAN_POINT('Ctrl Pts',(1.98224355205528,-2.75080836499406,52.9527892428312));
#11624=CARTESIAN_POINT('Ctrl Pts',(1.91982073489687,-2.79472681761542,52.9482912404704));
#11625=CARTESIAN_POINT('Ctrl Pts',(1.85606903414094,-2.83644368937638,52.9437932381097));
#11626=CARTESIAN_POINT('Ctrl Pts',(1.76954300026846,-2.89306328408904,52.9376883922779));
#11627=CARTESIAN_POINT('Ctrl Pts',(1.68027951834246,-2.94581447430127,52.9315835464462));
#11628=CARTESIAN_POINT('Ctrl Pts',(1.58865887313047,-2.99442282373813,52.9254787006145));
#11629=CARTESIAN_POINT('Ctrl Pts',(1.49715772291929,-3.04296777638552,52.9193818169462));
#11630=CARTESIAN_POINT('Ctrl Pts',(1.40330589574736,-3.08738043194736,52.913284933278));
#11631=CARTESIAN_POINT('Ctrl Pts',(1.30751253226124,-3.12742962198669,52.9071880496098));
#11632=CARTESIAN_POINT('Ctrl Pts',(1.21181678545712,-3.16743800054486,52.9010973788725));
#11633=CARTESIAN_POINT('Ctrl Pts',(1.1141838288362,-3.20309159190741,52.8950067081353));
#11634=CARTESIAN_POINT('Ctrl Pts',(1.0150465067861,-3.23420556730109,52.888916037398));
#11635=CARTESIAN_POINT('Ctrl Pts',(0.915978670843065,-3.26529773467149,
52.8828296356584));
#11636=CARTESIAN_POINT('Ctrl Pts',(0.81540897278163,-3.29185648606345,52.8767432339189));
#11637=CARTESIAN_POINT('Ctrl Pts',(0.713788528613445,-3.31374576558309,
52.8706568321793));
#11638=CARTESIAN_POINT('Ctrl Pts',(0.612204979229959,-3.33562709788047,
52.8645726401967));
#11639=CARTESIAN_POINT('Ctrl Pts',(0.50957185915237,-3.35284223795687,52.858488448214));
#11640=CARTESIAN_POINT('Ctrl Pts',(0.406352906602684,-3.3653056886107,52.8524042562314));
#11641=CARTESIAN_POINT('Ctrl Pts',(0.30314477287223,-3.37776783291704,52.8463207019589));
#11642=CARTESIAN_POINT('Ctrl Pts',(0.199351352903832,-3.38547922705865,
52.8402371476864));
#11643=CARTESIAN_POINT('Ctrl Pts',(0.0954430767543992,-3.38840606799121,
52.834153593414));
#11644=CARTESIAN_POINT('Ctrl Pts',(-0.00848114221444304,-3.39133335799384,
52.8280691057316));
#11645=CARTESIAN_POINT('Ctrl Pts',(-0.112519825311717,-3.38947462424989,
52.8219846180493));
#11646=CARTESIAN_POINT('Ctrl Pts',(-0.216201874215394,-3.38284818046654,
52.815900130367));
#11647=CARTESIAN_POINT('Ctrl Pts',(-0.319990816950072,-3.37621490497057,
52.8098093697164));
#11648=CARTESIAN_POINT('Ctrl Pts',(-0.423421964109565,-3.36480413073154,
52.8037186090659));
#11649=CARTESIAN_POINT('Ctrl Pts',(-0.52602871677517,-3.34868613811863,
52.7976278484153));
#11650=CARTESIAN_POINT('Ctrl Pts',(-0.628690992966425,-3.33255942358681,
52.7915337918754));
#11651=CARTESIAN_POINT('Ctrl Pts',(-0.730527567488587,-3.31172050241758,
52.7854397353355));
#11652=CARTESIAN_POINT('Ctrl Pts',(-0.831083360381304,-3.28629053958979,
52.7793456787956));
#11653=CARTESIAN_POINT('Ctrl Pts',(-0.93180029479501,-3.26081982502835,
52.7732418564778));
#11654=CARTESIAN_POINT('Ctrl Pts',(-1.0312319385576,-3.23074349611941,52.76713803416));
#11655=CARTESIAN_POINT('Ctrl Pts',(-1.12893947007988,-3.19623227181564,
52.7610342118422));
#11656=CARTESIAN_POINT('Ctrl Pts',(-1.20094087720445,-3.17080069379142,
52.7565362597511));
#11657=CARTESIAN_POINT('Ctrl Pts',(-1.2720063947445,-3.14296185816959,52.7520383076601));
#11658=CARTESIAN_POINT('Ctrl Pts',(-1.34196868650031,-3.11280020350691,
52.7475403555691));
#11659=CARTESIAN_POINT('Ctrl Pts',(-1.43692472241457,-3.07186342039838,
52.7414355283889));
#11660=CARTESIAN_POINT('Ctrl Pts',(-1.53016425998354,-3.02650945017575,
52.7353307012087));
#11661=CARTESIAN_POINT('Ctrl Pts',(-1.62124861941892,-2.97690409259893,
52.7292258740285));
#11662=CARTESIAN_POINT('Ctrl Pts',(-1.71221418254363,-2.92736343255642,
52.7231290090381));
#11663=CARTESIAN_POINT('Ctrl Pts',(-1.80102978379207,-2.87358261158481,
52.7170321440476));
#11664=CARTESIAN_POINT('Ctrl Pts',(-1.88727691443995,-2.81577536581348,
52.7109352790571));
#11665=CARTESIAN_POINT('Ctrl Pts',(-1.97343615605219,-2.75802702777677,
52.7048446269989));
#11666=CARTESIAN_POINT('Ctrl Pts',(-2.05703177887024,-2.69626066085924,
52.6987539749407));
#11667=CARTESIAN_POINT('Ctrl Pts',(-2.13767084953855,-2.63073533475588,
52.6926633228826));
#11668=CARTESIAN_POINT('Ctrl Pts',(-2.21825340047877,-2.56525593519387,
52.6865769397476));
#11669=CARTESIAN_POINT('Ctrl Pts',(-2.29588318959422,-2.4960230844489,52.6804905566126));
#11670=CARTESIAN_POINT('Ctrl Pts',(-2.37019788498121,-2.42333799717055,
52.6744041734776));
#11671=CARTESIAN_POINT('Ctrl Pts',(-2.44448559989363,-2.35067929872606,
52.6683200000469));
#11672=CARTESIAN_POINT('Ctrl Pts',(-2.51546030812431,-2.27457115324918,
52.6622358266163));
#11673=CARTESIAN_POINT('Ctrl Pts',(-2.5827948851974,-2.19535319333773,52.6561516531856));
#11674=CARTESIAN_POINT('Ctrl Pts',(-2.650122405451,-2.11614353565178,52.6500681173904));
#11675=CARTESIAN_POINT('Ctrl Pts',(-2.71381027655406,-2.03382503718923,
52.6439845815952));
#11676=CARTESIAN_POINT('Ctrl Pts',(-2.77357079996188,-1.94877142838734,
52.6379010458));
#11677=CARTESIAN_POINT('Ctrl Pts',(-2.83334049350506,-1.86370476827562,
52.6318165764981));
#11678=CARTESIAN_POINT('Ctrl Pts',(-2.88918139640564,-1.77590251354845,
52.6257321071963));
#11679=CARTESIAN_POINT('Ctrl Pts',(-2.94084891135973,-1.68576770139136,
52.6196476378944));
#11680=CARTESIAN_POINT('Ctrl Pts',(-2.992569696728,-1.59553995813859,52.6135568953627));
#11681=CARTESIAN_POINT('Ctrl Pts',(-3.04010828853447,-1.50297522617446,
52.6074661528309));
#11682=CARTESIAN_POINT('Ctrl Pts',(-3.08326591619373,-1.40850145634928,
52.6013754102991));
#11683=CARTESIAN_POINT('Ctrl Pts',(-3.12644689862605,-1.31397656199353,
52.5952813717588));
#11684=CARTESIAN_POINT('Ctrl Pts',(-3.16524203502955,-1.21754096830853,
52.5891873332185));
#11685=CARTESIAN_POINT('Ctrl Pts',(-3.19950135126218,-1.1196410879257,52.5830932946782));
#11686=CARTESIAN_POINT('Ctrl Pts',(-3.23381557061824,-1.0215843156429,52.5769894899841));
#11687=CARTESIAN_POINT('Ctrl Pts',(-3.26357932707888,-0.922058978611061,
52.5708856852901));
#11688=CARTESIAN_POINT('Ctrl Pts',(-3.28869294748947,-0.82152526414774,
52.564781880596));
#11689=CARTESIAN_POINT('Ctrl Pts',(-3.30720017078735,-0.7474379811468,52.5602837447401));
#11690=CARTESIAN_POINT('Ctrl Pts',(-3.3231830594563,-0.672803339565695,
52.5557856088842));
#11691=CARTESIAN_POINT('Ctrl Pts',(-3.33661973224267,-0.597807514931707,
52.5512874730284));
#11692=CARTESIAN_POINT('Ctrl Pts',(-3.36382438323819,-0.445966708228573,
52.5421802916573));
#11693=CARTESIAN_POINT('Ctrl Pts',(-3.38066933541319,-0.292218649893261,
52.5330731102862));
#11694=CARTESIAN_POINT('Ctrl Pts',(-3.38695150873708,-0.137711800378893,
52.5239659289151));
#11695=CARTESIAN_POINT('Ctrl Pts',(-3.38877905928926,-0.0927641264471587,
52.5213165536932));
#11696=CARTESIAN_POINT('Ctrl Pts',(-3.3897129670525,-0.0477524120291606,
52.5186671784714));
#11697=CARTESIAN_POINT('Ctrl Pts',(-3.38974892034748,-0.00270545801625161,
52.5160178032496));
#11698=CARTESIAN_POINT('Ctrl Pts',(-3.39152367512854,-0.00269060468911869,
52.5160168468642));
#11699=CARTESIAN_POINT('Ctrl Pts',(-3.39112041704622,0.0436611229947171,
52.5132921806742));
#11700=CARTESIAN_POINT('Ctrl Pts',(-3.38975319490166,0.090027953380886,
52.5105675144842));
#11701=CARTESIAN_POINT('Ctrl Pts',(-3.38743469189442,0.136371088936278,
52.5078428482942));
#11702=CARTESIAN_POINT('Origin',(0.,0.,0.));
#11703=CARTESIAN_POINT('',(-3.38700661857411,0.136349654327209,51.2580969930732));
#11704=CARTESIAN_POINT('',(-3.38700661379996,0.136349772919874,51.6005689639805));
#11705=CARTESIAN_POINT('',(-3.38700661857411,0.136349654327212,0.));
#11706=CARTESIAN_POINT('',(-3.38974867768107,0.00293645210927518,51.6091549103211));
#11707=CARTESIAN_POINT('Ctrl Pts',(-3.38700661379996,0.136349772919874,
51.6005689639805));
#11708=CARTESIAN_POINT('Ctrl Pts',(-3.38879548487887,0.0919131886429986,
51.6034319494006));
#11709=CARTESIAN_POINT('Ctrl Pts',(-3.38971017523789,0.0474336314538165,
51.6062961227749));
#11710=CARTESIAN_POINT('Ctrl Pts',(-3.38974872771026,0.00293691789115749,
51.6091549678441));
#11711=CARTESIAN_POINT('Ctrl Pts',(-3.3897487281089,0.00293645774800871,
51.6091549974076));
#11712=CARTESIAN_POINT('Ctrl Pts',(-3.38987105787604,-0.138276938860297,
51.6182277397316));
#11713=CARTESIAN_POINT('Ctrl Pts',(-3.38116912748961,-0.279373005641703,
51.627220309697));
#11714=CARTESIAN_POINT('Ctrl Pts',(-3.35498934500473,-0.489277272767235,
51.6403570728065));
#11715=CARTESIAN_POINT('Ctrl Pts',(-3.34412219774405,-0.558742803692446,
51.6446660030182));
#11716=CARTESIAN_POINT('Ctrl Pts',(-3.32233360665932,-0.674348489415988,
51.6517704980771));
#11717=CARTESIAN_POINT('Ctrl Pts',(-3.31259094933643,-0.720685797073671,
51.6546001506718));
#11718=CARTESIAN_POINT('Ctrl Pts',(-3.29399230171,-0.800771948080072,51.6594617774325));
#11719=CARTESIAN_POINT('Ctrl Pts',(-3.2855803465773,-0.834615430341658,
51.661507189113));
#11720=CARTESIAN_POINT('Ctrl Pts',(-3.26698882397763,-0.904771111174041,
51.6657304430639));
#11721=CARTESIAN_POINT('Ctrl Pts',(-3.25672250925341,-0.941055471628134,
51.6679052353609));
#11722=CARTESIAN_POINT('Ctrl Pts',(-3.22771751943565,-1.03740174388216,
51.6736594903687));
#11723=CARTESIAN_POINT('Ctrl Pts',(-3.20790823785293,-1.09712724215636,
51.6772048774853));
#11724=CARTESIAN_POINT('Ctrl Pts',(-3.09162758310946,-1.4175734352985,51.6961723481098));
#11725=CARTESIAN_POINT('Ctrl Pts',(-2.96503289569032,-1.66621028992737,
51.7105862441453));
#11726=CARTESIAN_POINT('Ctrl Pts',(-2.74119056567748,-1.99779507427186,
51.7320515705437));
#11727=CARTESIAN_POINT('Ctrl Pts',(-2.66746898058891,-2.0952123385526,51.7387002793221));
#11728=CARTESIAN_POINT('Ctrl Pts',(-2.56819260788787,-2.21264480834499,
51.7474422266867));
#11729=CARTESIAN_POINT('Ctrl Pts',(-2.54738534201585,-2.23656837253055,
51.7492639629333));
#11730=CARTESIAN_POINT('Ctrl Pts',(-2.51271320640104,-2.2753218130507,51.7522893685993));
#11731=CARTESIAN_POINT('Ctrl Pts',(-2.49904467132517,-2.2903258985071,51.7534795528178));
#11732=CARTESIAN_POINT('Ctrl Pts',(-2.47056773260371,-2.32102688021627,
51.7559561569881));
#11733=CARTESIAN_POINT('Ctrl Pts',(-2.45574283270985,-2.33670661075482,
51.7572436395464));
#11734=CARTESIAN_POINT('Ctrl Pts',(-2.41443092156084,-2.37957329127065,
51.7608237458737));
#11735=CARTESIAN_POINT('Ctrl Pts',(-2.38763612859452,-2.40645780837782,
51.7631372659178));
#11736=CARTESIAN_POINT('Ctrl Pts',(-2.18903673737211,-2.59913985968773,
51.7801861561247));
#11737=CARTESIAN_POINT('Ctrl Pts',(-2.00059975057804,-2.74681691735285,
51.7957827711509));
#11738=CARTESIAN_POINT('Ctrl Pts',(-1.66164816339618,-2.95893343004414,
51.8213726801498));
#11739=CARTESIAN_POINT('Ctrl Pts',(-1.51914391289128,-3.0345632536054,51.831519559208));
#11740=CARTESIAN_POINT('Ctrl Pts',(-1.31982432293415,-3.12277080624156,
51.8448001997358));
#11741=CARTESIAN_POINT('Ctrl Pts',(-1.26729142258515,-3.14445651569493,
51.8482210557487));
#11742=CARTESIAN_POINT('Ctrl Pts',(-1.18012874384436,-3.17789800519564,
51.8537704955256));
#11743=CARTESIAN_POINT('Ctrl Pts',(-1.14581154357527,-3.19043188999231,
51.8559239524696));
#11744=CARTESIAN_POINT('Ctrl Pts',(-1.0781699104516,-3.21390483573051,51.8601093696363));
#11745=CARTESIAN_POINT('Ctrl Pts',(-1.04486517558037,-3.22488628435555,
51.862142479027));
#11746=CARTESIAN_POINT('Ctrl Pts',(-0.962949469430438,-3.25049376513832,
51.8670789974797));
#11747=CARTESIAN_POINT('Ctrl Pts',(-0.914168151969811,-3.26454872292996,
51.8699640671037));
#11748=CARTESIAN_POINT('Ctrl Pts',(-0.712492115176322,-3.31778054074508,
51.8816915375638));
#11749=CARTESIAN_POINT('Ctrl Pts',(-0.557262906336512,-3.34735383324367,
51.8902385934743));
#11750=CARTESIAN_POINT('Ctrl Pts',(-0.243918895803178,-3.38463903569707,
51.9070900918788));
#11751=CARTESIAN_POINT('Ctrl Pts',(-0.0862073925304647,-3.39232132574715,
51.9153757928337));
#11752=CARTESIAN_POINT('Ctrl Pts',(0.181882681816868,-3.38666826602269,
51.9298176140896));
#11753=CARTESIAN_POINT('Ctrl Pts',(0.292114723578123,-3.37894481550556,
51.935862044089));
#11754=CARTESIAN_POINT('Ctrl Pts',(0.432523396443501,-3.36218504322535,
51.9439091654905));
#11755=CARTESIAN_POINT('Ctrl Pts',(0.46323098688419,-3.35809196749698,51.9456906663847));
#11756=CARTESIAN_POINT('Ctrl Pts',(0.513824118068741,-3.3506411856894,51.9486677754617));
#11757=CARTESIAN_POINT('Ctrl Pts',(0.533744310745238,-3.34752573918671,
51.9498507795762));
#11758=CARTESIAN_POINT('Ctrl Pts',(0.575157259635956,-3.34066985373146,
51.9523347141267));
#11759=CARTESIAN_POINT('Ctrl Pts',(0.596643535394793,-3.33689936618805,
51.9536370463206));
#11760=CARTESIAN_POINT('Ctrl Pts',(0.65654546626964,-3.3257905367248,51.9573030423094));
#11761=CARTESIAN_POINT('Ctrl Pts',(0.694871642469487,-3.31799453956417,
51.9596891766464));
#11762=CARTESIAN_POINT('Ctrl Pts',(0.959525996132115,-3.25937440210863,
51.9764093468088));
#11763=CARTESIAN_POINT('Ctrl Pts',(1.18024131676789,-3.18610021009077,51.9915450678248));
#11764=CARTESIAN_POINT('Ctrl Pts',(1.55387646790826,-3.01786223221083,52.0177892658091));
#11765=CARTESIAN_POINT('Ctrl Pts',(1.71003755733788,-2.93220237788336,52.0289828493556));
#11766=CARTESIAN_POINT('Ctrl Pts',(1.90158604219653,-2.80659878090064,52.042869699458));
#11767=CARTESIAN_POINT('Ctrl Pts',(1.94375952304615,-2.77755747623924,52.0459394768243));
#11768=CARTESIAN_POINT('Ctrl Pts',(2.0140289994769,-2.72678417667402,52.0510780116933));
#11769=CARTESIAN_POINT('Ctrl Pts',(2.04246979922072,-2.70554652845264,52.0531646428357));
#11770=CARTESIAN_POINT('Ctrl Pts',(2.09947172719957,-2.66157016984409,52.0573629060216));
#11771=CARTESIAN_POINT('Ctrl Pts',(2.12800960088497,-2.63880893397884,52.0594732872653));
#11772=CARTESIAN_POINT('Ctrl Pts',(2.19989804813751,-2.57954733420765,52.0648155652048));
#11773=CARTESIAN_POINT('Ctrl Pts',(2.24271194414063,-2.54241214585397,52.0680220632045));
#11774=CARTESIAN_POINT('Ctrl Pts',(2.49019708357747,-2.31663371880594,52.0867557271232));
#11775=CARTESIAN_POINT('Ctrl Pts',(2.67192516132004,-2.10444631676261,52.1012322733145));
#11776=CARTESIAN_POINT('Ctrl Pts',(2.87556365369532,-1.79713549656603,52.1209561951511));
#11777=CARTESIAN_POINT('Ctrl Pts',(2.92242166496743,-1.71988727619846,52.1258343055489));
#11778=CARTESIAN_POINT('Ctrl Pts',(2.99429611797371,-1.5899622129895,52.1340551747531));
#11779=CARTESIAN_POINT('Ctrl Pts',(3.02113878404768,-1.53834610481194,52.1373253574219));
#11780=CARTESIAN_POINT('Ctrl Pts',(3.05771914351488,-1.46335147061405,52.1421183023096));
#11781=CARTESIAN_POINT('Ctrl Pts',(3.06854492988605,-1.44051234551156,52.1435833770792));
#11782=CARTESIAN_POINT('Ctrl Pts',(3.08726264045479,-1.39985504342026,52.146204637741));
#11783=CARTESIAN_POINT('Ctrl Pts',(3.09525793954078,-1.38208646628821,52.1473548265244));
#11784=CARTESIAN_POINT('Ctrl Pts',(3.11321275499186,-1.34124673581127,52.1500092555031));
#11785=CARTESIAN_POINT('Ctrl Pts',(3.12306931595686,-1.31813293291421,52.15151903168));
#11786=CARTESIAN_POINT('Ctrl Pts',(3.15369329506298,-1.24404703755062,52.1563770912907));
#11787=CARTESIAN_POINT('Ctrl Pts',(3.17347576003551,-1.19267989577675,52.1597735038214));
#11788=CARTESIAN_POINT('Ctrl Pts',(3.26690727779489,-0.931268360590284,
52.1771214028011));
#11789=CARTESIAN_POINT('Ctrl Pts',(3.32099067256739,-0.714816893078074,
52.1916474391223));
#11790=CARTESIAN_POINT('Ctrl Pts',(3.37724086001234,-0.33345442658512,52.2162658669266));
#11791=CARTESIAN_POINT('Ctrl Pts',(3.38936579170606,-0.170759440167206,
52.2264812983484));
#11792=CARTESIAN_POINT('Ctrl Pts',(3.38985704326271,0.0425848775897024,
52.2394055452134));
#11793=CARTESIAN_POINT('Ctrl Pts',(3.38884945476204,0.0929732405482049,
52.2424250329519));
#11794=CARTESIAN_POINT('Ctrl Pts',(3.38522394881534,0.178644149332612,52.2475051475909));
#11795=CARTESIAN_POINT('Ctrl Pts',(3.3831766467966,0.213941188261571,52.2495826975655));
#11796=CARTESIAN_POINT('Ctrl Pts',(3.37787884403524,0.285809479566358,52.2537832812902));
#11797=CARTESIAN_POINT('Ctrl Pts',(3.3745856624859,0.322372923341972,52.2559047254914));
#11798=CARTESIAN_POINT('Ctrl Pts',(3.36458496562479,0.416303061115712,52.2613185614779));
#11799=CARTESIAN_POINT('Ctrl Pts',(3.35700403925316,0.473565887704233,52.264584111905));
#11800=CARTESIAN_POINT('Ctrl Pts',(3.3052905989075,0.79985990430415,52.283041720845));
#11801=CARTESIAN_POINT('Ctrl Pts',(3.23029727614805,1.06297081266451,52.2972392750651));
#11802=CARTESIAN_POINT('Ctrl Pts',(3.08872379539329,1.39955389326863,52.3167603660537));
#11803=CARTESIAN_POINT('Ctrl Pts',(3.04937543608565,1.48333187692974,52.3217521768385));
#11804=CARTESIAN_POINT('Ctrl Pts',(2.97936203090318,1.61780689506126,52.3301404461206));
#11805=CARTESIAN_POINT('Ctrl Pts',(2.95070752615989,1.66949738903029,52.3334605314602));
#11806=CARTESIAN_POINT('Ctrl Pts',(2.90781690297534,1.74231228803539,52.3383134502885));
#11807=CARTESIAN_POINT('Ctrl Pts',(2.89466975283893,1.76406864608762,52.3397865886549));
#11808=CARTESIAN_POINT('Ctrl Pts',(2.87101396405339,1.8022385065597,52.3424159466096));
#11809=CARTESIAN_POINT('Ctrl Pts',(2.86060648159784,1.81871254861502,52.3435659984875));
#11810=CARTESIAN_POINT('Ctrl Pts',(2.83652960922569,1.85610593422345,52.3462117221215));
#11811=CARTESIAN_POINT('Ctrl Pts',(2.82277048245854,1.87696461997163,52.3477127650335));
#11812=CARTESIAN_POINT('Ctrl Pts',(2.77721730143225,1.94438892006352,52.3526425717778));
#11813=CARTESIAN_POINT('Ctrl Pts',(2.74449314205261,1.99031174862924,52.3561227195155));
#11814=CARTESIAN_POINT('Ctrl Pts',(2.57743683899233,2.21278936472214,52.3735162069105));
#11815=CARTESIAN_POINT('Ctrl Pts',(2.42714402196589,2.37667578195511,52.3879932241919));
#11816=CARTESIAN_POINT('Ctrl Pts',(2.140731632253,2.63327709480896,52.41255038668));
#11817=CARTESIAN_POINT('Ctrl Pts',(2.01187126753199,2.73299574038936,52.4227522423883));
#11818=CARTESIAN_POINT('Ctrl Pts',(1.83437461242483,2.85096698845879,52.4356630076093));
#11819=CARTESIAN_POINT('Ctrl Pts',(1.7918005229941,2.87791491855263,52.4386817164428));
#11820=CARTESIAN_POINT('Ctrl Pts',(1.71835510809195,2.92214142648197,52.4437609514644));
#11821=CARTESIAN_POINT('Ctrl Pts',(1.6877861928792,2.93990351894607,52.4458383854721));
#11822=CARTESIAN_POINT('Ctrl Pts',(1.62491675438216,2.97512997878435,52.4500390839158));
#11823=CARTESIAN_POINT('Ctrl Pts',(1.5925991082126,2.99255427377152,52.4521607530354));
#11824=CARTESIAN_POINT('Ctrl Pts',(1.50871453160159,3.03603738002926,52.4575759155834));
#11825=CARTESIAN_POINT('Ctrl Pts',(1.45675205264521,3.06130960674944,52.4608425419491));
#11826=CARTESIAN_POINT('Ctrl Pts',(1.15614185747562,3.19812441646148,52.4792950249874));
#11827=CARTESIAN_POINT('Ctrl Pts',(0.895419301129158,3.28068494276031,52.4934874155788));
#11828=CARTESIAN_POINT('Ctrl Pts',(0.493959466364551,3.35632348972954,52.5153272777128));
#11829=CARTESIAN_POINT('Ctrl Pts',(0.358920374819451,3.37343629959095,52.5226924495569));
#11830=CARTESIAN_POINT('Ctrl Pts',(0.190916675886263,3.38452430683381,52.5322553231149));
#11831=CARTESIAN_POINT('Ctrl Pts',(0.158572621835733,3.38619381042795,52.5341147485072));
#11832=CARTESIAN_POINT('Ctrl Pts',(0.105795509761141,3.38816022922224,52.5371858608962));
#11833=CARTESIAN_POINT('Ctrl Pts',(0.0853740264588072,3.38873629529908,
52.5383832303929));
#11834=CARTESIAN_POINT('Ctrl Pts',(0.0435717885324079,3.38953738855444,
52.540854871851));
#11835=CARTESIAN_POINT('Ctrl Pts',(0.0221919479965969,3.38974477992475,
52.542129911089));
#11836=CARTESIAN_POINT('Ctrl Pts',(-0.0361875206390548,3.38975876814832,
52.5456387085442));
#11837=CARTESIAN_POINT('Ctrl Pts',(-0.0731833303047075,3.38916184372154,
52.5478920926298));
#11838=CARTESIAN_POINT('Ctrl Pts',(-0.316538787699377,3.38124908538498,
52.5628794440812));
#11839=CARTESIAN_POINT('Ctrl Pts',(-0.521859338970512,3.35569592859384,
52.5762760873013));
#11840=CARTESIAN_POINT('Ctrl Pts',(-0.920842547156187,3.26852116135418,
52.6025258227099));
#11841=CARTESIAN_POINT('Ctrl Pts',(-1.11389786101519,3.20787058003291,52.6153281811723));
#11842=CARTESIAN_POINT('Ctrl Pts',(-1.34984712358641,3.10985237075649,52.6308513326477));
#11843=CARTESIAN_POINT('Ctrl Pts',(-1.39877715367245,3.08815349085226,52.6340657641505));
#11844=CARTESIAN_POINT('Ctrl Pts',(-1.47964648362908,3.04997389471161,52.6393731063393));
#11845=CARTESIAN_POINT('Ctrl Pts',(-1.51187317492557,3.0341282313925,52.6414866958907));
#11846=CARTESIAN_POINT('Ctrl Pts',(-1.57589042752171,3.00137805996543,52.6456845056885));
#11847=CARTESIAN_POINT('Ctrl Pts',(-1.60767555491014,2.98447321182746,52.6477683678868));
#11848=CARTESIAN_POINT('Ctrl Pts',(-1.68645263251289,2.94095198307756,52.6529358224508));
#11849=CARTESIAN_POINT('Ctrl Pts',(-1.73308992255605,2.91371254872916,52.6559974383317));
#11850=CARTESIAN_POINT('Ctrl Pts',(-2.0274189979257,2.73223540059595,52.6753792958114));
#11851=CARTESIAN_POINT('Ctrl Pts',(-2.25495812588372,2.54768627066783,52.6905086998192));
#11852=CARTESIAN_POINT('Ctrl Pts',(-2.54257924458769,2.24531838466659,52.7128777053626));
#11853=CARTESIAN_POINT('Ctrl Pts',(-2.62397250391029,2.14963401706148,52.7197043680379));
#11854=CARTESIAN_POINT('Ctrl Pts',(-2.71914997230546,2.02426423880615,52.7286505082782));
#11855=CARTESIAN_POINT('Ctrl Pts',(-2.73807489114561,1.99859150779091,52.7304826618189));
#11856=CARTESIAN_POINT('Ctrl Pts',(-2.76846702437069,1.95612086719505,52.733520709445));
#11857=CARTESIAN_POINT('Ctrl Pts',(-2.78015081454608,1.93947929588414,52.7347128908033));
#11858=CARTESIAN_POINT('Ctrl Pts',(-2.80389203030473,1.90500859873086,52.7371880418936));
#11859=CARTESIAN_POINT('Ctrl Pts',(-2.81593055365271,1.88716807447398,52.738471990852));
#11860=CARTESIAN_POINT('Ctrl Pts',(-2.84857845315503,1.83777745739272,52.7420318516036));
#11861=CARTESIAN_POINT('Ctrl Pts',(-2.86883229941964,1.80599727907717,52.7443282963346));
#11862=CARTESIAN_POINT('Ctrl Pts',(-2.99142721624258,1.60636698104816,52.7587583953573));
#11863=CARTESIAN_POINT('Ctrl Pts',(-3.07952865630849,1.43022564660035,52.7714880063254));
#11864=CARTESIAN_POINT('Ctrl Pts',(-3.20427716363135,1.11503194436916,52.7932909347465));
#11865=CARTESIAN_POINT('Ctrl Pts',(-3.24829444849369,0.979426934267012,
52.8023896652377));
#11866=CARTESIAN_POINT('Ctrl Pts',(-3.30688705398011,0.750775642305356,
52.8171100024576));
#11867=CARTESIAN_POINT('Ctrl Pts',(-3.32635768508744,0.659176045620381,
52.82285006368));
#11868=CARTESIAN_POINT('Ctrl Pts',(-3.34922340952981,0.524372559918057,
52.8310667186017));
#11869=CARTESIAN_POINT('Ctrl Pts',(-3.35562237123423,0.481728953830529,
52.8336329966302));
#11870=CARTESIAN_POINT('Ctrl Pts',(-3.36566231985887,0.404853358648766,
52.8382024921641));
#11871=CARTESIAN_POINT('Ctrl Pts',(-3.36959871261343,0.370666612059013,
52.8402144915192));
#11872=CARTESIAN_POINT('Ctrl Pts',(-3.37698490169864,0.296612286757205,
52.844531814897));
#11873=CARTESIAN_POINT('Ctrl Pts',(-3.38025074163482,0.256731360692908,
52.8468312412225));
#11874=CARTESIAN_POINT('Ctrl Pts',(-3.38452747924999,0.190000076920932,
52.8506399303389));
#11875=CARTESIAN_POINT('Ctrl Pts',(-3.38592647032564,0.163181179021443,
52.8521601726888));
#11876=CARTESIAN_POINT('Ctrl Pts',(-3.3870066183502,0.136349659889395,52.8536715661706));
#11877=CARTESIAN_POINT('',(-3.38581326799137,0.000818680359414605,51.2660178032496));
#11878=CARTESIAN_POINT('Ctrl Pts',(-3.38743469189442,0.136371088936278,
52.5078428482942));
#11879=CARTESIAN_POINT('Ctrl Pts',(-3.34409159582951,1.00272967033552,52.4569067623586));
#11880=CARTESIAN_POINT('Ctrl Pts',(-2.48565222001799,2.96284343806158,52.3405530489097));
#11881=CARTESIAN_POINT('Ctrl Pts',(0.890051795839941,3.89117902226943,52.158781707947));
#11882=CARTESIAN_POINT('Ctrl Pts',(3.73656515455507,1.40411381468714,51.9625288254065));
#11883=CARTESIAN_POINT('Ctrl Pts',(3.23236205304029,-2.34203796083313,51.7662759428657));
#11884=CARTESIAN_POINT('Ctrl Pts',(-0.170370382920846,-3.98806386008981,
51.5700230603252));
#11885=CARTESIAN_POINT('Ctrl Pts',(-2.93186071344323,-2.34791161761635,
51.4032703471197));
#11886=CARTESIAN_POINT('Ctrl Pts',(-3.3833120129129,-0.613321193095971,
51.3019352614279));
#11887=CARTESIAN_POINT('Ctrl Pts',(-3.38470792471488,0.000818413090442893,
51.2660178032496));
#11888=CARTESIAN_POINT('Ctrl Pts',(-3.38974990090759,0.000819632226453476,
51.2660178032496));
#11889=CARTESIAN_POINT('Ctrl Pts',(-3.38973896871118,0.0460318755858765,
51.2633775331908));
#11890=CARTESIAN_POINT('Ctrl Pts',(-3.38882336922471,0.0912204861733642,
51.260737263132));
#11891=CARTESIAN_POINT('Ctrl Pts',(-3.38700661857411,0.136349654327206,
51.2580969930732));
#11892=CARTESIAN_POINT('Origin',(0.,0.,0.));
#11893=CARTESIAN_POINT('',(-3.38700661857411,0.136349654327212,28.));
#11894=CARTESIAN_POINT('Origin',(0.,0.,28.));
#11895=CARTESIAN_POINT('',(-3.38700661857411,0.136349654327212,50.));
#11896=CARTESIAN_POINT('',(-3.38700661857411,0.136349654327212,0.));
#11897=CARTESIAN_POINT('',(0.786086670334145,3.30023142332346,49.9983683068078));
#11898=CARTESIAN_POINT('Origin',(0.,0.,50.));
#11899=CARTESIAN_POINT('',(-3.38700661811317,0.13634966577722,50.3495735854002));
#11900=CARTESIAN_POINT('Ctrl Pts',(0.785310170844009,3.29752831649236,49.9967568224334));
#11901=CARTESIAN_POINT('Ctrl Pts',(0.746609307942668,3.30674497161701,49.9991821184928));
#11902=CARTESIAN_POINT('Ctrl Pts',(0.707750531259817,3.31527928317419,50.0016377255565));
#11903=CARTESIAN_POINT('Ctrl Pts',(0.450743211555314,3.36699988893547,50.0179748958375));
#11904=CARTESIAN_POINT('Ctrl Pts',(0.228953455097597,3.38931182096382,50.0324855428879));
#11905=CARTESIAN_POINT('Ctrl Pts',(-0.164263402961797,3.39007534803615,
50.0576378042822));
#11906=CARTESIAN_POINT('Ctrl Pts',(-0.334906605078102,3.37749079198311,
50.068370160301));
#11907=CARTESIAN_POINT('Ctrl Pts',(-0.55462065489123,3.34446296323699,50.0818357627315));
#11908=CARTESIAN_POINT('Ctrl Pts',(-0.605171315982537,3.33568653873055,
50.0849107259738));
#11909=CARTESIAN_POINT('Ctrl Pts',(-0.690689456111278,3.31883099074862,
50.0900761579914));
#11910=CARTESIAN_POINT('Ctrl Pts',(-0.725762169369974,3.31133817171354,
50.0921840802752));
#11911=CARTESIAN_POINT('Ctrl Pts',(-0.792631465371682,3.29593892778624,
50.0961849703029));
#11912=CARTESIAN_POINT('Ctrl Pts',(-0.824445060020095,3.2881253785261,50.0980805306922));
#11913=CARTESIAN_POINT('Ctrl Pts',(-0.908676532223715,3.2661383983955,50.1030814135789));
#11914=CARTESIAN_POINT('Ctrl Pts',(-0.960876609895461,3.25116435510229,
50.1061618659434));
#11915=CARTESIAN_POINT('Ctrl Pts',(-1.25430335787979,3.15930730586294,50.1234120561698));
#11916=CARTESIAN_POINT('Ctrl Pts',(-1.48667388182259,3.05684627039881,50.1367440097761));
#11917=CARTESIAN_POINT('Ctrl Pts',(-1.83576854494666,2.85360953247586,50.158354616456));
#11918=CARTESIAN_POINT('Ctrl Pts',(-1.96083938456098,2.7691575803534,50.1664915251561));
#11919=CARTESIAN_POINT('Ctrl Pts',(-2.10605221950588,2.6563224939898,50.176937725591));
#11920=CARTESIAN_POINT('Ctrl Pts',(-2.1319413911594,2.63558928487613,50.1788419978037));
#11921=CARTESIAN_POINT('Ctrl Pts',(-2.17363187534116,2.60118546863107,50.1819851336088));
#11922=CARTESIAN_POINT('Ctrl Pts',(-2.18961895312857,2.58774229155763,50.1832093048278));
#11923=CARTESIAN_POINT('Ctrl Pts',(-2.22194733711898,2.56004400476953,50.1857258995685));
#11924=CARTESIAN_POINT('Ctrl Pts',(-2.23827807376954,2.54577816874297,50.1870190523104));
#11925=CARTESIAN_POINT('Ctrl Pts',(-2.28276116009191,2.50616076360308,50.1905993904282));
#11926=CARTESIAN_POINT('Ctrl Pts',(-2.31062637683867,2.48049305170421,50.192907109681));
#11927=CARTESIAN_POINT('Ctrl Pts',(-2.47841443459673,2.32065635129221,50.2071749376582));
#11928=CARTESIAN_POINT('Ctrl Pts',(-2.60703696249065,2.17516273276916,50.2197089895251));
#11929=CARTESIAN_POINT('Ctrl Pts',(-2.84994425392242,1.84769433054061,50.2459143137803));
#11930=CARTESIAN_POINT('Ctrl Pts',(-2.96084551142556,1.66420383069609,50.2594969096643));
#11931=CARTESIAN_POINT('Ctrl Pts',(-3.07657251474616,1.42403581738916,50.275678802049));
#11932=CARTESIAN_POINT('Ctrl Pts',(-3.0983177787475,1.37608279090161,50.2788385498945));
#11933=CARTESIAN_POINT('Ctrl Pts',(-3.13299025812217,1.29462903260921,50.2840898257772));
#11934=CARTESIAN_POINT('Ctrl Pts',(-3.14651771998916,1.26139552590942,50.28620072154));
#11935=CARTESIAN_POINT('Ctrl Pts',(-3.172707477592,1.19400941833025,50.2904196061501));
#11936=CARTESIAN_POINT('Ctrl Pts',(-3.18535205776579,1.15985501045487,50.2925267965072));
#11937=CARTESIAN_POINT('Ctrl Pts',(-3.21589060270197,1.07309794581504,50.297805099226));
#11938=CARTESIAN_POINT('Ctrl Pts',(-3.23304658937067,1.02024595286799,50.3009524651739));
#11939=CARTESIAN_POINT('Ctrl Pts',(-3.3293154233636,0.696802911808041,50.3198491292813));
#11940=CARTESIAN_POINT('Ctrl Pts',(-3.37567739213672,0.417774362651803,
50.3345047438463));
#11941=CARTESIAN_POINT('Ctrl Pts',(-3.38700661811317,0.136349665777316,
50.3495735854002));
#11942=CARTESIAN_POINT('',(-3.38700661857411,0.136349654327281,50.0079012193304));
#11943=CARTESIAN_POINT('',(-3.38700661857411,0.136349654327212,0.));
#11944=CARTESIAN_POINT('',(-3.3787688286016,0.272628438300507,50.));
#11945=CARTESIAN_POINT('Ctrl Pts',(-3.38700661857411,0.136349654327351,
50.0079012193304));
#11946=CARTESIAN_POINT('Ctrl Pts',(-3.38700507140738,0.136388086870375,
50.0078990226929));
#11947=CARTESIAN_POINT('Ctrl Pts',(-3.3870035235907,0.13642651938927,50.0078968260301));
#11948=CARTESIAN_POINT('Ctrl Pts',(-3.38597226724431,0.16202186261079,50.0064338749809));
#11949=CARTESIAN_POINT('Ctrl Pts',(-3.38465335442818,0.187565683441125,
50.004963170781));
#11950=CARTESIAN_POINT('Ctrl Pts',(-3.38179470016056,0.232949742603296,
50.0023277969806));
#11951=CARTESIAN_POINT('Ctrl Pts',(-3.38036906961303,0.252796154913672,
50.0011677352365));
#11952=CARTESIAN_POINT('Ctrl Pts',(-3.3787688286016,0.272628438300507,50.));
#11953=CARTESIAN_POINT('Origin',(0.,0.,50.));
#11954=CARTESIAN_POINT('Origin',(0.,0.,0.));
#11955=CARTESIAN_POINT('Ctrl Pts',(-3.38700661811317,0.136349665777316,
50.3495735854002));
#11956=CARTESIAN_POINT('Ctrl Pts',(-3.38826066203953,0.105198470402101,
50.3512415713039));
#11957=CARTESIAN_POINT('Ctrl Pts',(-3.38908543079459,0.0740179861142426,
50.3529159549153));
#11958=CARTESIAN_POINT('Ctrl Pts',(-3.39081429351722,-0.0628422592113099,
50.3603018318282));
#11959=CARTESIAN_POINT('Ctrl Pts',(-3.38720763024682,-0.168497659618867,
50.3660982382046));
#11960=CARTESIAN_POINT('Ctrl Pts',(-3.37619544593572,-0.304386056493696,
50.373861742131));
#11961=CARTESIAN_POINT('Ctrl Pts',(-3.37330194467216,-0.334933441996331,
50.3756272594484));
#11962=CARTESIAN_POINT('Ctrl Pts',(-3.36782519952948,-0.385439113149716,
50.3785860061352));
#11963=CARTESIAN_POINT('Ctrl Pts',(-3.36547810227512,-0.40542201413453,
50.379767007702));
#11964=CARTESIAN_POINT('Ctrl Pts',(-3.36021440736446,-0.447035271618782,
50.3822500003375));
#11965=CARTESIAN_POINT('Ctrl Pts',(-3.35726658392158,-0.468660244976085,
50.3835534758816));
#11966=CARTESIAN_POINT('Ctrl Pts',(-3.34840228581628,-0.529305945517847,
50.3872430989558));
#11967=CARTESIAN_POINT('Ctrl Pts',(-3.34201302111642,-0.568252875777798,
50.3896523595134));
#11968=CARTESIAN_POINT('Ctrl Pts',(-3.30855473415173,-0.752054058905714,
50.4011835604538));
#11969=CARTESIAN_POINT('Ctrl Pts',(-3.27274021625441,-0.89514515717768,
50.410630314275));
#11970=CARTESIAN_POINT('Ctrl Pts',(-3.18548424477249,-1.16714446052443,
50.4290184106722));
#11971=CARTESIAN_POINT('Ctrl Pts',(-3.1352109698773,-1.29614479781498,50.4379383500371));
#11972=CARTESIAN_POINT('Ctrl Pts',(-3.02218025575127,-1.54079100775359,
50.4550073729889));
#11973=CARTESIAN_POINT('Ctrl Pts',(-2.96029622936766,-1.65658174036465,
50.4631587199742));
#11974=CARTESIAN_POINT('Ctrl Pts',(-2.86697385484724,-1.80918196803392,
50.4739670805158));
#11975=CARTESIAN_POINT('Ctrl Pts',(-2.84124164526892,-1.84933088892586,
50.4768181048648));
#11976=CARTESIAN_POINT('Ctrl Pts',(-2.79530057353443,-1.91778725608769,
50.4816945537671));
#11977=CARTESIAN_POINT('Ctrl Pts',(-2.77548791473621,-1.9463504886227,50.4837340295698));
#11978=CARTESIAN_POINT('Ctrl Pts',(-2.73354588082854,-2.0048737562823,50.4879248308165));
#11979=CARTESIAN_POINT('Ctrl Pts',(-2.71135498647931,-2.03478405662866,
50.4900734629393));
#11980=CARTESIAN_POINT('Ctrl Pts',(-2.6513849743876,-2.11289190962338,50.4957071611048));
#11981=CARTESIAN_POINT('Ctrl Pts',(-2.61278428946314,-2.16044287131503,
50.4991602394588));
#11982=CARTESIAN_POINT('Ctrl Pts',(-2.38981729272071,-2.42038614954167,
50.5182304973037));
#11983=CARTESIAN_POINT('Ctrl Pts',(-2.18087778385413,-2.61022403431013,
50.5327939180363));
#11984=CARTESIAN_POINT('Ctrl Pts',(-1.84993923394252,-2.8431264978651,50.554479288014));
#11985=CARTESIAN_POINT('Ctrl Pts',(-1.74519218241375,-2.90859796609916,
50.561193826104));
#11986=CARTESIAN_POINT('Ctrl Pts',(-1.60938415877447,-2.98350313292404,
50.5700078218592));
#11987=CARTESIAN_POINT('Ctrl Pts',(-1.58143696372896,-2.9984104606419,50.5718272254527));
#11988=CARTESIAN_POINT('Ctrl Pts',(-1.53531976546108,-3.02218577522506,
50.574845319316));
#11989=CARTESIAN_POINT('Ctrl Pts',(-1.51727126047909,-3.03128711080798,
50.576030414953));
#11990=CARTESIAN_POINT('Ctrl Pts',(-1.47985237606117,-3.04973844694305,
50.578497472976));
#11991=CARTESIAN_POINT('Ctrl Pts',(-1.46047271870659,-3.05906636625982,
50.5797804739509));
#11992=CARTESIAN_POINT('Ctrl Pts',(-1.40697689140364,-3.08419106254895,
50.5833338797222));
#11993=CARTESIAN_POINT('Ctrl Pts',(-1.37268554107248,-3.09960523902601,
50.5856246911011));
#11994=CARTESIAN_POINT('Ctrl Pts',(-1.15515967672149,-3.19306698094872,
50.6002063756298));
#11995=CARTESIAN_POINT('Ctrl Pts',(-0.965611784236614,-3.25540395352576,
50.6131093194901));
#11996=CARTESIAN_POINT('Ctrl Pts',(-0.568419468426531,-3.34826631767495,
50.6393410156936));
#11997=CARTESIAN_POINT('Ctrl Pts',(-0.361154943105755,-3.37691836337358,
50.6525951834277));
#11998=CARTESIAN_POINT('Ctrl Pts',(-0.0991440327766787,-3.3887214725872,
50.6685283423939));
#11999=CARTESIAN_POINT('Ctrl Pts',(-0.0456892563724606,-3.38986367444856,
50.6717389621893));
#12000=CARTESIAN_POINT('Ctrl Pts',(0.0437213682890569,-3.38965865990238,
50.6770449215391));
#12001=CARTESIAN_POINT('Ctrl Pts',(0.0796675943391308,-3.38900436853749,
50.6791607816298));
#12002=CARTESIAN_POINT('Ctrl Pts',(0.151682358896865,-3.38654708304739,
50.6833670669487));
#12003=CARTESIAN_POINT('Ctrl Pts',(0.187746023543892,-3.38473931918434,
50.6854570670065));
#12004=CARTESIAN_POINT('Ctrl Pts',(0.277968228511519,-3.37877026334543,
50.6906483448547));
#12005=CARTESIAN_POINT('Ctrl Pts',(0.33206941547825,-3.37388280555407,50.6937273556445));
#12006=CARTESIAN_POINT('Ctrl Pts',(0.64479091464955,-3.3380362042881,50.7113691915576));
#12007=CARTESIAN_POINT('Ctrl Pts',(0.899265220823585,-3.27865405311346,
50.7250211358607));
#12008=CARTESIAN_POINT('Ctrl Pts',(1.277081441481,-3.14313928076725,50.7464212444358));
#12009=CARTESIAN_POINT('Ctrl Pts',(1.40661389866871,-3.08734384367361,50.7540014877076));
#12010=CARTESIAN_POINT('Ctrl Pts',(1.56737206255776,-3.0058770775312,50.7641535609055));
#12011=CARTESIAN_POINT('Ctrl Pts',(1.60214388454224,-2.98748839098475,50.7663964741347));
#12012=CARTESIAN_POINT('Ctrl Pts',(1.65576673136436,-2.95792516865605,50.7699412553557));
#12013=CARTESIAN_POINT('Ctrl Pts',(1.67484366845317,-2.94716531636127,50.7712196291253));
#12014=CARTESIAN_POINT('Ctrl Pts',(1.7110949170622,-2.92625310504677,50.7736846367434));
#12015=CARTESIAN_POINT('Ctrl Pts',(1.72828612390148,-2.91613272148169,50.7748694119276));
#12016=CARTESIAN_POINT('Ctrl Pts',(1.77177397041937,-2.89001203745366,50.7779052089944));
#12017=CARTESIAN_POINT('Ctrl Pts',(1.79794350702348,-2.87380437391669,50.779768411163));
#12018=CARTESIAN_POINT('Ctrl Pts',(1.90812396471953,-2.8034719720309,50.787756853726));
#12019=CARTESIAN_POINT('Ctrl Pts',(1.98993481732703,-2.74600590434541,50.7940474610914));
#12020=CARTESIAN_POINT('Ctrl Pts',(2.07941931980257,-2.67704887957704,50.8012488981733));
#12021=CARTESIAN_POINT('Ctrl Pts',(2.08971144788955,-2.66902256861067,50.8020822044132));
#12022=CARTESIAN_POINT('Ctrl Pts',(2.33920773840247,-2.47212521838049,50.8224016295563));
#12023=CARTESIAN_POINT('Ctrl Pts',(2.55195419033199,-2.25186314665627,50.8422233236295));
#12024=CARTESIAN_POINT('Ctrl Pts',(2.7648108471223,-1.96194483195287,50.8640996161308));
#12025=CARTESIAN_POINT('Ctrl Pts',(2.79615982948518,-1.91700215701818,50.86739329103));
#12026=CARTESIAN_POINT('Ctrl Pts',(2.84636576997775,-1.84117192589998,50.8727940353639));
#12027=CARTESIAN_POINT('Ctrl Pts',(2.86584150458879,-1.81070836345626,50.8749233459621));
#12028=CARTESIAN_POINT('Ctrl Pts',(2.90362010169414,-1.74947887278681,50.8791256913018));
#12029=CARTESIAN_POINT('Ctrl Pts',(2.92193038749412,-1.71872306472263,50.8811988069719));
#12030=CARTESIAN_POINT('Ctrl Pts',(2.96604676899315,-1.64187733811533,50.8862896908081));
#12031=CARTESIAN_POINT('Ctrl Pts',(2.99126965412893,-1.59546259952072,50.8892869662395));
#12032=CARTESIAN_POINT('Ctrl Pts',(3.04369150994376,-1.49337975464593,50.8957265132123));
#12033=CARTESIAN_POINT('Ctrl Pts',(3.07047006879992,-1.43751703557933,50.8991549778405));
#12034=CARTESIAN_POINT('Ctrl Pts',(3.14847188970471,-1.26265871937509,50.9096383085556));
#12035=CARTESIAN_POINT('Ctrl Pts',(3.19441832538802,-1.14143611673253,50.9165550871717));
#12036=CARTESIAN_POINT('Ctrl Pts',(3.2999803841755,-0.806115290203916,50.935237920404));
#12037=CARTESIAN_POINT('Ctrl Pts',(3.34567261715104,-0.588340569558574,
50.9468782790256));
#12038=CARTESIAN_POINT('Ctrl Pts',(3.37357321334678,-0.33264385636009,50.9614335353705));
#12039=CARTESIAN_POINT('Ctrl Pts',(3.37685045289602,-0.297538190790384,
50.9634516204217));
#12040=CARTESIAN_POINT('Ctrl Pts',(3.38120630577591,-0.241434712943392,
50.9667171344041));
#12041=CARTESIAN_POINT('Ctrl Pts',(3.38263823971397,-0.220466077580982,
50.9679465923971));
#12042=CARTESIAN_POINT('Ctrl Pts',(3.38509349233651,-0.178817719287028,
50.9704087271372));
#12043=CARTESIAN_POINT('Ctrl Pts',(3.38612250565234,-0.158139326963475,
50.9716410761596));
#12044=CARTESIAN_POINT('Ctrl Pts',(3.38833211778515,-0.103692758148475,
50.9749096455387));
#12045=CARTESIAN_POINT('Ctrl Pts',(3.38919731902172,-0.0699147614432324,
50.9769614640334));
#12046=CARTESIAN_POINT('Ctrl Pts',(3.39144539304957,0.140984356942711,50.989899476896));
#12047=CARTESIAN_POINT('Ctrl Pts',(3.37944805712352,0.317961450163962,51.0013014153132));
#12048=CARTESIAN_POINT('Ctrl Pts',(3.32058220268071,0.718260439995007,51.0273503581134));
#12049=CARTESIAN_POINT('Ctrl Pts',(3.26490159203354,0.939472748909802,51.041903809923));
#12050=CARTESIAN_POINT('Ctrl Pts',(3.16763704817694,1.20825336871614,51.0593411196336));
#12051=CARTESIAN_POINT('Ctrl Pts',(3.14639793318988,1.26252973827489,51.0628526961353));
#12052=CARTESIAN_POINT('Ctrl Pts',(3.10948309290259,1.35013834081802,51.068507530299));
#12053=CARTESIAN_POINT('Ctrl Pts',(3.09464576630408,1.38380865136708,51.0706776188934));
#12054=CARTESIAN_POINT('Ctrl Pts',(3.06452005824452,1.44926369874454,51.0748919811378));
#12055=CARTESIAN_POINT('Ctrl Pts',(3.04927804288143,1.48106448503404,51.0769374713223));
#12056=CARTESIAN_POINT('Ctrl Pts',(3.01124948554602,1.55733019479729,51.0818413733612));
#12057=CARTESIAN_POINT('Ctrl Pts',(2.98797045065487,1.60154105357617,51.0846826833174));
#12058=CARTESIAN_POINT('Ctrl Pts',(2.88772764377693,1.78211950177047,51.0963035997398));
#12059=CARTESIAN_POINT('Ctrl Pts',(2.80233645084357,1.91359299465454,51.1047909677306));
#12060=CARTESIAN_POINT('Ctrl Pts',(2.62450155193859,2.1498238041335,51.120588265185));
#12061=CARTESIAN_POINT('Ctrl Pts',(2.53409034779772,2.25568973176625,51.1279114807518));
#12062=CARTESIAN_POINT('Ctrl Pts',(2.34755708273018,2.4486948039968,51.142280559732));
#12063=CARTESIAN_POINT('Ctrl Pts',(2.25244123554241,2.53646068588342,51.1492998749553));
#12064=CARTESIAN_POINT('Ctrl Pts',(2.12750804953232,2.6391600642915,51.1584845690548));
#12065=CARTESIAN_POINT('Ctrl Pts',(2.10216784750255,2.65938837396396,51.1603459586974));
#12066=CARTESIAN_POINT('Ctrl Pts',(2.06198820049496,2.69052946280075,51.1633018248083));
#12067=CARTESIAN_POINT('Ctrl Pts',(2.04734270757057,2.70169056936238,51.1643801409092));
#12068=CARTESIAN_POINT('Ctrl Pts',(2.01602156803004,2.72515901032878,51.1666898537986));
#12069=CARTESIAN_POINT('Ctrl Pts',(1.99932266557269,2.73743372839147,51.1679234501976));
#12070=CARTESIAN_POINT('Ctrl Pts',(1.95505893109681,2.76934923751482,51.1711967368812));
#12071=CARTESIAN_POINT('Ctrl Pts',(1.92731122310546,2.78873123203654,51.1732520767495));
#12072=CARTESIAN_POINT('Ctrl Pts',(1.86435461453637,2.83131856039307,51.1779147458144));
#12073=CARTESIAN_POINT('Ctrl Pts',(1.82899371716767,2.85428881029334,51.1805331487497));
#12074=CARTESIAN_POINT('Ctrl Pts',(1.71228718946605,2.92704152103061,51.189151517978));
#12075=CARTESIAN_POINT('Ctrl Pts',(1.62927004288795,2.97405058821817,51.1952444944297));
#12076=CARTESIAN_POINT('Ctrl Pts',(1.31320291347944,3.13581710690244,51.218054227701));
#12077=CARTESIAN_POINT('Ctrl Pts',(1.06914929048292,3.22719814109254,51.2348256630643));
#12078=CARTESIAN_POINT('Ctrl Pts',(0.756755189036587,3.30478201921148,51.2545202273031));
#12079=CARTESIAN_POINT('Ctrl Pts',(0.696074424957335,3.31809339150359,51.2582719191943));
#12080=CARTESIAN_POINT('Ctrl Pts',(0.598164907463169,3.33676707273177,51.2642101077037));
#12081=CARTESIAN_POINT('Ctrl Pts',(0.561155319407196,3.34319018751275,51.2664286967592));
#12082=CARTESIAN_POINT('Ctrl Pts',(0.489521157817721,3.35439938178435,51.2706748644592));
#12083=CARTESIAN_POINT('Ctrl Pts',(0.454914472380718,3.35926764811395,51.2727047261129));
#12084=CARTESIAN_POINT('Ctrl Pts',(0.372826140364179,3.36952350897208,51.2774719428083));
#12085=CARTESIAN_POINT('Ctrl Pts',(0.325293082510113,3.37444406334867,51.280194752315));
#12086=CARTESIAN_POINT('Ctrl Pts',(0.147596889819737,3.38904906566998,51.2902502451853));
#12087=CARTESIAN_POINT('Ctrl Pts',(0.0170081292474336,3.39221958541235,
51.2973885926618));
#12088=CARTESIAN_POINT('Ctrl Pts',(-0.252874782560523,3.3831820800764,51.3119167667793));
#12089=CARTESIAN_POINT('Ctrl Pts',(-0.391882060304622,3.36991034417655,
51.3192759000744));
#12090=CARTESIAN_POINT('Ctrl Pts',(-0.674657313741865,3.32517494142439,
51.3345195787468));
#12091=CARTESIAN_POINT('Ctrl Pts',(-0.817984027549354,3.2928476095757,51.3423967332442));
#12092=CARTESIAN_POINT('Ctrl Pts',(-0.996644941965798,3.24016431350472,
51.3528856327293));
#12093=CARTESIAN_POINT('Ctrl Pts',(-1.03433949712157,3.22832889352018,51.3551378653434));
#12094=CARTESIAN_POINT('Ctrl Pts',(-1.09259449605376,3.20891289933913,51.3586920747182));
#12095=CARTESIAN_POINT('Ctrl Pts',(-1.11330390725119,3.20178685767882,51.3599702013536));
#12096=CARTESIAN_POINT('Ctrl Pts',(-1.1529083576904,3.1877284109914,51.3624451994619));
#12097=CARTESIAN_POINT('Ctrl Pts',(-1.17181315036002,3.18082756018247,51.3636403816511));
#12098=CARTESIAN_POINT('Ctrl Pts',(-1.21945680171208,3.16295376060578,51.366685650754));
#12099=CARTESIAN_POINT('Ctrl Pts',(-1.24810947751682,3.15175728290683,51.3685477436155));
#12100=CARTESIAN_POINT('Ctrl Pts',(-1.37609403323414,3.09972649009205,51.376991300474));
#12101=CARTESIAN_POINT('Ctrl Pts',(-1.47359725627769,3.05457794910724,51.3837662181386));
#12102=CARTESIAN_POINT('Ctrl Pts',(-1.8234411821228,2.87193195696922,51.4089691175009));
#12103=CARTESIAN_POINT('Ctrl Pts',(-2.06021279408939,2.70712022312822,51.4276844349272));
#12104=CARTESIAN_POINT('Ctrl Pts',(-2.3224422219859,2.47002940924011,51.4493906312513));
#12105=CARTESIAN_POINT('Ctrl Pts',(-2.37021533579752,2.4242242716559,51.4533992210571));
#12106=CARTESIAN_POINT('Ctrl Pts',(-2.44374408004428,2.34947145429332,51.459659275503));
#12107=CARTESIAN_POINT('Ctrl Pts',(-2.47039540505616,2.32143230999211,51.4619484558853));
#12108=CARTESIAN_POINT('Ctrl Pts',(-2.51996675349378,2.26745888968959,51.4662472748003));
#12109=CARTESIAN_POINT('Ctrl Pts',(-2.54298073958333,2.24161801881715,51.4682606680281));
#12110=CARTESIAN_POINT('Ctrl Pts',(-2.59515928108421,2.18119222074448,51.4728696732307));
#12111=CARTESIAN_POINT('Ctrl Pts',(-2.62403553948191,2.14636645475345,51.4754535809631));
#12112=CARTESIAN_POINT('Ctrl Pts',(-2.71977396876846,2.02608151096315,51.4841485645555));
#12113=CARTESIAN_POINT('Ctrl Pts',(-2.78322965550586,1.9379918308852,51.4901314802297));
#12114=CARTESIAN_POINT('Ctrl Pts',(-2.94405356249563,1.69049987475813,51.5061386691015));
#12115=CARTESIAN_POINT('Ctrl Pts',(-3.03265169641367,1.52586559173489,51.515929248131));
#12116=CARTESIAN_POINT('Ctrl Pts',(-3.16356987145404,1.22559755007993,51.5334212304276));
#12117=CARTESIAN_POINT('Ctrl Pts',(-3.21177600473811,1.09304663090856,51.5410367137765));
#12118=CARTESIAN_POINT('Ctrl Pts',(-3.26083842657181,0.926503538899818,
51.5508932802624));
#12119=CARTESIAN_POINT('Ctrl Pts',(-3.26963087434435,0.894980351820823,
51.5527714711769));
#12120=CARTESIAN_POINT('Ctrl Pts',(-3.28267084537566,0.845469421872272,
51.5557479301081));
#12121=CARTESIAN_POINT('Ctrl Pts',(-3.2872302109388,0.827565059713995,51.5568296770401));
#12122=CARTESIAN_POINT('Ctrl Pts',(-3.29657728914046,0.789563204837427,
51.5591387703207));
#12123=CARTESIAN_POINT('Ctrl Pts',(-3.30132802622744,0.769457653527173,
51.5603682138607));
#12124=CARTESIAN_POINT('Ctrl Pts',(-3.31330767188874,0.716604480789697,
51.5636182725297));
#12125=CARTESIAN_POINT('Ctrl Pts',(-3.32023475482486,0.68379141546493,51.56565416774));
#12126=CARTESIAN_POINT('Ctrl Pts',(-3.33467145282173,0.610005144884213,
51.5702647852953));
#12127=CARTESIAN_POINT('Ctrl Pts',(-3.34191488328282,0.568985595155038,
51.5728502397294));
#12128=CARTESIAN_POINT('Ctrl Pts',(-3.36884386333107,0.398160727214537,
51.5836825681657));
#12129=CARTESIAN_POINT('Ctrl Pts',(-3.38172925503845,0.26744239336117,51.5921228543816));
#12130=CARTESIAN_POINT('Ctrl Pts',(-3.38700661379996,0.136349772919876,
51.6005689639805));
#12131=CARTESIAN_POINT('',(-3.38974999869979,9.38871559445019E-5,50.0160178032496));
#12132=CARTESIAN_POINT('Ctrl Pts',(-3.38700661857411,0.136349654327206,
51.2580969930732));
#12133=CARTESIAN_POINT('Ctrl Pts',(-3.38238609317346,0.251126257102754,
51.2513820182541));
#12134=CARTESIAN_POINT('Ctrl Pts',(-3.37193260407542,0.365517353525659,
51.244667043435));
#12135=CARTESIAN_POINT('Ctrl Pts',(-3.35574418187459,0.478942635724639,
51.2379520686159));
#12136=CARTESIAN_POINT('Ctrl Pts',(-3.33998514488251,0.589359401227443,
51.23141520324));
#12137=CARTESIAN_POINT('Ctrl Pts',(-3.31879173836351,0.6988606573217,51.2248783378641));
#12138=CARTESIAN_POINT('Ctrl Pts',(-3.29230537054002,0.806926520578764,
51.2183414724881));
#12139=CARTESIAN_POINT('Ctrl Pts',(-3.2647364948276,0.919409076614527,51.2115374429474));
#12140=CARTESIAN_POINT('Ctrl Pts',(-3.23143298620414,1.03033602875945,51.2047334134067));
#12141=CARTESIAN_POINT('Ctrl Pts',(-3.19260961647215,1.13914393265713,51.197929383866));
#12142=CARTESIAN_POINT('Ctrl Pts',(-3.15378624674016,1.24795183655482,51.1911253543253));
#12143=CARTESIAN_POINT('Ctrl Pts',(-3.10944323885395,1.3546403622979,51.1843213247846));
#12144=CARTESIAN_POINT('Ctrl Pts',(-3.05984868931851,1.45867441911338,51.1775172952438));
#12145=CARTESIAN_POINT('Ctrl Pts',(-3.01534232440451,1.55203503513846,51.1714113294782));
#12146=CARTESIAN_POINT('Ctrl Pts',(-2.96648525399577,1.64351199803028,51.1653053637126));
#12147=CARTESIAN_POINT('Ctrl Pts',(-2.91345995819217,1.73267311819365,51.159199397947));
#12148=CARTESIAN_POINT('Ctrl Pts',(-2.8605036792689,1.82171818766332,51.1531013796091));
#12149=CARTESIAN_POINT('Ctrl Pts',(-2.80339017764802,1.90845304315786,51.1470033612713));
#12150=CARTESIAN_POINT('Ctrl Pts',(-2.74234906458397,1.99246748291545,51.1409053429334));
#12151=CARTESIAN_POINT('Ctrl Pts',(-2.68137001247147,2.07639650457016,51.134813524496));
#12152=CARTESIAN_POINT('Ctrl Pts',(-2.61647153956889,2.15761026701092,51.1287217060585));
#12153=CARTESIAN_POINT('Ctrl Pts',(-2.54792758214111,2.23572585498861,51.1226298876211));
#12154=CARTESIAN_POINT('Ctrl Pts',(-2.47943149408921,2.31378688900438,51.1165423235564));
#12155=CARTESIAN_POINT('Ctrl Pts',(-2.4072952652929,2.38875373131041,51.1104547594917));
#12156=CARTESIAN_POINT('Ctrl Pts',(-2.33183378098951,2.46027565129117,51.104367195427));
#12157=CARTESIAN_POINT('Ctrl Pts',(-2.25639958327868,2.5317717092112,51.0982818326029));
#12158=CARTESIAN_POINT('Ctrl Pts',(-2.17764282950951,2.5998250272145,51.0921964697788));
#12159=CARTESIAN_POINT('Ctrl Pts',(-2.09591545520761,2.66412151883541,51.0861111069547));
#12160=CARTESIAN_POINT('Ctrl Pts',(-2.01419655095042,2.72841134690982,51.0800263748041));
#12161=CARTESIAN_POINT('Ctrl Pts',(-1.9295079740343,2.78894485889433,51.0739416426536));
#12162=CARTESIAN_POINT('Ctrl Pts',(-1.84223423472553,2.845448661794,51.0678569105031));
#12163=CARTESIAN_POINT('Ctrl Pts',(-1.75494702767579,2.90196118413879,51.0617712393806));
#12164=CARTESIAN_POINT('Ctrl Pts',(-1.66507422409557,2.95444252980832,51.055685568258));
#12165=CARTESIAN_POINT('Ctrl Pts',(-1.57302798386049,3.0026634883869,51.0495998971355));
#12166=CARTESIAN_POINT('Ctrl Pts',(-1.480886846121,3.05093416163735,51.0435079518295));
#12167=CARTESIAN_POINT('Ctrl Pts',(-1.38656817589773,3.09493547777582,51.0374160065234));
#12168=CARTESIAN_POINT('Ctrl Pts',(-1.29050729109405,3.13448496473234,51.0313240612174));
#12169=CARTESIAN_POINT('Ctrl Pts',(-1.19439439738538,3.17405586441594,51.0252288176344));
#12170=CARTESIAN_POINT('Ctrl Pts',(-1.09653781209418,3.20916998946029,51.0191335740514));
#12171=CARTESIAN_POINT('Ctrl Pts',(-0.997389454265164,3.23969432802242,
51.0130383304684));
#12172=CARTESIAN_POINT('Ctrl Pts',(-0.898082375398527,3.27026753128383,
51.0069333293523));
#12173=CARTESIAN_POINT('Ctrl Pts',(-0.797479806827848,3.29623616410636,
51.0008283282361));
#12174=CARTESIAN_POINT('Ctrl Pts',(-0.696045528625235,3.31751800064157,
50.99472332712));
#12175=CARTESIAN_POINT('Ctrl Pts',(-0.621505806011331,3.3331571141657,50.9902370223144));
#12176=CARTESIAN_POINT('Ctrl Pts',(-0.546517177004937,3.34626635828502,
50.9857507175088));
#12177=CARTESIAN_POINT('Ctrl Pts',(-0.471264993133025,3.35683100092145,
50.9812644127032));
#12178=CARTESIAN_POINT('Ctrl Pts',(-0.368976564799787,3.37119125780148,
50.9751662897786));
#12179=CARTESIAN_POINT('Ctrl Pts',(-0.265858260901948,3.38089616573506,
50.9690681668541));
#12180=CARTESIAN_POINT('Ctrl Pts',(-0.162370066605167,3.38585897874832,
50.9629700439296));
#12181=CARTESIAN_POINT('Ctrl Pts',(-0.0590172561375931,3.39081529938211,
50.9568798986033));
#12182=CARTESIAN_POINT('Ctrl Pts',(0.0447040585680405,3.39104183758612,
50.950789753277));
#12183=CARTESIAN_POINT('Ctrl Pts',(0.148326141367558,3.38650327303651,50.9446996079506));
#12184=CARTESIAN_POINT('Ctrl Pts',(0.251842401734575,3.38196934342502,50.93861568209));
#12185=CARTESIAN_POINT('Ctrl Pts',(0.355259206099814,3.37268000617653,50.9325317562294));
#12186=CARTESIAN_POINT('Ctrl Pts',(0.458107050130199,3.35865196070105,50.9264478303688));
#12187=CARTESIAN_POINT('Ctrl Pts',(0.560883025557151,3.34463371782325,50.9203681558687));
#12188=CARTESIAN_POINT('Ctrl Pts',(0.663090408115839,3.32588340899181,50.9142884813685));
#12189=CARTESIAN_POINT('Ctrl Pts',(0.764263886960711,3.30246964764064,50.9082088068684));
#12190=CARTESIAN_POINT('Ctrl Pts',(0.865400811614649,3.27906434573075,50.9021313289674));
#12191=CARTESIAN_POINT('Ctrl Pts',(0.965504158150382,3.25099903635872,50.8960538510664));
#12192=CARTESIAN_POINT('Ctrl Pts',(1.0641186988592,3.21839345904726,50.8899763731655));
#12193=CARTESIAN_POINT('Ctrl Pts',(1.16272323352482,3.18579119009999,50.8838995119231));
#12194=CARTESIAN_POINT('Ctrl Pts',(1.25983885614774,3.14864970375598,50.8778226506808));
#12195=CARTESIAN_POINT('Ctrl Pts',(1.35502628589034,3.10713836625378,50.8717457894384));
#12196=CARTESIAN_POINT('Ctrl Pts',(1.45022879016512,3.06562045473237,50.8656679658228));
#12197=CARTESIAN_POINT('Ctrl Pts',(1.5435021022964,3.01973148835263,50.8595901422072));
#12198=CARTESIAN_POINT('Ctrl Pts',(1.63442853190733,2.9696882726285,50.8535123185915));
#12199=CARTESIAN_POINT('Ctrl Pts',(1.72545008344898,2.91959270460901,50.8474281367111));
#12200=CARTESIAN_POINT('Ctrl Pts',(1.81411947369797,2.86533441547347,50.8413439548306));
#12201=CARTESIAN_POINT('Ctrl Pts',(1.90004521796449,2.80717531198005,50.8352597729502));
#12202=CARTESIAN_POINT('Ctrl Pts',(1.98601804169933,2.74898434260412,50.8291722574932));
#12203=CARTESIAN_POINT('Ctrl Pts',(2.06924388206197,2.68688855801591,50.8230847420362));
#12204=CARTESIAN_POINT('Ctrl Pts',(2.14936337133644,2.62119098130167,50.8169972265792));
#12205=CARTESIAN_POINT('Ctrl Pts',(2.22961307137135,2.55538663242126,50.810899817649));
#12206=CARTESIAN_POINT('Ctrl Pts',(2.30674601743564,2.48596908519958,50.8048024087188));
#12207=CARTESIAN_POINT('Ctrl Pts',(2.3804386759118,2.41327925709464,50.7987049997886));
#12208=CARTESIAN_POINT('Ctrl Pts',(2.43560463203426,2.35886401478006,50.7941405099133));
#12209=CARTESIAN_POINT('Ctrl Pts',(2.48884342648908,2.30261578862049,50.7895760200379));
#12210=CARTESIAN_POINT('Ctrl Pts',(2.5400344934993,2.24468925117348,50.7850115301626));
#12211=CARTESIAN_POINT('Ctrl Pts',(2.60861698763998,2.16708300760258,50.7788963206462));
#12212=CARTESIAN_POINT('Ctrl Pts',(2.6737522283564,2.08620330603658,50.7727811111299));
#12213=CARTESIAN_POINT('Ctrl Pts',(2.73511350553951,2.00238836750401,50.7666659016136));
#12214=CARTESIAN_POINT('Ctrl Pts',(2.79639464695022,1.91868288847337,50.760558678356));
#12215=CARTESIAN_POINT('Ctrl Pts',(2.85391137495837,1.83205013479395,50.7544514550985));
#12216=CARTESIAN_POINT('Ctrl Pts',(2.90737569847378,1.74286304981891,50.7483442318409));
#12217=CARTESIAN_POINT('Ctrl Pts',(2.96078530298451,1.6537672449387,50.7422432591287));
#12218=CARTESIAN_POINT('Ctrl Pts',(3.01015053355163,1.56212267104315,50.7361422864165));
#12219=CARTESIAN_POINT('Ctrl Pts',(3.055225880012,1.4683323481436,50.7300413137042));
#12220=CARTESIAN_POINT('Ctrl Pts',(3.1002689573856,1.37460916900013,50.7239447086305));
#12221=CARTESIAN_POINT('Ctrl Pts',(3.1410280749658,1.27874367860853,50.7178481035567));
#12222=CARTESIAN_POINT('Ctrl Pts',(3.17730338172666,1.18116395261976,50.711751498483));
#12223=CARTESIAN_POINT('Ctrl Pts',(3.21356515562498,1.08362062971441,50.7056571678082));
#12224=CARTESIAN_POINT('Ctrl Pts',(3.24534629552966,0.984364740910517,50.6995628371334));
#12225=CARTESIAN_POINT('Ctrl Pts',(3.27249517191522,0.88384411085417,50.6934685064585));
#12226=CARTESIAN_POINT('Ctrl Pts',(3.29964086532482,0.783335265990847,50.6873748902924));
#12227=CARTESIAN_POINT('Ctrl Pts',(3.3221552644091,0.681562385665184,50.6812812741263));
#12228=CARTESIAN_POINT('Ctrl Pts',(3.33993693075423,0.57898735831103,50.6751876579601));
#12229=CARTESIAN_POINT('Ctrl Pts',(3.35772106110552,0.476398117131597,50.6690931974014));
#12230=CARTESIAN_POINT('Ctrl Pts',(3.37077108308944,0.373006927482335,50.6629987368426));
#12231=CARTESIAN_POINT('Ctrl Pts',(3.37903703200953,0.269283862881242,50.6569042762839));
#12232=CARTESIAN_POINT('Ctrl Pts',(3.38731122028522,0.165457408914655,50.6508037408718));
#12233=CARTESIAN_POINT('Ctrl Pts',(3.39079177831328,0.0612988444033651,
50.6447032054596));
#12234=CARTESIAN_POINT('Ctrl Pts',(3.38948081194506,-0.0427187073333277,
50.6386026700475));
#12235=CARTESIAN_POINT('Ctrl Pts',(3.38816915803506,-0.146790811509927,
50.632498935184));
#12236=CARTESIAN_POINT('Ctrl Pts',(3.38206099820747,-0.250721330601563,
50.6263952003206));
#12237=CARTESIAN_POINT('Ctrl Pts',(3.37121045455189,-0.354041146789476,
50.6202914654572));
#12238=CARTESIAN_POINT('Ctrl Pts',(3.36034300140308,-0.457521976636091,
50.6141782185299));
#12239=CARTESIAN_POINT('Ctrl Pts',(3.34471846477157,-0.560389781347759,
50.6080649716027));
#12240=CARTESIAN_POINT('Ctrl Pts',(3.32444235334103,-0.662184341261841,
50.6019517246755));
#12241=CARTESIAN_POINT('Ctrl Pts',(3.30985630746213,-0.735412392222972,
50.5975540323243));
#12242=CARTESIAN_POINT('Ctrl Pts',(3.29286417536053,-0.808085261419362,
50.5931563399731));
#12243=CARTESIAN_POINT('Ctrl Pts',(3.27352104037737,-0.88003696553423,50.5887586476219));
#12244=CARTESIAN_POINT('Ctrl Pts',(3.24664850436202,-0.979996189407429,
50.58264913403));
#12245=CARTESIAN_POINT('Ctrl Pts',(3.21514945967312,-1.07888658774537,50.576539620438));
#12246=CARTESIAN_POINT('Ctrl Pts',(3.17912595974147,-1.17624963107238,50.570430106846));
#12247=CARTESIAN_POINT('Ctrl Pts',(3.14314874037317,-1.27348758892728,50.5643284423451));
#12248=CARTESIAN_POINT('Ctrl Pts',(3.10265876947978,-1.36920169648386,50.5582267778441));
#12249=CARTESIAN_POINT('Ctrl Pts',(3.05780841205472,-1.46294660793461,50.5521251133432));
#12250=CARTESIAN_POINT('Ctrl Pts',(3.01300295146507,-1.556597677327,50.5460295568298));
#12251=CARTESIAN_POINT('Ctrl Pts',(2.96384596785311,-1.64828308812112,50.5399340003165));
#12252=CARTESIAN_POINT('Ctrl Pts',(2.91053832948993,-1.73757638539144,50.5338384438032));
#12253=CARTESIAN_POINT('Ctrl Pts',(2.85726684321948,-1.82680912586984,50.527747021165));
#12254=CARTESIAN_POINT('Ctrl Pts',(2.79985051790869,-1.91365261387333,50.5216555985269));
#12255=CARTESIAN_POINT('Ctrl Pts',(2.73853629076501,-1.99770469455898,50.5155641758887));
#12256=CARTESIAN_POINT('Ctrl Pts',(2.67724349359053,-2.08172739815577,50.5094748822671));
#12257=CARTESIAN_POINT('Ctrl Pts',(2.61205575346245,-2.16296028953365,50.5033855886454));
#12258=CARTESIAN_POINT('Ctrl Pts',(2.54326304242446,-2.24103060209759,50.4972962950237));
#12259=CARTESIAN_POINT('Ctrl Pts',(2.47447670201679,-2.31909368486795,50.4912075653083));
#12260=CARTESIAN_POINT('Ctrl Pts',(2.4020863365294,-2.39399445144511,50.4851188355929));
#12261=CARTESIAN_POINT('Ctrl Pts',(2.32642128351071,-2.46539430398636,50.4790301058774));
#12262=CARTESIAN_POINT('Ctrl Pts',(2.25074379926239,-2.53680588701515,50.472940375827));
#12263=CARTESIAN_POINT('Ctrl Pts',(2.17179086853526,-2.60471512050655,50.4668506457766));
#12264=CARTESIAN_POINT('Ctrl Pts',(2.08992698377767,-2.66882188708388,50.4607609157262));
#12265=CARTESIAN_POINT('Ctrl Pts',(2.00797783578205,-2.73299542242639,50.4546648430731));
#12266=CARTESIAN_POINT('Ctrl Pts',(1.92311201553347,-2.79335831876617,50.4485687704199));
#12267=CARTESIAN_POINT('Ctrl Pts',(1.83572522232259,-2.84965225433362,50.4424726977667));
#12268=CARTESIAN_POINT('Ctrl Pts',(1.74829051866409,-2.9059770534624,50.4363732828972));
#12269=CARTESIAN_POINT('Ctrl Pts',(1.65833245748417,-2.95822823385694,50.4302738680277));
#12270=CARTESIAN_POINT('Ctrl Pts',(1.56627198999204,-3.00619312684105,50.4241744531582));
#12271=CARTESIAN_POINT('Ctrl Pts',(1.47406382635318,-3.05423497174671,50.4180652527629));
#12272=CARTESIAN_POINT('Ctrl Pts',(1.37974690559371,-3.09797661321588,50.4119560523677));
#12273=CARTESIAN_POINT('Ctrl Pts',(1.28376301401928,-3.13725319130225,50.4058468519724));
#12274=CARTESIAN_POINT('Ctrl Pts',(1.21389410839056,-3.16584352539604,50.4013998230087));
#12275=CARTESIAN_POINT('Ctrl Pts',(1.14314233688534,-3.1920689633944,50.396952794045));
#12276=CARTESIAN_POINT('Ctrl Pts',(1.07168247758956,-3.21588272947375,50.3925057650813));
#12277=CARTESIAN_POINT('Ctrl Pts',(0.974484192739338,-3.24827374229615,
50.3864570043894));
#12278=CARTESIAN_POINT('Ctrl Pts',(0.875636788894064,-3.27631376402613,
50.3804082436976));
#12279=CARTESIAN_POINT('Ctrl Pts',(0.775569533376517,-3.29983286870686,
50.3743594830057));
#12280=CARTESIAN_POINT('Ctrl Pts',(0.675634356763346,-3.32332093048986,
50.3683187060812));
#12281=CARTESIAN_POINT('Ctrl Pts',(0.574482948375973,-3.34229983416437,
50.3622779291567));
#12282=CARTESIAN_POINT('Ctrl Pts',(0.472561959383147,-3.35664866452299,
50.3562371522321));
#12283=CARTESIAN_POINT('Ctrl Pts',(0.370745031754765,-3.37098284472093,
50.3502025429429));
#12284=CARTESIAN_POINT('Ctrl Pts',(0.268160514506922,-3.3806962874626,50.3441679336537));
#12285=CARTESIAN_POINT('Ctrl Pts',(0.165266583023911,-3.38571883342897,
50.3381333243645));
#12286=CARTESIAN_POINT('Ctrl Pts',(0.062440570147767,-3.39073806409462,
50.3321026984225));
#12287=CARTESIAN_POINT('Ctrl Pts',(-0.0406940169840591,-3.39107252976694,
50.3260720724805));
#12288=CARTESIAN_POINT('Ctrl Pts',(-0.143673419542869,-3.38670385640919,
50.3200414465384));
#12289=CARTESIAN_POINT('Ctrl Pts',(-0.24661825811988,-3.3823366493519,50.3140128447143));
#12290=CARTESIAN_POINT('Ctrl Pts',(-0.349407580425442,-3.37326945722734,
50.3079842428901));
#12291=CARTESIAN_POINT('Ctrl Pts',(-0.451578116844336,-3.35953601958475,
50.3019556410659));
#12292=CARTESIAN_POINT('Ctrl Pts',(-0.553741992782523,-3.34580347722273,
50.2959274322453));
#12293=CARTESIAN_POINT('Ctrl Pts',(-0.655286730866545,-3.32740535195045,
50.2898992234247));
#12294=CARTESIAN_POINT('Ctrl Pts',(-0.755755695255239,-3.30442708976749,
50.2838710146042));
#12295=CARTESIAN_POINT('Ctrl Pts',(-0.856245283087935,-3.28144411079556,
50.2778415683623));
#12296=CARTESIAN_POINT('Ctrl Pts',(-0.955658233567042,-3.25387922458748,
50.2718121221205));
#12297=CARTESIAN_POINT('Ctrl Pts',(-1.05355059476116,-3.22186843411993,
50.2657826758787));
#12298=CARTESIAN_POINT('Ctrl Pts',(-1.15155783809582,-3.18982007720608,
50.2597461537458));
#12299=CARTESIAN_POINT('Ctrl Pts',(-1.24804051385002,-3.15331553394133,
50.2537096316129));
#12300=CARTESIAN_POINT('Ctrl Pts',(-1.34257233603639,-3.11253989291861,
50.2476731094799));
#12301=CARTESIAN_POINT('Ctrl Pts',(-1.43716132893339,-3.07173959170931,
50.2416329365948));
#12302=CARTESIAN_POINT('Ctrl Pts',(-1.52979672830863,-3.02666324234653,
50.2355927637096));
#12303=CARTESIAN_POINT('Ctrl Pts',(-1.62007662889155,-2.97754207006708,
50.2295525908245));
#12304=CARTESIAN_POINT('Ctrl Pts',(-1.71051958478066,-2.92833217961522,
50.223501508731));
#12305=CARTESIAN_POINT('Ctrl Pts',(-1.79859817213365,-2.87506310127268,
50.2174504266376));
#12306=CARTESIAN_POINT('Ctrl Pts',(-1.88393906443226,-2.81800969906175,
50.2113993445441));
#12307=CARTESIAN_POINT('Ctrl Pts',(-1.95514465282031,-2.77040624701729,
50.2063505238763));
#12308=CARTESIAN_POINT('Ctrl Pts',(-2.02444480706955,-2.72016911359938,
50.2013017032085));
#12309=CARTESIAN_POINT('Ctrl Pts',(-2.09164155441515,-2.66747833549661,
50.1962528825407));
#12310=CARTESIAN_POINT('Ctrl Pts',(-2.17420186419761,-2.60274057459771,
50.1900497221968));
#12311=CARTESIAN_POINT('Ctrl Pts',(-2.25388088605287,-2.53406697426379,
50.1838465618529));
#12312=CARTESIAN_POINT('Ctrl Pts',(-2.33028851954139,-2.46173931970743,
50.177643401509));
#12313=CARTESIAN_POINT('Ctrl Pts',(-2.40658582881859,-2.38951609832196,
50.1714491978458));
#12314=CARTESIAN_POINT('Ctrl Pts',(-2.47962085078108,-2.31364960005651,
50.1652549941826));
#12315=CARTESIAN_POINT('Ctrl Pts',(-2.54903549203045,-2.23446260270095,
50.1590607905194));
#12316=CARTESIAN_POINT('Ctrl Pts',(-2.61835116314992,-2.15538850872244,
50.1528754184388));
#12317=CARTESIAN_POINT('Ctrl Pts',(-2.68405646356693,-2.0730036513876,50.1466900463582));
#12318=CARTESIAN_POINT('Ctrl Pts',(-2.74582992284387,-1.98766775325134,
50.1405046742776));
#12319=CARTESIAN_POINT('Ctrl Pts',(-2.80755240900049,-1.90240227106804,
50.134324406132));
#12320=CARTESIAN_POINT('Ctrl Pts',(-2.86534926738651,-1.81419092354675,
50.1281441379863));
#12321=CARTESIAN_POINT('Ctrl Pts',(-2.91893923119918,-1.72342647857875,
50.1219638698406));
#12322=CARTESIAN_POINT('Ctrl Pts',(-2.97249733481119,-1.63271599471137,
50.1157872759759));
#12323=CARTESIAN_POINT('Ctrl Pts',(-3.02185331151303,-1.53945578678077,
50.1096106821112));
#12324=CARTESIAN_POINT('Ctrl Pts',(-3.06676957025133,-1.44406698787849,
50.1034340882465));
#12325=CARTESIAN_POINT('Ctrl Pts',(-3.11166948095893,-1.34871290734005,
50.0972597424574));
#12326=CARTESIAN_POINT('Ctrl Pts',(-3.15213271525814,-1.25123214969023,
50.0910853966683));
#12327=CARTESIAN_POINT('Ctrl Pts',(-3.18796827153445,-1.15206916554071,
50.0849110508792));
#12328=CARTESIAN_POINT('Ctrl Pts',(-3.22380944156518,-1.05289064719278,
50.0787357378591));
#12329=CARTESIAN_POINT('Ctrl Pts',(-3.25502133760869,-0.952029759991573,
50.072560424839));
#12330=CARTESIAN_POINT('Ctrl Pts',(-3.28146174758333,-0.849949328870463,
50.0663851118189));
#12331=CARTESIAN_POINT('Ctrl Pts',(-3.30790346808446,-0.747863838103573,
50.0602094927176));
#12332=CARTESIAN_POINT('Ctrl Pts',(-3.3295731347263,-0.644559083050461,
50.0540338736164));
#12333=CARTESIAN_POINT('Ctrl Pts',(-3.34637920118809,-0.540510225949323,
50.0478582545151));
#12334=CARTESIAN_POINT('Ctrl Pts',(-3.36319782829134,-0.436383604048632,
50.0416780198343));
#12335=CARTESIAN_POINT('Ctrl Pts',(-3.37514553356435,-0.331512176604862,
50.0354977851534));
#12336=CARTESIAN_POINT('Ctrl Pts',(-3.38218241566213,-0.226378377249048,
50.0293175504725));
#12337=CARTESIAN_POINT('Ctrl Pts',(-3.38723016104025,-0.150963066546201,
50.0248843013982));
#12338=CARTESIAN_POINT('Ctrl Pts',(-3.38975209003901,-0.0754128960838142,
50.0204510523239));
#12339=CARTESIAN_POINT('Ctrl Pts',(-3.38974999869979,9.38871559445019E-5,
50.0160178032496));
#12340=CARTESIAN_POINT('Ctrl Pts',(-3.38974999927235,7.02360661182119E-5,
50.0155995406885));
#12341=CARTESIAN_POINT('Ctrl Pts',(-3.38974905771225,0.0455120371475817,
50.0130593630806));
#12342=CARTESIAN_POINT('Ctrl Pts',(-3.38883435054036,0.0909477037524909,
50.0104961979471));
#12343=CARTESIAN_POINT('Ctrl Pts',(-3.38700661857411,0.136349654327351,
50.0079012193304));
#12344=CARTESIAN_POINT('Origin',(0.,0.,46.4896150285955));
#12345=CARTESIAN_POINT('',(-4.08499869890724,-0.00326035675198677,52.1146150285711));
#12346=CARTESIAN_POINT('Ctrl Pts',(-2.31338095599002,-3.36682247118299,
51.0573853382455));
#12347=CARTESIAN_POINT('Ctrl Pts',(-2.21485531346751,-3.43452052982407,
51.0631908707828));
#12348=CARTESIAN_POINT('Ctrl Pts',(-2.11333489385848,-3.49790437700326,
51.0689964033201));
#12349=CARTESIAN_POINT('Ctrl Pts',(-2.00923758994844,-3.55671046152736,
51.0748019358575));
#12350=CARTESIAN_POINT('Ctrl Pts',(-1.90513465637732,-3.61551972632908,
51.0806077823624));
#12351=CARTESIAN_POINT('Ctrl Pts',(-1.79845491668258,-3.66975053568956,
51.0864136288673));
#12352=CARTESIAN_POINT('Ctrl Pts',(-1.6896416456048,-3.71918487164028,51.0922194753723));
#12353=CARTESIAN_POINT('Ctrl Pts',(-1.58079687153331,-3.76863351953621,
51.0980270027526));
#12354=CARTESIAN_POINT('Ctrl Pts',(-1.46981770892226,-3.8132827636905,51.1038345301329));
#12355=CARTESIAN_POINT('Ctrl Pts',(-1.3571676249016,-3.85296263126428,51.1096420575131));
#12356=CARTESIAN_POINT('Ctrl Pts',(-1.24439571494977,-3.89268541080619,
51.1154558654696));
#12357=CARTESIAN_POINT('Ctrl Pts',(-1.12994966124609,-3.92742794946554,
51.121269673426));
#12358=CARTESIAN_POINT('Ctrl Pts',(-1.01430848479722,-3.9570700395202,51.1270834813825));
#12359=CARTESIAN_POINT('Ctrl Pts',(-0.898595034237535,-3.98673065546474,
51.1329009228872));
#12360=CARTESIAN_POINT('Ctrl Pts',(-0.781685371760786,-4.01128439002637,
51.138718364392));
#12361=CARTESIAN_POINT('Ctrl Pts',(-0.664067470212348,-4.03066240151737,
51.1445358058967));
#12362=CARTESIAN_POINT('Ctrl Pts',(-0.54627905099552,-4.05006850646433,
51.1503616812925));
#12363=CARTESIAN_POINT('Ctrl Pts',(-0.427780746829687,-4.06428385975495,
51.1561875566882));
#12364=CARTESIAN_POINT('Ctrl Pts',(-0.309064608487866,-4.07329155202279,
51.1620134320839));
#12365=CARTESIAN_POINT('Ctrl Pts',(-0.264187796497275,-4.07669661992695,
51.164215716613));
#12366=CARTESIAN_POINT('Ctrl Pts',(-0.219279844602496,-4.07935805925082,
51.166418001142));
#12367=CARTESIAN_POINT('Ctrl Pts',(-0.17436721939883,-4.08127689244422,
51.168620285671));
#12368=CARTESIAN_POINT('Ctrl Pts',(-0.0555365400593207,-4.08635377786066,
51.1744471320309));
#12369=CARTESIAN_POINT('Ctrl Pts',(0.0637050618138584,-4.08624461472206,
51.1802739783909));
#12370=CARTESIAN_POINT('Ctrl Pts',(0.182868281360663,-4.0809048251181,51.1861008247508));
#12371=CARTESIAN_POINT('Ctrl Pts',(0.301882461461882,-4.07557171407893,
51.1919203833758));
#12372=CARTESIAN_POINT('Ctrl Pts',(0.420818050366714,-4.06502100708473,
51.1977399420009));
#12373=CARTESIAN_POINT('Ctrl Pts',(0.539182790279408,-4.04926004581905,
51.2035595006259));
#12374=CARTESIAN_POINT('Ctrl Pts',(0.657430234058117,-4.03351470322347,
51.2093732922318));
#12375=CARTESIAN_POINT('Ctrl Pts',(0.775107552319402,-4.01256943182584,
51.2151870838376));
#12376=CARTESIAN_POINT('Ctrl Pts',(0.89172525873247,-3.9864835460514,51.2210008754435));
#12377=CARTESIAN_POINT('Ctrl Pts',(1.01197134723284,-3.95958603772334,51.2269955543088));
#12378=CARTESIAN_POINT('Ctrl Pts',(1.13109036807526,-3.92722281822845,51.2329902331742));
#12379=CARTESIAN_POINT('Ctrl Pts',(1.24855402613677,-3.88951640230732,51.2389849120395));
#12380=CARTESIAN_POINT('Ctrl Pts',(1.36234726760442,-3.85298820828882,51.2447922736601));
#12381=CARTESIAN_POINT('Ctrl Pts',(1.47458664040822,-3.81144590016996,51.2505996352808));
#12382=CARTESIAN_POINT('Ctrl Pts',(1.58480557157098,-3.76505196515501,51.2564069969014));
#12383=CARTESIAN_POINT('Ctrl Pts',(1.69500873526949,-3.71866466706443,51.2622135277449));
#12384=CARTESIAN_POINT('Ctrl Pts',(1.8031916564231,-3.66742728057848,51.2680200585884));
#12385=CARTESIAN_POINT('Ctrl Pts',(1.90890733784516,-3.61155060542157,51.2738265894319));
#12386=CARTESIAN_POINT('Ctrl Pts',(2.01463276006086,-3.55566878170813,51.2796336552974));
#12387=CARTESIAN_POINT('Ctrl Pts',(2.11789013001795,-3.49514700996815,51.285440721163));
#12388=CARTESIAN_POINT('Ctrl Pts',(2.21825724068107,-3.43024194688451,51.2912477870285));
#12389=CARTESIAN_POINT('Ctrl Pts',(2.31865720517891,-3.36531563799433,51.2970567537596));
#12390=CARTESIAN_POINT('Ctrl Pts',(2.41616468655407,-3.29600340549605,51.3028657204907));
#12391=CARTESIAN_POINT('Ctrl Pts',(2.51038716963343,-3.22260473197379,51.3086746872217));
#12392=CARTESIAN_POINT('Ctrl Pts',(2.60471317050794,-3.14912541879312,51.3144900359904));
#12393=CARTESIAN_POINT('Ctrl Pts',(2.69574664744501,-3.07155095401748,51.3203053847591));
#12394=CARTESIAN_POINT('Ctrl Pts',(2.78312873585002,-2.99022063394758,51.3261207335277));
#12395=CARTESIAN_POINT('Ctrl Pts',(2.87056836554361,-2.90883675769125,51.3319399117157));
#12396=CARTESIAN_POINT('Ctrl Pts',(2.95435153272342,-2.82369239045701,51.3377590899038));
#12397=CARTESIAN_POINT('Ctrl Pts',(3.03415789412681,-2.73516194648652,51.3435782680918));
#12398=CARTESIAN_POINT('Ctrl Pts',(3.11407652144017,-2.64650696418754,51.3494056322856));
#12399=CARTESIAN_POINT('Ctrl Pts',(3.19000691928114,-2.55445671187275,51.3552329964794));
#12400=CARTESIAN_POINT('Ctrl Pts',(3.26167041649538,-2.45941681993086,51.3610603606732));
#12401=CARTESIAN_POINT('Ctrl Pts',(3.27730007416623,-2.43868881984896,51.3623312965193));
#12402=CARTESIAN_POINT('Ctrl Pts',(3.29272693884235,-2.41781871297285,51.3636022323655));
#12403=CARTESIAN_POINT('Ctrl Pts',(3.30794840624843,-2.39681086896702,51.3648731682117));
#12404=CARTESIAN_POINT('Ctrl Pts',(3.37773264172279,-2.30049845086699,51.3706998920089));
#12405=CARTESIAN_POINT('Ctrl Pts',(3.44341813786752,-2.20098258530104,51.376526615806));
#12406=CARTESIAN_POINT('Ctrl Pts',(3.50469780021593,-2.0986467852313,51.3823533396032));
#12407=CARTESIAN_POINT('Ctrl Pts',(3.5659008220121,-1.99643897333789,51.3881727760996));
#12408=CARTESIAN_POINT('Ctrl Pts',(3.62270876242533,-1.89141858877044,51.393992212596));
#12409=CARTESIAN_POINT('Ctrl Pts',(3.67485620291266,-1.78400024885489,51.3998116490924));
#12410=CARTESIAN_POINT('Ctrl Pts',(3.72695197092691,-1.6766883488955,51.4056253191567));
#12411=CARTESIAN_POINT('Ctrl Pts',(3.77439624928288,-1.5669835855383,51.411438989221));
#12412=CARTESIAN_POINT('Ctrl Pts',(3.81696849768409,-1.45532693498308,51.4172526592853));
#12413=CARTESIAN_POINT('Ctrl Pts',(3.86086656961436,-1.34019297185826,51.4232473839297));
#12414=CARTESIAN_POINT('Ctrl Pts',(3.89958395878201,-1.22298393522567,51.4292421085742));
#12415=CARTESIAN_POINT('Ctrl Pts',(3.93293141597882,-1.10420807695236,51.4352368332187));
#12416=CARTESIAN_POINT('Ctrl Pts',(3.96523594665418,-0.989146879499215,
51.4410440755827));
#12417=CARTESIAN_POINT('Ctrl Pts',(3.99250130578342,-0.872615824488559,
51.4468513179468));
#12418=CARTESIAN_POINT('Ctrl Pts',(4.01460564908539,-0.755093691095127,
51.4526585603109));
#12419=CARTESIAN_POINT('Ctrl Pts',(4.03670683422612,-0.637588348693489,
51.4584649729644));
#12420=CARTESIAN_POINT('Ctrl Pts',(4.05364839468815,-0.519092610191553,
51.4642713856178));
#12421=CARTESIAN_POINT('Ctrl Pts',(4.06535958175131,-0.400095577409752,
51.4700777982713));
#12422=CARTESIAN_POINT('Ctrl Pts',(4.07707185035241,-0.281087555152209,
51.4758847471519));
#12423=CARTESIAN_POINT('Ctrl Pts',(4.08355274523143,-0.161578552421022,
51.4816916960324));
#12424=CARTESIAN_POINT('Ctrl Pts',(4.08478344148044,-0.0420622896098659,
51.487498644913));
#12425=CARTESIAN_POINT('Ctrl Pts',(4.08601454087451,0.0774931237154308,
51.4933074960036));
#12426=CARTESIAN_POINT('Ctrl Pts',(4.08199201701098,0.197055394294678,51.4991163470942));
#12427=CARTESIAN_POINT('Ctrl Pts',(4.07274914450126,0.316131943916218,51.5049251981848));
#12428=CARTESIAN_POINT('Ctrl Pts',(4.06349611297606,0.435339372819054,51.5107404338931));
#12429=CARTESIAN_POINT('Ctrl Pts',(4.04901131164756,0.554059608373962,51.5165556696015));
#12430=CARTESIAN_POINT('Ctrl Pts',(4.02937978590845,0.671806178084404,51.5223709053099));
#12431=CARTESIAN_POINT('Ctrl Pts',(4.00973532784342,0.789630313697542,51.528189971822));
#12432=CARTESIAN_POINT('Ctrl Pts',(3.9849374775445,0.906479108090121,51.5340090383342));
#12433=CARTESIAN_POINT('Ctrl Pts',(3.95512182112969,1.02187884801661,51.5398281048464));
#12434=CARTESIAN_POINT('Ctrl Pts',(3.92526420674824,1.13744098377875,51.5456553602173));
#12435=CARTESIAN_POINT('Ctrl Pts',(3.89037481199442,1.25154960673471,51.5514826155882));
#12436=CARTESIAN_POINT('Ctrl Pts',(3.85063824722395,1.3637485431765,51.5573098709591));
#12437=CARTESIAN_POINT('Ctrl Pts',(3.84196395913701,1.38824099498674,51.5585819308902));
#12438=CARTESIAN_POINT('Ctrl Pts',(3.83305886807873,1.41264253115848,51.5598539908213));
#12439=CARTESIAN_POINT('Ctrl Pts',(3.82392518819003,1.43694855688219,51.5611260507524));
#12440=CARTESIAN_POINT('Ctrl Pts',(3.78208928498747,1.54827986603781,51.5669525934814));
#12441=CARTESIAN_POINT('Ctrl Pts',(3.73532072835553,1.65795986297884,51.5727791362104));
#12442=CARTESIAN_POINT('Ctrl Pts',(3.68376995515531,1.76552086294528,51.5786056789395));
#12443=CARTESIAN_POINT('Ctrl Pts',(3.63228368614921,1.87294727452067,51.5844249310612));
#12444=CARTESIAN_POINT('Ctrl Pts',(3.57602727748281,1.97825959835997,51.5902441831829));
#12445=CARTESIAN_POINT('Ctrl Pts',(3.51520010096128,2.08100774871259,51.5960634353047));
#12446=CARTESIAN_POINT('Ctrl Pts',(3.45443323148049,2.18365402951865,51.6018769179349));
#12447=CARTESIAN_POINT('Ctrl Pts',(3.38910481626058,2.28374084551855,51.6076904005652));
#12448=CARTESIAN_POINT('Ctrl Pts',(3.31946097070129,2.38084099930903,51.6135038831955));
#12449=CARTESIAN_POINT('Ctrl Pts',(3.24764507016129,2.48096951649582,51.6194986769496));
#12450=CARTESIAN_POINT('Ctrl Pts',(3.17124033780107,2.57792162304733,51.6254934707036));
#12451=CARTESIAN_POINT('Ctrl Pts',(3.09056630564523,2.67125904966374,51.6314882644577));
#12452=CARTESIAN_POINT('Ctrl Pts',(3.01241882673005,2.76167333023932,51.637295312971));
#12453=CARTESIAN_POINT('Ctrl Pts',(2.93026575552348,2.84869563009802,51.6431023614844));
#12454=CARTESIAN_POINT('Ctrl Pts',(2.84443918786769,2.93196021571279,51.6489094099977));
#12455=CARTESIAN_POINT('Ctrl Pts',(2.75862491330545,3.0152128751913,51.6547156267571));
#12456=CARTESIAN_POINT('Ctrl Pts',(2.6691384813639,3.09470860694659,51.6605218435164));
#12457=CARTESIAN_POINT('Ctrl Pts',(2.57634878563552,3.17011859947769,51.6663280602758));
#12458=CARTESIAN_POINT('Ctrl Pts',(2.48355054971071,3.24553553260865,51.6721348114288));
#12459=CARTESIAN_POINT('Ctrl Pts',(2.38744876202428,3.31686572162996,51.6779415625819));
#12460=CARTESIAN_POINT('Ctrl Pts',(2.28844481299793,3.38382111493248,51.683748313735));
#12461=CARTESIAN_POINT('Ctrl Pts',(2.18940845936944,3.45079842314751,51.6895569654735));
#12462=CARTESIAN_POINT('Ctrl Pts',(2.08746839288154,3.51339785952447,51.695365617212));
#12463=CARTESIAN_POINT('Ctrl Pts',(1.98305379253874,3.57137545714501,51.7011742689505));
#12464=CARTESIAN_POINT('Ctrl Pts',(1.87852444961677,3.62941676711097,51.7069893038928));
#12465=CARTESIAN_POINT('Ctrl Pts',(1.77151550180268,3.68282590245674,51.7128043388352));
#12466=CARTESIAN_POINT('Ctrl Pts',(1.66247959503268,3.73140544515066,51.7186193737776));
#12467=CARTESIAN_POINT('Ctrl Pts',(1.55337187785856,3.78001698204443,51.7244382384676));
#12468=CARTESIAN_POINT('Ctrl Pts',(1.44223492164552,3.82379244249884,51.7302571031576));
#12469=CARTESIAN_POINT('Ctrl Pts',(1.32953861083212,3.86258360198282,51.7360759678477));
#12470=CARTESIAN_POINT('Ctrl Pts',(1.21668370371905,3.90142935184612,51.7419030213631));
#12471=CARTESIAN_POINT('Ctrl Pts',(1.10226545186857,3.93527668611693,51.7477300748784));
#12472=CARTESIAN_POINT('Ctrl Pts',(0.986766154322983,3.96402794600172,51.7535571283938));
#12473=CARTESIAN_POINT('Ctrl Pts',(0.961515211741925,3.97031366745555,51.7548310633602));
#12474=CARTESIAN_POINT('Ctrl Pts',(0.936212625199436,3.97635601021811,51.7561049983266));
#12475=CARTESIAN_POINT('Ctrl Pts',(0.91086347119859,3.98215428340441,51.7573789332929));
#12476=CARTESIAN_POINT('Ctrl Pts',(0.794922507767534,4.00867419722217,51.7632056069304));
#12477=CARTESIAN_POINT('Ctrl Pts',(0.677637888103198,4.03016865893983,51.7690322805679));
#12478=CARTESIAN_POINT('Ctrl Pts',(0.5594827134802,4.04650517030645,51.7748589542053));
#12479=CARTESIAN_POINT('Ctrl Pts',(0.44147534529509,4.06282124548346,51.7806783389545));
#12480=CARTESIAN_POINT('Ctrl Pts',(0.322599988750864,4.07399214894305,51.7864977237036));
#12481=CARTESIAN_POINT('Ctrl Pts',(0.203342057658757,4.07993590728912,51.7923171084527));
#12482=CARTESIAN_POINT('Ctrl Pts',(0.0842023303830821,4.08587377441342,
51.7981307252543));
#12483=CARTESIAN_POINT('Ctrl Pts',(-0.0353188120385766,4.08659478343787,
51.803944342056));
#12484=CARTESIAN_POINT('Ctrl Pts',(-0.154729263620538,4.08206857548712,
51.8097579588576));
#12485=CARTESIAN_POINT('Ctrl Pts',(-0.277860030136686,4.07740135040754,
51.8157527028983));
#12486=CARTESIAN_POINT('Ctrl Pts',(-0.400872658223365,4.06715453202206,
51.8217474469389));
#12487=CARTESIAN_POINT('Ctrl Pts',(-0.523225359481639,4.05135288801103,
51.8277421909796));
#12488=CARTESIAN_POINT('Ctrl Pts',(-0.641749994926215,4.03604563221225,
51.8335493766379));
#12489=CARTESIAN_POINT('Ctrl Pts',(-0.759654948262934,4.01552601377994,
51.8393565622962));
#12490=CARTESIAN_POINT('Ctrl Pts',(-0.876451953488757,3.98986929274954,
51.8451637479545));
#12491=CARTESIAN_POINT('Ctrl Pts',(-0.993232247399792,3.96421624268264,
51.8509701027208));
#12492=CARTESIAN_POINT('Ctrl Pts',(-1.10890451027023,3.93342763929747,51.856776457487));
#12493=CARTESIAN_POINT('Ctrl Pts',(-1.22299097464946,3.89762980231909,51.8625828122532));
#12494=CARTESIAN_POINT('Ctrl Pts',(-1.33708795306209,3.86182866626702,51.8683897021242));
#12495=CARTESIAN_POINT('Ctrl Pts',(-1.44959845329711,3.82101750085935,51.8741965919952));
#12496=CARTESIAN_POINT('Ctrl Pts',(-1.56006077978372,3.77537221521013,51.8800034818662));
#12497=CARTESIAN_POINT('Ctrl Pts',(-1.67055927107023,3.72971198552817,51.8858122728831));
#12498=CARTESIAN_POINT('Ctrl Pts',(-1.77900787829312,3.67921464363256,51.8916210639001));
#12499=CARTESIAN_POINT('Ctrl Pts',(-1.88496634784923,3.62410359502539,51.8974298549171));
#12500=CARTESIAN_POINT('Ctrl Pts',(-1.99104125621177,3.56893198434377,51.9032450292717));
#12501=CARTESIAN_POINT('Ctrl Pts',(-2.09462020294267,3.50913673530709,51.9090602036264));
#12502=CARTESIAN_POINT('Ctrl Pts',(-2.1952888154897,3.44498650455787,51.9148753779811));
#12503=CARTESIAN_POINT('Ctrl Pts',(-2.29602373029234,3.3807940232512,51.9206943823198));
#12504=CARTESIAN_POINT('Ctrl Pts',(-2.39384416028491,3.31224108133478,51.9265133866584));
#12505=CARTESIAN_POINT('Ctrl Pts',(-2.48836725530378,3.23963785055242,51.9323323909971));
#12506=CARTESIAN_POINT('Ctrl Pts',(-2.5830233571213,3.16693245718963,51.9381595834631));
#12507=CARTESIAN_POINT('Ctrl Pts',(-2.67437255274091,3.09016566156676,51.9439867759292));
#12508=CARTESIAN_POINT('Ctrl Pts',(-2.76206731988696,3.00968588401057,51.9498139683952));
#12509=CARTESIAN_POINT('Ctrl Pts',(-2.78121920958726,2.99210969476892,51.951086584208));
#12510=CARTESIAN_POINT('Ctrl Pts',(-2.80019694882373,2.97435654342491,51.9523592000208));
#12511=CARTESIAN_POINT('Ctrl Pts',(-2.81899717149045,2.95643027097357,51.9536318158336));
#12512=CARTESIAN_POINT('Ctrl Pts',(-2.90382455259405,2.87554618933505,51.9593739109389));
#12513=CARTESIAN_POINT('Ctrl Pts',(-2.98532230630841,2.79086082135747,51.9651160060442));
#12514=CARTESIAN_POINT('Ctrl Pts',(-3.0631239898746,2.70268318947203,51.9708581011494));
#12515=CARTESIAN_POINT('Ctrl Pts',(-3.14428289015889,2.61070060881995,51.9768479731253));
#12516=CARTESIAN_POINT('Ctrl Pts',(-3.22141920270685,2.51491785335467,51.9828378451012));
#12517=CARTESIAN_POINT('Ctrl Pts',(-3.29415604745111,2.41573196672174,51.9888277170772));
#12518=CARTESIAN_POINT('Ctrl Pts',(-3.36371623152867,2.32087785865119,51.9945559913611));
#12519=CARTESIAN_POINT('Ctrl Pts',(-3.42925281645865,2.22291197470652,52.0002842656451));
#12520=CARTESIAN_POINT('Ctrl Pts',(-3.49047521124661,2.12221766076736,52.006012539929));
#12521=CARTESIAN_POINT('Ctrl Pts',(-3.55166090817329,2.02158370490433,52.011737380577));
#12522=CARTESIAN_POINT('Ctrl Pts',(-3.60853733626655,1.91822492781679,52.0174622212251));
#12523=CARTESIAN_POINT('Ctrl Pts',(-3.66085668343508,1.81255436976349,52.0231870618731));
#12524=CARTESIAN_POINT('Ctrl Pts',(-3.71315785954413,1.70692051220625,52.0289099142237));
#12525=CARTESIAN_POINT('Ctrl Pts',(-3.76090491502834,1.5989768468548,52.0346327665744));
#12526=CARTESIAN_POINT('Ctrl Pts',(-3.80389594386372,1.48916105517743,52.0403556189251));
#12527=CARTESIAN_POINT('Ctrl Pts',(-3.84688287862381,1.37935572135907,52.0460779262832));
#12528=CARTESIAN_POINT('Ctrl Pts',(-3.88511453582612,1.26767900832715,52.0518002336414));
#12529=CARTESIAN_POINT('Ctrl Pts',(-3.91843742957534,1.15458785309,52.0575225409995));
#12530=CARTESIAN_POINT('Ctrl Pts',(-3.95177845910788,1.04143514867586,52.0632479626888));
#12531=CARTESIAN_POINT('Ctrl Pts',(-3.98020527092869,0.92686686891414,52.0689733843781));
#12532=CARTESIAN_POINT('Ctrl Pts',(-4.00361455484754,0.811354112710945,
52.0746988060675));
#12533=CARTESIAN_POINT('Ctrl Pts',(-4.02703139991122,0.695804046153278,
52.0804260770548));
#12534=CARTESIAN_POINT('Ctrl Pts',(-4.04542742176376,0.579309310973017,
52.0861533480421));
#12535=CARTESIAN_POINT('Ctrl Pts',(-4.0587508784753,0.462348684951092,52.0918806190295));
#12536=CARTESIAN_POINT('Ctrl Pts',(-4.07208789433607,0.345269029264654,
52.0976137186035));
#12537=CARTESIAN_POINT('Ctrl Pts',(-4.08034201096014,0.227722955682589,
52.1033468181775));
#12538=CARTESIAN_POINT('Ctrl Pts',(-4.08351353671633,0.110191630600995,
52.1090799177515));
#12539=CARTESIAN_POINT('Ctrl Pts',(-4.08453420312904,0.0723674774412442,
52.1109249546914));
#12540=CARTESIAN_POINT('Ctrl Pts',(-4.08502887233281,0.0345448325489773,
52.1127699916312));
#12541=CARTESIAN_POINT('Ctrl Pts',(-4.08499869890724,-0.00326035675198486,
52.1146150285711));
#12542=CARTESIAN_POINT('Ctrl Pts',(-4.08499869890684,-0.00326035725228949,
52.1146150285955));
#12543=CARTESIAN_POINT('Ctrl Pts',(-4.08485654869641,-0.181364589317125,
52.1233071921155));
#12544=CARTESIAN_POINT('Ctrl Pts',(-4.07306320787908,-0.359009021589031,
52.1319993556354));
#12545=CARTESIAN_POINT('Ctrl Pts',(-4.0498173705152,-0.534980621586747,
52.1406915191554));
#12546=CARTESIAN_POINT('Ctrl Pts',(-4.04162212857929,-0.597018818501584,
52.1437559122284));
#12547=CARTESIAN_POINT('Ctrl Pts',(-4.03200385599029,-0.658849401833403,
52.1468203053013));
#12548=CARTESIAN_POINT('Ctrl Pts',(-4.02097252192971,-0.720420001031497,
52.1498846983743));
#12549=CARTESIAN_POINT('Ctrl Pts',(-3.99999469520333,-0.83750623505584,
52.1557121265487));
#12550=CARTESIAN_POINT('Ctrl Pts',(-3.97386510412177,-0.95386180699246,
52.1615395547231));
#12551=CARTESIAN_POINT('Ctrl Pts',(-3.94264701505503,-1.06899930527464,
52.1673669828975));
#12552=CARTESIAN_POINT('Ctrl Pts',(-3.91142671509086,-1.18414495771379,
52.1731948237764));
#12553=CARTESIAN_POINT('Ctrl Pts',(-3.87511722923416,-1.29807195533858,
52.1790226646553));
#12554=CARTESIAN_POINT('Ctrl Pts',(-3.83383365485423,-1.41029943873882,
52.1848505055342));
#12555=CARTESIAN_POINT('Ctrl Pts',(-3.7926549498143,-1.52224183969914,52.1906635424182));
#12556=CARTESIAN_POINT('Ctrl Pts',(-3.7465275009288,-1.63249295561268,52.1964765793021));
#12557=CARTESIAN_POINT('Ctrl Pts',(-3.69561600635882,-1.74058821481259,
52.2022896161861));
#12558=CARTESIAN_POINT('Ctrl Pts',(-3.64473842267718,-1.84861147443174,
52.2080987811498));
#12559=CARTESIAN_POINT('Ctrl Pts',(-3.58908330420487,-1.95448136575595,
52.2139079461136));
#12560=CARTESIAN_POINT('Ctrl Pts',(-3.52886367089602,-2.05775270434283,
52.2197171110773));
#12561=CARTESIAN_POINT('Ctrl Pts',(-3.46866998087206,-2.16097955249345,
52.2255237733885));
#12562=CARTESIAN_POINT('Ctrl Pts',(-3.40391589366085,-2.26160972367424,
52.2313304356996));
#12563=CARTESIAN_POINT('Ctrl Pts',(-3.33486033893715,-2.35922265159183,
52.2371370980108));
#12564=CARTESIAN_POINT('Ctrl Pts',(-3.26539041267044,-2.45742131109496,
52.2429786035091));
#12565=CARTESIAN_POINT('Ctrl Pts',(-3.19156743003351,-2.55256603294785,
52.2488201090075));
#12566=CARTESIAN_POINT('Ctrl Pts',(-3.1136990161998,-2.6442585797377,52.2546616145059));
#12567=CARTESIAN_POINT('Ctrl Pts',(-3.03628664318898,-2.73541412387868,
52.2604689088929));
#12568=CARTESIAN_POINT('Ctrl Pts',(-2.95487639471255,-2.82315753412575,
52.26627620328));
#12569=CARTESIAN_POINT('Ctrl Pts',(-2.86981001746449,-2.90713182770586,
52.272083497667));
#12570=CARTESIAN_POINT('Ctrl Pts',(-2.78399194370129,-2.99184816750787,
52.277942108721));
#12571=CARTESIAN_POINT('Ctrl Pts',(-2.69445310243411,-3.07272814755913,
52.2838007197751));
#12572=CARTESIAN_POINT('Ctrl Pts',(-2.60158052560731,-3.14944499376966,
52.2896593308291));
#12573=CARTESIAN_POINT('Ctrl Pts',(-2.50870794878052,-3.22616183998019,
52.2955179418831));
#12574=CARTESIAN_POINT('Ctrl Pts',(-2.41250198808257,-3.2987153137835,52.3013765529371));
#12575=CARTESIAN_POINT('Ctrl Pts',(-2.31338095599003,-3.36682247118298,
52.3072351639912));
#12576=CARTESIAN_POINT('',(-4.08499847832697,0.00352591354478465,52.0103849713646));
#12577=CARTESIAN_POINT('Ctrl Pts',(-4.08499847832768,0.00352591272458481,
52.0103849714045));
#12578=CARTESIAN_POINT('Ctrl Pts',(-4.0851002980183,-0.114438799892165,
52.0161295062253));
#12579=CARTESIAN_POINT('Ctrl Pts',(-4.08008809612221,-0.232534395693748,
52.0218740410462));
#12580=CARTESIAN_POINT('Ctrl Pts',(-4.06995463095962,-0.350277464205617,
52.027618575867));
#12581=CARTESIAN_POINT('Ctrl Pts',(-4.05982760487945,-0.467945715534103,
52.0333594604525));
#12582=CARTESIAN_POINT('Ctrl Pts',(-4.04458582194297,-0.585261469241392,
52.039100345038));
#12583=CARTESIAN_POINT('Ctrl Pts',(-4.02427410712041,-0.701742766802956,
52.0448412296234));
#12584=CARTESIAN_POINT('Ctrl Pts',(-4.0039689110298,-0.818186681486533,
52.0505802717604));
#12585=CARTESIAN_POINT('Ctrl Pts',(-3.97859708867849,-0.933796260396595,
52.0563193138974));
#12586=CARTESIAN_POINT('Ctrl Pts',(-3.94825507161076,-1.04809679395555,
52.0620583560344));
#12587=CARTESIAN_POINT('Ctrl Pts',(-3.91791522923565,-1.16238913529297,
52.0677969868391));
#12588=CARTESIAN_POINT('Ctrl Pts',(-3.88260600808933,-1.27537221339099,
52.0735356176437));
#12589=CARTESIAN_POINT('Ctrl Pts',(-3.8424743059363,-1.38658436750864,52.0792742484484));
#12590=CARTESIAN_POINT('Ctrl Pts',(-3.80233547636011,-1.49781627299593,
52.0850138984386));
#12591=CARTESIAN_POINT('Ctrl Pts',(-3.75737260616839,-1.60727623597289,
52.0907535484288));
#12592=CARTESIAN_POINT('Ctrl Pts',(-3.70778125120284,-1.71452127231735,
52.096493198419));
#12593=CARTESIAN_POINT('Ctrl Pts',(-3.6581399257979,-1.82187437349674,52.102238631934));
#12594=CARTESIAN_POINT('Ctrl Pts',(-3.60386098019509,-1.92700771180435,
52.107984065449));
#12595=CARTESIAN_POINT('Ctrl Pts',(-3.54518661164281,-2.02950163553237,
52.113729498964));
#12596=CARTESIAN_POINT('Ctrl Pts',(-3.48647998938321,-2.13205190088108,
52.1194780907837));
#12597=CARTESIAN_POINT('Ctrl Pts',(-3.4233733573591,-2.23195950984396,52.1252266826033));
#12598=CARTESIAN_POINT('Ctrl Pts',(-3.35615204817023,-2.32883413526227,
52.130975274423));
#12599=CARTESIAN_POINT('Ctrl Pts',(-3.28882935454087,-2.42585486880931,
52.1367325363767));
#12600=CARTESIAN_POINT('Ctrl Pts',(-3.21737984600797,-2.51983315294746,
52.1424897983305));
#12601=CARTESIAN_POINT('Ctrl Pts',(-3.1421290247519,-2.61041188164085,52.1482470602843));
#12602=CARTESIAN_POINT('Ctrl Pts',(-3.09623099807221,-2.6656589186404,52.1517586095052));
#12603=CARTESIAN_POINT('Ctrl Pts',(-3.04891955031542,-2.71964195879564,
52.1552701587261));
#12604=CARTESIAN_POINT('Ctrl Pts',(-3.00027489997305,-2.77228705667211,
52.158781707947));
#12605=CARTESIAN_POINT('Ctrl Pts',(-2.91955433272997,-2.85964593649234,
52.1646087463371));
#12606=CARTESIAN_POINT('Ctrl Pts',(-2.8348867034544,-2.94361541160434,52.1704357847271));
#12607=CARTESIAN_POINT('Ctrl Pts',(-2.74658772409465,-3.0238189221335,52.1762628231172));
#12608=CARTESIAN_POINT('Ctrl Pts',(-2.65841192984707,-3.10391054146625,
52.1820817322583));
#12609=CARTESIAN_POINT('Ctrl Pts',(-2.56661516667542,-3.18024637993033,
52.1879006413995));
#12610=CARTESIAN_POINT('Ctrl Pts',(-2.47155169054511,-3.25248477951298,
52.1937195505407));
#12611=CARTESIAN_POINT('Ctrl Pts',(-2.41977587778372,-3.29182903666856,
52.1968887882168));
#12612=CARTESIAN_POINT('Ctrl Pts',(-2.36703170632116,-3.32995844726935,
52.2000580258928));
#12613=CARTESIAN_POINT('Ctrl Pts',(-2.31338095599002,-3.36682247118298,
52.2032272635689));
#12614=CARTESIAN_POINT('Ctrl Pts',(-2.31338095599002,-3.36682247118298,
50.953013989131));
#12615=CARTESIAN_POINT('Ctrl Pts',(-2.21503604400629,-3.43439634787205,
50.9588336971937));
#12616=CARTESIAN_POINT('Ctrl Pts',(-2.11384052331764,-3.49758034904679,
50.9646534052564));
#12617=CARTESIAN_POINT('Ctrl Pts',(-2.01023163741533,-3.55614872635193,
50.9704731133191));
#12618=CARTESIAN_POINT('Ctrl Pts',(-1.94619208453836,-3.59234921883563,
50.9740702131138));
#12619=CARTESIAN_POINT('Ctrl Pts',(-1.88123099978353,-3.62678730989976,
50.9776673129085));
#12620=CARTESIAN_POINT('Ctrl Pts',(-1.81545530512256,-3.65941894774326,
50.9812644127032));
#12621=CARTESIAN_POINT('Ctrl Pts',(-1.70889026982991,-3.71228637326225,
50.9870921742882));
#12622=CARTESIAN_POINT('Ctrl Pts',(-1.59984484477099,-3.76057898376045,
50.9929199358733));
#12623=CARTESIAN_POINT('Ctrl Pts',(-1.4887483140663,-3.80405749921906,50.9987476974583));
#12624=CARTESIAN_POINT('Ctrl Pts',(-1.37779067366811,-3.84748165884585,
51.0045681733109));
#12625=CARTESIAN_POINT('Ctrl Pts',(-1.26478740440378,-3.88610354726307,
51.0103886491636));
#12626=CARTESIAN_POINT('Ctrl Pts',(-1.15019154773323,-3.91973014422205,
51.0162091250162));
#12627=CARTESIAN_POINT('Ctrl Pts',(-1.03570921813449,-3.95332342820447,
51.022023834678));
#12628=CARTESIAN_POINT('Ctrl Pts',(-0.919637828923187,-3.98193115185382,
51.0278385443398));
#12629=CARTESIAN_POINT('Ctrl Pts',(-0.802448969845905,-4.00540892429141,
51.0336532540016));
#12630=CARTESIAN_POINT('Ctrl Pts',(-0.681639965355161,-4.02961196149287,
51.0396475890533));
#12631=CARTESIAN_POINT('Ctrl Pts',(-0.559643739567971,-4.04836279438894,
51.0456419241051));
#12632=CARTESIAN_POINT('Ctrl Pts',(-0.436992659478849,-4.06155911142034,
51.0516362591569));
#12633=CARTESIAN_POINT('Ctrl Pts',(-0.318148572653272,-4.07434582512819,
51.0574445347533));
#12634=CARTESIAN_POINT('Ctrl Pts',(-0.198690117475006,-4.08191769342196,
51.0632528103496));
#12635=CARTESIAN_POINT('Ctrl Pts',(-0.0791097938878756,-4.08423391109165,
51.069061085946));
#12636=CARTESIAN_POINT('Ctrl Pts',(0.0404533604251056,-4.08654979620014,
51.0748685275936));
#12637=CARTESIAN_POINT('Ctrl Pts',(0.160137940902236,-4.08361152357275,
51.0806759692411));
#12638=CARTESIAN_POINT('Ctrl Pts',(0.279449736580199,-4.0754303876677,51.0864834108886));
#12639=CARTESIAN_POINT('Ctrl Pts',(0.398772437464804,-4.06724850399937,
51.0922913833416));
#12640=CARTESIAN_POINT('Ctrl Pts',(0.517721879117753,-4.05382283216858,
51.0980993557946));
#12641=CARTESIAN_POINT('Ctrl Pts',(0.635807899724545,-4.03521663788301,
51.1039073282475));
#12642=CARTESIAN_POINT('Ctrl Pts',(0.753932461133397,-4.0166043709256,51.109717196301));
#12643=CARTESIAN_POINT('Ctrl Pts',(0.871192638594963,-3.99280828218478,
51.1155270643544));
#12644=CARTESIAN_POINT('Ctrl Pts',(0.987108027432526,-3.96394282781403,
51.1213369324079));
#12645=CARTESIAN_POINT('Ctrl Pts',(1.10315050066471,-3.93504572666341,51.1271531701381));
#12646=CARTESIAN_POINT('Ctrl Pts',(1.21784484664755,-3.90106826487509,51.1329694078684));
#12647=CARTESIAN_POINT('Ctrl Pts',(1.33072525776886,-3.86217494274094,51.1387856455987));
#12648=CARTESIAN_POINT('Ctrl Pts',(1.44367986835026,-3.82325605493535,51.1446057065051));
#12649=CARTESIAN_POINT('Ctrl Pts',(1.55481779108012,-3.77941502048066,51.1504257674115));
#12650=CARTESIAN_POINT('Ctrl Pts',(1.66369416928531,-3.7308640703041,51.156245828318));
#12651=CARTESIAN_POINT('Ctrl Pts',(1.77272339024437,-3.68224496336984,51.1620740595379));
#12652=CARTESIAN_POINT('Ctrl Pts',(1.87948436703941,-3.62890292608085,51.1679022907578));
#12653=CARTESIAN_POINT('Ctrl Pts',(1.98355765725178,-3.57109563304566,51.1737305219776));
#12654=CARTESIAN_POINT('Ctrl Pts',(2.00609748327204,-3.55857593346611,51.1749927797331));
#12655=CARTESIAN_POINT('Ctrl Pts',(2.02851135483631,-3.54584694786113,51.1762550374885));
#12656=CARTESIAN_POINT('Ctrl Pts',(2.05079520308251,-3.53291155210738,51.1775172952439));
#12657=CARTESIAN_POINT('Ctrl Pts',(2.15367449828829,-3.47319186708479,51.1833448429282));
#12658=CARTESIAN_POINT('Ctrl Pts',(2.25410615705943,-3.40887996998109,51.1891723906125));
#12659=CARTESIAN_POINT('Ctrl Pts',(2.3516538373978,-3.34020197429021,51.1949999382969));
#12660=CARTESIAN_POINT('Ctrl Pts',(2.44907980244682,-3.27160967168898,51.2008202146483));
#12661=CARTESIAN_POINT('Ctrl Pts',(2.54362861620005,-3.19866233919883,51.2066404909998));
#12662=CARTESIAN_POINT('Ctrl Pts',(2.63488942346093,-3.12163142060906,51.2124607673513));
#12663=CARTESIAN_POINT('Ctrl Pts',(2.72606004679311,-3.04467662397217,51.2182752921058));
#12664=CARTESIAN_POINT('Ctrl Pts',(2.81394881802279,-2.96364653099269,51.2240898168602));
#12665=CARTESIAN_POINT('Ctrl Pts',(2.8981752184825,-2.87885487702557,51.2299043416147));
#12666=CARTESIAN_POINT('Ctrl Pts',(2.98500734751445,-2.79144000712824,51.2358987514551));
#12667=CARTESIAN_POINT('Ctrl Pts',(3.06794645219371,-2.70002730027494,51.2418931612955));
#12668=CARTESIAN_POINT('Ctrl Pts',(3.146613551979,-2.60500444423846,51.2478875711359));
#12669=CARTESIAN_POINT('Ctrl Pts',(3.22283600547571,-2.51293450337202,51.2536956996489));
#12670=CARTESIAN_POINT('Ctrl Pts',(3.2950477569999,-2.41747580536904,51.259503828162));
#12671=CARTESIAN_POINT('Ctrl Pts',(3.36294316667186,-2.31901665749409,51.265311956675));
#12672=CARTESIAN_POINT('Ctrl Pts',(3.43082899567965,-2.2205714031067,51.2711192656079));
#12673=CARTESIAN_POINT('Ctrl Pts',(3.49439946281028,-2.11912687641255,51.2769265745408));
#12674=CARTESIAN_POINT('Ctrl Pts',(3.55339144620601,-2.01510154335457,51.2827338834737));
#12675=CARTESIAN_POINT('Ctrl Pts',(3.61238896987661,-1.91106644068205,51.2885417378043));
#12676=CARTESIAN_POINT('Ctrl Pts',(3.66680695376404,-1.80445040434974,51.2943495921348));
#12677=CARTESIAN_POINT('Ctrl Pts',(3.71642786354686,-1.69569718259261,51.3001574464653));
#12678=CARTESIAN_POINT('Ctrl Pts',(3.76606509555665,-1.58690818771532,51.3059672112227));
#12679=CARTESIAN_POINT('Ctrl Pts',(3.81090194606285,-1.47598097993228,51.31177697598));
#12680=CARTESIAN_POINT('Ctrl Pts',(3.85076896470228,-1.36337939711797,51.3175867407374));
#12681=CARTESIAN_POINT('Ctrl Pts',(3.89067984733628,-1.25065392354416,51.3234028977332));
#12682=CARTESIAN_POINT('Ctrl Pts',(3.92560984752966,-1.13625078225909,51.329219054729));
#12683=CARTESIAN_POINT('Ctrl Pts',(3.9554393111504,-1.02064923250156,51.3350352117248));
#12684=CARTESIAN_POINT('Ctrl Pts',(3.98528845015726,-0.90497143245822,51.3408552050328));
#12685=CARTESIAN_POINT('Ctrl Pts',(4.0100302680747,-0.78809404753574,51.3466751983408));
#12686=CARTESIAN_POINT('Ctrl Pts',(4.02959648159546,-0.670505179333855,
51.3524951916488));
#12687=CARTESIAN_POINT('Ctrl Pts',(4.04919022894369,-0.552750838563258,
51.3583233749262));
#12688=CARTESIAN_POINT('Ctrl Pts',(4.06359378695451,-0.434283419442727,
51.3641515582037));
#12689=CARTESIAN_POINT('Ctrl Pts',(4.07279079626367,-0.315594882515428,
51.3699797414812));
#12690=CARTESIAN_POINT('Ctrl Pts',(4.07478459526346,-0.289864661064443,
51.371243220249));
#12691=CARTESIAN_POINT('Ctrl Pts',(4.07653389700963,-0.264124041270327,
51.3725066990167));
#12692=CARTESIAN_POINT('Ctrl Pts',(4.07803885719302,-0.238378017492929,
51.3737701777845));
#12693=CARTESIAN_POINT('Ctrl Pts',(4.08497817797847,-0.119663967836718,
51.379596035885));
#12694=CARTESIAN_POINT('Ctrl Pts',(4.08674052243847,-0.000457205424181928,
51.3854218939854));
#12695=CARTESIAN_POINT('Ctrl Pts',(4.08327350447201,0.118753895417587,51.3912477520858));
#12696=CARTESIAN_POINT('Ctrl Pts',(4.07981083073444,0.237815622845764,51.397066310293));
#12697=CARTESIAN_POINT('Ctrl Pts',(4.07113183939052,0.356881273646933,51.4028848685002));
#12698=CARTESIAN_POINT('Ctrl Pts',(4.05723600945606,0.475458687556647,51.4087034267074));
#12699=CARTESIAN_POINT('Ctrl Pts',(4.0433539781617,0.593918353403358,51.4145162070523));
#12700=CARTESIAN_POINT('Ctrl Pts',(4.02426546143581,0.711890343989486,51.4203289873973));
#12701=CARTESIAN_POINT('Ctrl Pts',(4.00002194848,0.828884438072178,51.4261417677423));
#12702=CARTESIAN_POINT('Ctrl Pts',(3.97501822268229,0.94954715942479,51.4321368215999));
#12703=CARTESIAN_POINT('Ctrl Pts',(3.94453089160701,1.06916920351069,51.4381318754575));
#12704=CARTESIAN_POINT('Ctrl Pts',(3.90867410516127,1.18722017319524,51.4441269293152));
#12705=CARTESIAN_POINT('Ctrl Pts',(3.87394608817749,1.30155490551603,51.449933259241));
#12706=CARTESIAN_POINT('Ctrl Pts',(3.83418173070917,1.41441557471631,51.4557395891669));
#12707=CARTESIAN_POINT('Ctrl Pts',(3.78953605866919,1.52533322918174,51.4615459190928));
#12708=CARTESIAN_POINT('Ctrl Pts',(3.74489681890927,1.63623490329824,51.4673514124776));
#12709=CARTESIAN_POINT('Ctrl Pts',(3.69537781552154,1.74519374108193,51.4731569058624));
#12710=CARTESIAN_POINT('Ctrl Pts',(3.64118269125795,1.85175959802657,51.4789623992472));
#12711=CARTESIAN_POINT('Ctrl Pts',(3.58698261568811,1.95833519090596,51.4847684230261));
#12712=CARTESIAN_POINT('Ctrl Pts',(3.52810575477887,2.06251700463936,51.490574446805));
#12713=CARTESIAN_POINT('Ctrl Pts',(3.46480199459916,2.1638789564626,51.4963804705839));
#12714=CARTESIAN_POINT('Ctrl Pts',(3.40147754716054,2.26527403271534,51.5021883917338));
#12715=CARTESIAN_POINT('Ctrl Pts',(3.33372353927051,2.36384706853591,51.5079963128836));
#12716=CARTESIAN_POINT('Ctrl Pts',(3.26183314596471,2.45920099379574,51.5138042340335));
#12717=CARTESIAN_POINT('Ctrl Pts',(3.18986375518712,2.55465969966219,51.5196185372752));
#12718=CARTESIAN_POINT('Ctrl Pts',(3.11374915219426,2.64689190844894,51.5254328405168));
#12719=CARTESIAN_POINT('Ctrl Pts',(3.0338228506004,2.73553356974007,51.5312471437584));
#12720=CARTESIAN_POINT('Ctrl Pts',(2.95384392377078,2.82423359465157,51.5370652752653));
#12721=CARTESIAN_POINT('Ctrl Pts',(2.87004858564418,2.90933807383332,51.5428834067721));
#12722=CARTESIAN_POINT('Ctrl Pts',(2.78280606796309,2.99052092253303,51.548701538279));
#12723=CARTESIAN_POINT('Ctrl Pts',(2.69544070968695,3.07181807959645,51.5545278619237));
#12724=CARTESIAN_POINT('Ctrl Pts',(2.60461879405326,3.14918232216273,51.5603541855685));
#12725=CARTESIAN_POINT('Ctrl Pts',(2.5107414184921,3.22232874323342,51.5661805092132));
#12726=CARTESIAN_POINT('Ctrl Pts',(2.49010355513011,3.23840914422942,51.5674613595839));
#12727=CARTESIAN_POINT('Ctrl Pts',(2.46931812920197,3.25428587253981,51.5687422099545));
#12728=CARTESIAN_POINT('Ctrl Pts',(2.44838957246161,3.26995619259055,51.5700230603252));
#12729=CARTESIAN_POINT('Ctrl Pts',(2.35318136683388,3.34124362402462,51.575849905768));
#12730=CARTESIAN_POINT('Ctrl Pts',(2.25470573000445,3.40848286671879,51.5816767512108));
#12731=CARTESIAN_POINT('Ctrl Pts',(2.15334133041396,3.47136084478854,51.5875035966536));
#12732=CARTESIAN_POINT('Ctrl Pts',(2.05210370916048,3.53416018020341,51.5933231543526));
#12733=CARTESIAN_POINT('Ctrl Pts',(1.94798485517365,3.59260888757542,51.5991427120516));
#12734=CARTESIAN_POINT('Ctrl Pts',(1.84139519027646,3.64643507459364,51.6049622697506));
#12735=CARTESIAN_POINT('Ctrl Pts',(1.73491115290288,3.7002079212918,51.6107760604227));
#12736=CARTESIAN_POINT('Ctrl Pts',(1.62596153775807,3.74936717810325,51.6165898510948));
#12737=CARTESIAN_POINT('Ctrl Pts',(1.51498382552037,3.79368541242044,51.6224036417669));
#12738=CARTESIAN_POINT('Ctrl Pts',(1.4005531860078,3.83938255099654,51.6283983209793));
#12739=CARTESIAN_POINT('Ctrl Pts',(1.28396655721288,3.87993226317693,51.6343930001918));
#12740=CARTESIAN_POINT('Ctrl Pts',(1.1657291361518,3.91513736427303,51.6403876794042));
#12741=CARTESIAN_POINT('Ctrl Pts',(1.0511863349633,3.94924239514637,51.6461950400778));
#12742=CARTESIAN_POINT('Ctrl Pts',(0.935094790972726,3.97833172795182,51.6520024007515));
#12743=CARTESIAN_POINT('Ctrl Pts',(0.817931329882171,4.00227601991632,51.6578097614251));
#12744=CARTESIAN_POINT('Ctrl Pts',(0.700784629779372,4.02621688649563,51.6636162913184));
#12745=CARTESIAN_POINT('Ctrl Pts',(0.582566716966366,4.04501409443355,51.6694228212117));
#12746=CARTESIAN_POINT('Ctrl Pts',(0.463765540101661,4.05858922826815,51.6752293511049));
#12747=CARTESIAN_POINT('Ctrl Pts',(0.344953416769791,4.07216561293005,51.6810364160181));
#12748=CARTESIAN_POINT('Ctrl Pts',(0.225558327689244,4.08051892051422,51.6868434809312));
#12749=CARTESIAN_POINT('Ctrl Pts',(0.106073654365429,4.08362258048532,51.6926505458443));
#12750=CARTESIAN_POINT('Ctrl Pts',(-0.0134501306549043,4.08672725639765,
51.6984595116219));
#12751=CARTESIAN_POINT('Ctrl Pts',(-0.133063150818387,4.08457885652801,
51.7042684773994));
#12752=CARTESIAN_POINT('Ctrl Pts',(-0.252272348793747,4.07720292137074,
51.7100774431769));
#12753=CARTESIAN_POINT('Ctrl Pts',(-0.371612516373126,4.0698188826164,51.7158927909951));
#12754=CARTESIAN_POINT('Ctrl Pts',(-0.490547568998258,4.05719587012279,
51.7217081388133));
#12755=CARTESIAN_POINT('Ctrl Pts',(-0.608589741591365,4.03941128463415,
51.7275234866315));
#12756=CARTESIAN_POINT('Ctrl Pts',(-0.726709645230837,4.02161498795444,
51.7333426638698));
#12757=CARTESIAN_POINT('Ctrl Pts',(-0.843935098636929,3.9986504272913,51.7391618411081));
#12758=CARTESIAN_POINT('Ctrl Pts',(-0.959790300434298,3.97064573831414,
51.7449810183464));
#12759=CARTESIAN_POINT('Ctrl Pts',(-1.0758084792732,3.94260165428792,51.7508083815985));
#12760=CARTESIAN_POINT('Ctrl Pts',(-1.19045216910166,3.90950340407007,51.7566357448507));
#12761=CARTESIAN_POINT('Ctrl Pts',(-1.30326233582066,3.87152841705072,51.7624631081029));
#12762=CARTESIAN_POINT('Ctrl Pts',(-1.32786617502205,3.86324609196006,51.7637340530239));
#12763=CARTESIAN_POINT('Ctrl Pts',(-1.35238288136288,3.85473197179528,51.7650049979448));
#12764=CARTESIAN_POINT('Ctrl Pts',(-1.37680783803398,3.84598819253624,51.7662759428658));
#12765=CARTESIAN_POINT('Ctrl Pts',(-1.48878552586352,3.80590180886304,51.7721026665536));
#12766=CARTESIAN_POINT('Ctrl Pts',(-1.59918920479397,3.7608571761825,51.7779293902414));
#12767=CARTESIAN_POINT('Ctrl Pts',(-1.707548870435,3.71099742051597,51.7837561139291));
#12768=CARTESIAN_POINT('Ctrl Pts',(-1.81577301396521,3.66120002291683,51.7895755503123));
#12769=CARTESIAN_POINT('Ctrl Pts',(-1.92195786169754,3.60659964961025,51.7953949866954));
#12770=CARTESIAN_POINT('Ctrl Pts',(-2.02565024277944,3.547388630236,51.8012144230786));
#12771=CARTESIAN_POINT('Ctrl Pts',(-2.12923987585959,3.48823628261619,51.8070280930259));
#12772=CARTESIAN_POINT('Ctrl Pts',(-2.23034160361061,3.42448257910419,51.8128417629732));
#12773=CARTESIAN_POINT('Ctrl Pts',(-2.32852441122453,3.35636694452967,51.8186554329206));
#12774=CARTESIAN_POINT('Ctrl Pts',(-2.42976491953772,3.28612998924197,51.8246501576075));
#12775=CARTESIAN_POINT('Ctrl Pts',(-2.52790132295908,3.2112551532176,51.8306448822944));
#12776=CARTESIAN_POINT('Ctrl Pts',(-2.62249044523785,3.13205505453467,51.8366396069813));
#12777=CARTESIAN_POINT('Ctrl Pts',(-2.71412133320897,3.05533190503415,51.8424468492198));
#12778=CARTESIAN_POINT('Ctrl Pts',(-2.80242317725726,2.97455028346731,51.8482540914584));
#12779=CARTESIAN_POINT('Ctrl Pts',(-2.8870250743218,2.8900365430626,51.8540613336969));
#12780=CARTESIAN_POINT('Ctrl Pts',(-2.97161488383443,2.80553487761435,51.8598677462219));
#12781=CARTESIAN_POINT('Ctrl Pts',(-3.05250550927932,2.71730244194935,51.8656741587469));
#12782=CARTESIAN_POINT('Ctrl Pts',(-3.12936238979499,2.62570295984459,51.8714805712719));
#12783=CARTESIAN_POINT('Ctrl Pts',(-3.20622636807049,2.53409501849557,51.8772875200211));
#12784=CARTESIAN_POINT('Ctrl Pts',(-3.27905559863151,2.43911972487573,51.8830944687703));
#12785=CARTESIAN_POINT('Ctrl Pts',(-3.34755576718379,2.34117393322122,51.8889014175195));
#12786=CARTESIAN_POINT('Ctrl Pts',(-3.41607837463245,2.24319605704027,51.894710268476));
#12787=CARTESIAN_POINT('Ctrl Pts',(-3.48026886616441,2.14224608158912,51.9005191194325));
#12788=CARTESIAN_POINT('Ctrl Pts',(-3.53987657185992,2.03874933623466,51.906327970389));
#12789=CARTESIAN_POINT('Ctrl Pts',(-3.59954979347561,1.93513883571334,51.9121432059599));
#12790=CARTESIAN_POINT('Ctrl Pts',(-3.65462997162388,1.82897633158772,51.9179584415308));
#12791=CARTESIAN_POINT('Ctrl Pts',(-3.70491261208295,1.72071134616725,51.9237736771017));
#12792=CARTESIAN_POINT('Ctrl Pts',(-3.75522837636329,1.61237504090371,51.9295927434743));
#12793=CARTESIAN_POINT('Ctrl Pts',(-3.80074015378899,1.50193387212695,51.9354118098469));
#12794=CARTESIAN_POINT('Ctrl Pts',(-3.8412923675263,1.38985536916046,51.9412308762195));
#12795=CARTESIAN_POINT('Ctrl Pts',(-3.88190164819559,1.27761914419275,51.9470581314487));
#12796=CARTESIAN_POINT('Ctrl Pts',(-3.91753731438086,1.16374137413654,51.9528853866779));
#12797=CARTESIAN_POINT('Ctrl Pts',(-3.94809415420144,1.04870279372205,51.9587126419072));
#12798=CARTESIAN_POINT('Ctrl Pts',(-3.95476456209936,1.02359043721307,51.9599847030736));
#12799=CARTESIAN_POINT('Ctrl Pts',(-3.96119314504871,0.998422794177258,
51.96125676424));
#12800=CARTESIAN_POINT('Ctrl Pts',(-3.96737913600756,0.973204907083755,
51.9625288254064));
#12801=CARTESIAN_POINT('Ctrl Pts',(-4.00616627586605,0.815084774006025,
51.9705048497328));
#12802=CARTESIAN_POINT('Ctrl Pts',(-4.03551488037941,0.654566284093707,
51.9784808740591));
#12803=CARTESIAN_POINT('Ctrl Pts',(-4.05518763375965,0.492623847375249,
51.9864568983855));
#12804=CARTESIAN_POINT('Ctrl Pts',(-4.07361578512735,0.340926742296961,
51.9939283173962));
#12805=CARTESIAN_POINT('Ctrl Pts',(-4.08355402542618,0.187980020910348,
52.001399736407));
#12806=CARTESIAN_POINT('Ctrl Pts',(-4.08485340672103,0.0346070166231305,
52.0088711554177));
#12807=CARTESIAN_POINT('Ctrl Pts',(-4.08494116444249,0.0242484979634525,
52.0093757607333));
#12808=CARTESIAN_POINT('Ctrl Pts',(-4.08498953438796,0.0138880443175454,
52.0098803660489));
#12809=CARTESIAN_POINT('Ctrl Pts',(-4.08499847832697,0.00352591354478465,
52.0103849713646));
#12810=CARTESIAN_POINT('Ctrl Pts',(-3.3742051597689,0.272260201830434,50.0026433987789));
#12811=CARTESIAN_POINT('Ctrl Pts',(-3.46373108274233,-0.837262340205114,
50.0680610262924));
#12812=CARTESIAN_POINT('Ctrl Pts',(-2.46188142412267,-3.13325453455775,
50.1988962813195));
#12813=CARTESIAN_POINT('Ctrl Pts',(1.26137334667247,-3.78380856561343,50.3951491638602));
#12814=CARTESIAN_POINT('Ctrl Pts',(3.84893150453541,-1.03415529302938,50.5914020464008));
#12815=CARTESIAN_POINT('Ctrl Pts',(2.98722390906374,2.63934847059358,50.7876549289415));
#12816=CARTESIAN_POINT('Ctrl Pts',(-0.554316335019722,3.94781660436653,
50.9839078114821));
#12817=CARTESIAN_POINT('Ctrl Pts',(-3.59823642187141,1.71527100232214,51.1801606940228));
#12818=CARTESIAN_POINT('Ctrl Pts',(-3.41577519450092,-2.0549734213795,51.3764135765633));
#12819=CARTESIAN_POINT('Ctrl Pts',(-0.170140265370355,-3.98267722262975,
51.5726664591041));
#12820=CARTESIAN_POINT('Ctrl Pts',(3.22799613435637,-2.3388745938823,51.7689193416447));
#12821=CARTESIAN_POINT('Ctrl Pts',(3.73151821384908,1.40221729238016,51.9651722241853));
#12822=CARTESIAN_POINT('Ctrl Pts',(0.888849611894781,3.88592324617839,52.161425106726));
#12823=CARTESIAN_POINT('Ctrl Pts',(-2.75087059625197,2.88498188108543,52.3576779892666));
#12824=CARTESIAN_POINT('Ctrl Pts',(-3.92380027550394,-0.703009314092971,
52.5539308718072));
#12825=CARTESIAN_POINT('Ctrl Pts',(-1.57812882528071,-3.6605927578834,52.7501837543479));
#12826=CARTESIAN_POINT('Ctrl Pts',(2.18270082891269,-3.33560221219144,52.9464366368885));
#12827=CARTESIAN_POINT('Ctrl Pts',(3.98623241350175,-0.0194698709056399,
53.1426895194292));
#12828=CARTESIAN_POINT('Ctrl Pts',(2.21517984862058,3.31412217551562,53.3389424019698));
#12829=CARTESIAN_POINT('Ctrl Pts',(-1.54229618557997,3.67583317214676,53.5351952845106));
#12830=CARTESIAN_POINT('Ctrl Pts',(-3.91674528364537,0.741305469766164,
53.731448167051));
#12831=CARTESIAN_POINT('Ctrl Pts',(-2.77892183456758,-2.8579749427365,53.9277010495919));
#12832=CARTESIAN_POINT('Ctrl Pts',(0.850850924385935,-3.8944165145412,54.1239539321323));
#12833=CARTESIAN_POINT('Ctrl Pts',(3.71763807573328,-1.43860851900921,54.3202068146731));
#12834=CARTESIAN_POINT('Ctrl Pts',(3.25069860030425,2.30724639538179,54.5164596972136));
#12835=CARTESIAN_POINT('Ctrl Pts',(-0.131247725255445,3.98411864144676,
54.7127125797544));
#12836=CARTESIAN_POINT('Ctrl Pts',(-3.39549996047873,2.08830250185008,54.9089654622949));
#12837=CARTESIAN_POINT('Ctrl Pts',(-3.61489726723329,-1.68016221397994,
55.1052183448357));
#12838=CARTESIAN_POINT('Ctrl Pts',(-0.592698966878081,-3.94197098576313,
55.3014712273762));
#12839=CARTESIAN_POINT('Ctrl Pts',(2.96099171844794,-2.66888654013749,55.4977241099169));
#12840=CARTESIAN_POINT('Ctrl Pts',(3.85946510628054,0.997475016183975,55.6939769924575));
#12841=CARTESIAN_POINT('Ctrl Pts',(1.297030976099,3.76936837760147,55.8902298749982));
#12842=CARTESIAN_POINT('Ctrl Pts',(-2.42849289597393,3.16114687847811,56.0864827575388));
#12843=CARTESIAN_POINT('Ctrl Pts',(-3.97630842629188,-0.281777542149775,
56.2827356400795));
#12844=CARTESIAN_POINT('Ctrl Pts',(-1.95843925820106,-3.47202289852517,
56.4789885226201));
#12845=CARTESIAN_POINT('Ctrl Pts',(1.81562593482226,-3.54879273574328,56.6752414051608));
#12846=CARTESIAN_POINT('Ctrl Pts',(3.9615604099093,-0.443245024956087,56.8714942877014));
#12847=CARTESIAN_POINT('Ctrl Pts',(2.5550353209114,3.05977483891776,57.067747170242));
#12848=CARTESIAN_POINT('Ctrl Pts',(-1.14267304857574,3.81899544833241,57.2640000527827));
#12849=CARTESIAN_POINT('Ctrl Pts',(-3.81570893955738,1.15359885362914,57.4602529353233));
#12850=CARTESIAN_POINT('Ctrl Pts',(-3.06707588158816,-2.54626696652778,
57.656505817864));
#12851=CARTESIAN_POINT('Ctrl Pts',(0.431905572125819,-3.962813176837,57.8527587004047));
#12852=CARTESIAN_POINT('Ctrl Pts',(3.54357932256467,-1.82577519870519,58.0490115829453));
#12853=CARTESIAN_POINT('Ctrl Pts',(3.47761850079261,1.94849240971066,58.2452644654859));
#12854=CARTESIAN_POINT('Ctrl Pts',(0.293148588013416,3.97548807326636,58.4415173480266));
#12855=CARTESIAN_POINT('Ctrl Pts',(-3.15416563634503,2.43752590710906,58.6377702305672));
#12856=CARTESIAN_POINT('Ctrl Pts',(-3.77310016312419,-1.28622732383755,
58.8340231131078));
#12857=CARTESIAN_POINT('Ctrl Pts',(-1.00844788781245,-3.85661364405493,
59.0302759956485));
#12858=CARTESIAN_POINT('Ctrl Pts',(2.6602618623872,-2.96857992693771,59.2265288781891));
#12859=CARTESIAN_POINT('Ctrl Pts',(3.94392822706054,0.581336976956441,59.4227817607298));
#12860=CARTESIAN_POINT('Ctrl Pts',(1.68994917986025,3.61022697369519,59.6190346432704));
#12861=CARTESIAN_POINT('Ctrl Pts',(-2.07747158823233,3.40115608239218,59.8152875258111));
#12862=CARTESIAN_POINT('Ctrl Pts',(-3.98594307013179,0.143275338329916,
60.0115404083517));
#12863=CARTESIAN_POINT('Ctrl Pts',(-2.3119444938318,-3.24546711309908,60.2077932908924));
#12864=CARTESIAN_POINT('Ctrl Pts',(0.17337489301873,-3.55926711365582,60.3386285459194));
#12865=CARTESIAN_POINT('Ctrl Pts',(1.21263345687891,-3.16052308597322,60.404046173433));
#12866=CARTESIAN_POINT('Ctrl Pts',(-3.60785736139254,0.291113292428083,
49.8673058081045));
#12867=CARTESIAN_POINT('Ctrl Pts',(-3.70358264925775,-0.895239902286395,
49.932723435618));
#12868=CARTESIAN_POINT('Ctrl Pts',(-2.63235831798232,-3.3502217270022,50.0635586906451));
#12869=CARTESIAN_POINT('Ctrl Pts',(1.34871914977698,-4.04582440638657,50.2598115731858));
#12870=CARTESIAN_POINT('Ctrl Pts',(4.11545688676643,-1.10576702070916,50.4560644557264));
#12871=CARTESIAN_POINT('Ctrl Pts',(3.19407897864206,2.82211435227708,50.652317338267));
#12872=CARTESIAN_POINT('Ctrl Pts',(-0.592700851058509,4.2211894425729,50.8485702208078));
#12873=CARTESIAN_POINT('Ctrl Pts',(-3.84740202447223,1.83404767033637,51.0448231033483));
#12874=CARTESIAN_POINT('Ctrl Pts',(-3.65230597928024,-2.19727332356336,
51.241075985889));
#12875=CARTESIAN_POINT('Ctrl Pts',(-0.181921898586555,-4.25846403977975,
51.4373288684296));
#12876=CARTESIAN_POINT('Ctrl Pts',(3.45152385952784,-2.50083368418836,51.6335817509703));
#12877=CARTESIAN_POINT('Ctrl Pts',(3.98991312606725,1.49931605846165,51.829834633511));
#12878=CARTESIAN_POINT('Ctrl Pts',(0.950399416633318,4.15501018038018,52.0260875160515));
#12879=CARTESIAN_POINT('Ctrl Pts',(-2.94135900485841,3.08475703886098,52.2223403985922));
#12880=CARTESIAN_POINT('Ctrl Pts',(-4.19551006482977,-0.751690311904906,
52.4185932811329));
#12881=CARTESIAN_POINT('Ctrl Pts',(-1.68740886517545,-3.91407632412441,
52.6148461636735));
#12882=CARTESIAN_POINT('Ctrl Pts',(2.33384541853099,-3.56658129132739,52.8110990462142));
#12883=CARTESIAN_POINT('Ctrl Pts',(4.2622654154968,-0.020818093075613,53.0073519287548));
#12884=CARTESIAN_POINT('Ctrl Pts',(2.36857349960355,3.54361383535649,53.2036048112954));
#12885=CARTESIAN_POINT('Ctrl Pts',(-1.64909493736103,3.93037208510725,53.399857693836));
#12886=CARTESIAN_POINT('Ctrl Pts',(-4.18796653884179,0.792638345772549,
53.5961105763767));
#12887=CARTESIAN_POINT('Ctrl Pts',(-2.97135269577556,-3.05587996212226,
53.7923634589173));
#12888=CARTESIAN_POINT('Ctrl Pts',(0.909769449586076,-4.16409157861594,
53.988616341458));
#12889=CARTESIAN_POINT('Ctrl Pts',(3.97507183571676,-1.53822725344444,54.1848692239986));
#12890=CARTESIAN_POINT('Ctrl Pts',(3.47579839382954,2.46701534079058,54.3811221065393));
#12891=CARTESIAN_POINT('Ctrl Pts',(-0.140336182688226,4.26000527193475,
54.5773749890799));
#12892=CARTESIAN_POINT('Ctrl Pts',(-3.63062675443846,2.23291032920782,54.7736278716206));
#12893=CARTESIAN_POINT('Ctrl Pts',(-3.86521657656367,-1.79650771811881,
54.9698807541612));
#12894=CARTESIAN_POINT('Ctrl Pts',(-0.633741349292258,-4.21493903481416,
55.1661336367019));
#12895=CARTESIAN_POINT('Ctrl Pts',(3.16603029827518,-2.85369783241513,55.3623865192425));
#12896=CARTESIAN_POINT('Ctrl Pts',(4.12671990451392,1.06654675976815,55.5586394017832));
#12897=CARTESIAN_POINT('Ctrl Pts',(1.38684594845247,4.03038428459433,55.7548922843238));
#12898=CARTESIAN_POINT('Ctrl Pts',(-2.59665774811071,3.38004552062906,55.9511451668644));
#12899=CARTESIAN_POINT('Ctrl Pts',(-4.25165422601242,-0.301289676111394,
56.147398049405));
#12900=CARTESIAN_POINT('Ctrl Pts',(-2.09405449875632,-3.71244864500931,
56.3436509319458));
#12901=CARTESIAN_POINT('Ctrl Pts',(1.9413518397122,-3.79453453167758,56.5399038144863));
#12902=CARTESIAN_POINT('Ctrl Pts',(4.23588495978454,-0.473938231514639,
56.736156697027));
#12903=CARTESIAN_POINT('Ctrl Pts',(2.73196280447852,3.27165381299732,56.9324095795677));
#12904=CARTESIAN_POINT('Ctrl Pts',(-1.22179926079279,4.08344786075023,57.1286624621083));
#12905=CARTESIAN_POINT('Ctrl Pts',(-4.07993377244917,1.23348164059026,57.3249153446489));
#12906=CARTESIAN_POINT('Ctrl Pts',(-3.27946042797683,-2.72258727145301,
57.5211682271896));
#12907=CARTESIAN_POINT('Ctrl Pts',(0.461813560242235,-4.2372244765502,57.7174211097302));
#12908=CARTESIAN_POINT('Ctrl Pts',(3.78896010741355,-1.95220390551107,57.9136739922709));
#12909=CARTESIAN_POINT('Ctrl Pts',(3.71843172365335,2.08341886492568,58.1099268748115));
#12910=CARTESIAN_POINT('Ctrl Pts',(0.313448128127004,4.25077706633721,58.3061797573521));
#12911=CARTESIAN_POINT('Ctrl Pts',(-3.37258085128358,2.60631626446532,58.5024326398928));
#12912=CARTESIAN_POINT('Ctrl Pts',(-4.03437448353951,-1.37529418011125,
58.6986855224334));
#12913=CARTESIAN_POINT('Ctrl Pts',(-1.07827946534055,-4.12367098825238,
58.8949384049742));
#12914=CARTESIAN_POINT('Ctrl Pts',(2.8444759251399,-3.17414396432785,59.0911912875147));
#12915=CARTESIAN_POINT('Ctrl Pts',(4.21703180839744,0.621592580311748,59.2874441700555));
#12916=CARTESIAN_POINT('Ctrl Pts',(1.80697239801379,3.86022288112327,59.4836970525959));
#12917=CARTESIAN_POINT('Ctrl Pts',(-2.22132941175433,3.63667454350762,59.6799499351367));
#12918=CARTESIAN_POINT('Ctrl Pts',(-4.26195603608509,0.153196666955191,
59.8762028176772));
#12919=CARTESIAN_POINT('Ctrl Pts',(-2.47203876653822,-3.47020464397426,
60.0724557002181));
#12920=CARTESIAN_POINT('Ctrl Pts',(0.185380513169834,-3.80573422454402,
60.203290955245));
#12921=CARTESIAN_POINT('Ctrl Pts',(1.2966041888132,-3.37937853262027,60.2687085827586));
#12922=CARTESIAN_POINT('Ctrl Pts',(-3.84150956301618,0.309966383025731,
49.7319682174301));
#12923=CARTESIAN_POINT('Ctrl Pts',(-3.94343421577317,-0.953217464367681,
49.7973858449436));
#12924=CARTESIAN_POINT('Ctrl Pts',(-2.80283521184197,-3.56718891944667,
49.9282210999707));
#12925=CARTESIAN_POINT('Ctrl Pts',(1.43606495288148,-4.30784024715974,50.1244739825114));
#12926=CARTESIAN_POINT('Ctrl Pts',(4.38198226899745,-1.17737874838892,50.3207268650521));
#12927=CARTESIAN_POINT('Ctrl Pts',(3.40093404822038,3.00488023396059,50.5169797475926));
#12928=CARTESIAN_POINT('Ctrl Pts',(-0.631085367097292,4.49456228077927,
50.7132326301334));
#12929=CARTESIAN_POINT('Ctrl Pts',(-4.09656762707307,1.9528243383506,50.9094855126739));
#12930=CARTESIAN_POINT('Ctrl Pts',(-3.88883676405956,-2.33957322574722,
51.1057383952146));
#12931=CARTESIAN_POINT('Ctrl Pts',(-0.193703531802759,-4.53425085692975,
51.3019912777552));
#12932=CARTESIAN_POINT('Ctrl Pts',(3.6750515846993,-2.66279277449443,51.4982441602959));
#12933=CARTESIAN_POINT('Ctrl Pts',(4.24830803828541,1.59641482454314,51.6944970428365));
#12934=CARTESIAN_POINT('Ctrl Pts',(1.01194922137185,4.42409711458196,51.8907499253772));
#12935=CARTESIAN_POINT('Ctrl Pts',(-3.13184741346485,3.28453219663654,52.0870028079178));
#12936=CARTESIAN_POINT('Ctrl Pts',(-4.46721985415561,-0.800371309716849,
52.2832556904585));
#12937=CARTESIAN_POINT('Ctrl Pts',(-1.79668890507018,-4.16755989036541,
52.4795085729991));
#12938=CARTESIAN_POINT('Ctrl Pts',(2.48499000814928,-3.79756037046334,52.6757614555397));
#12939=CARTESIAN_POINT('Ctrl Pts',(4.53829841749185,-0.0221663152455843,
52.8720143380803));
#12940=CARTESIAN_POINT('Ctrl Pts',(2.52196715058651,3.77310549519735,53.0682672206211));
#12941=CARTESIAN_POINT('Ctrl Pts',(-1.75589368914209,4.18491099806776,53.2645201031617));
#12942=CARTESIAN_POINT('Ctrl Pts',(-4.45918779403821,0.843971221778929,
53.4607729857023));
#12943=CARTESIAN_POINT('Ctrl Pts',(-3.16378355698353,-3.25378498150801,
53.6570258682431));
#12944=CARTESIAN_POINT('Ctrl Pts',(0.968687974786214,-4.4337666426907,53.8532787507835));
#12945=CARTESIAN_POINT('Ctrl Pts',(4.23250559570023,-1.63784598787967,54.0495316333243));
#12946=CARTESIAN_POINT('Ctrl Pts',(3.70089818735484,2.62678428619937,54.2457845158648));
#12947=CARTESIAN_POINT('Ctrl Pts',(-0.149424640121008,4.53589190242274,
54.4420373984056));
#12948=CARTESIAN_POINT('Ctrl Pts',(-3.86575354839818,2.37751815656555,54.6382902809461));
#12949=CARTESIAN_POINT('Ctrl Pts',(-4.11553588589404,-1.91285322225766,
54.8345431634869));
#12950=CARTESIAN_POINT('Ctrl Pts',(-0.674783731706433,-4.4879070838652,
55.0307960460274));
#12951=CARTESIAN_POINT('Ctrl Pts',(3.3710688781024,-3.03850912469279,55.2270489285682));
#12952=CARTESIAN_POINT('Ctrl Pts',(4.3939747027473,1.13561850335233,55.4233018111087));
#12953=CARTESIAN_POINT('Ctrl Pts',(1.47666092080595,4.29140019158721,55.6195546936494));
#12954=CARTESIAN_POINT('Ctrl Pts',(-2.76482260024748,3.59894416277999,55.8158075761901));
#12955=CARTESIAN_POINT('Ctrl Pts',(-4.52700002573295,-0.320801810073011,
56.0120604587307));
#12956=CARTESIAN_POINT('Ctrl Pts',(-2.22966973931158,-3.95287439149345,
56.2083133412713));
#12957=CARTESIAN_POINT('Ctrl Pts',(2.06707774460212,-4.04027632761189,56.4045662238119));
#12958=CARTESIAN_POINT('Ctrl Pts',(4.51020950965979,-0.504631438073187,
56.6008191063527));
#12959=CARTESIAN_POINT('Ctrl Pts',(2.90889028804564,3.48353278707687,56.7970719888932));
#12960=CARTESIAN_POINT('Ctrl Pts',(-1.30092547300982,4.34790027316804,56.993324871434));
#12961=CARTESIAN_POINT('Ctrl Pts',(-4.34415860534098,1.31336442755139,57.1895777539745));
#12962=CARTESIAN_POINT('Ctrl Pts',(-3.49184497436551,-2.89890757637825,
57.3858306365152));
#12963=CARTESIAN_POINT('Ctrl Pts',(0.491721548358648,-4.51163577626339,
57.5820835190559));
#12964=CARTESIAN_POINT('Ctrl Pts',(4.03434089226244,-2.07863261231695,57.7783364015964));
#12965=CARTESIAN_POINT('Ctrl Pts',(3.95924494651409,2.2183453201407,57.9745892841372));
#12966=CARTESIAN_POINT('Ctrl Pts',(0.333747668240588,4.52606605940804,58.1708421666777));
#12967=CARTESIAN_POINT('Ctrl Pts',(-3.59099606622211,2.77510662182156,58.3670950492184));
#12968=CARTESIAN_POINT('Ctrl Pts',(-4.29564880395483,-1.46436103638495,
58.563347931759));
#12969=CARTESIAN_POINT('Ctrl Pts',(-1.14811104286864,-4.39072833244981,
58.7596008142997));
#12970=CARTESIAN_POINT('Ctrl Pts',(3.02868998789261,-3.37970800171799,58.9558536968403));
#12971=CARTESIAN_POINT('Ctrl Pts',(4.49013538973434,0.661848183667063,59.152106579381));
#12972=CARTESIAN_POINT('Ctrl Pts',(1.92399561616732,4.11021878855135,59.3483594619216));
#12973=CARTESIAN_POINT('Ctrl Pts',(-2.36518723527633,3.87219300462306,59.5446123444623));
#12974=CARTESIAN_POINT('Ctrl Pts',(-4.53796900203841,0.163117995580461,
59.7408652270028));
#12975=CARTESIAN_POINT('Ctrl Pts',(-2.63213303924464,-3.69494217484943,
59.9371181095436));
#12976=CARTESIAN_POINT('Ctrl Pts',(0.197386133320944,-4.05220133543222,
60.0679533645706));
#12977=CARTESIAN_POINT('Ctrl Pts',(1.38057492074749,-3.59823397926732,60.1333709920842));
#12978=CARTESIAN_POINT('Ctrl Pts',(-4.07516176463982,0.32881947362338,49.5966306267557));
#12979=CARTESIAN_POINT('Ctrl Pts',(-4.18328578228859,-1.01119502644896,
49.6620482542693));
#12980=CARTESIAN_POINT('Ctrl Pts',(-2.97331210570162,-3.78415611189113,
49.7928835092963));
#12981=CARTESIAN_POINT('Ctrl Pts',(1.523410755986,-4.56985608793288,49.989136391837));
#12982=CARTESIAN_POINT('Ctrl Pts',(4.64850765122846,-1.2489904760687,50.1853892743776));
#12983=CARTESIAN_POINT('Ctrl Pts',(3.6077891177987,3.18764611564409,50.3816421569182));
#12984=CARTESIAN_POINT('Ctrl Pts',(-0.669469883136082,4.76793511898564,
50.5778950394589));
#12985=CARTESIAN_POINT('Ctrl Pts',(-4.34573322967388,2.07160100636482,50.7741479219996));
#12986=CARTESIAN_POINT('Ctrl Pts',(-4.12536754883888,-2.48187312793108,
50.9704008045402));
#12987=CARTESIAN_POINT('Ctrl Pts',(-0.205485165018958,-4.81003767407975,
51.1666536870808));
#12988=CARTESIAN_POINT('Ctrl Pts',(3.89857930987077,-2.8247518648005,51.3629065696215));
#12989=CARTESIAN_POINT('Ctrl Pts',(4.50670295050357,1.69351359062463,51.5591594521622));
#12990=CARTESIAN_POINT('Ctrl Pts',(1.07349902611038,4.69318404878375,51.7554123347027));
#12991=CARTESIAN_POINT('Ctrl Pts',(-3.32233582207128,3.48430735441209,51.9516652172434));
#12992=CARTESIAN_POINT('Ctrl Pts',(-4.73892964348144,-0.84905230752879,
52.1479180997841));
#12993=CARTESIAN_POINT('Ctrl Pts',(-1.90596894496492,-4.42104345660641,
52.3441709823247));
#12994=CARTESIAN_POINT('Ctrl Pts',(2.63613459776757,-4.02853944959931,52.5404238648654));
#12995=CARTESIAN_POINT('Ctrl Pts',(4.8143314194869,-0.0235145374155529,
52.736676747406));
#12996=CARTESIAN_POINT('Ctrl Pts',(2.67536080156949,4.0025971550382,52.9329296299466));
#12997=CARTESIAN_POINT('Ctrl Pts',(-1.86269244092313,4.43944991102827,53.1291825124873));
#12998=CARTESIAN_POINT('Ctrl Pts',(-4.73040904923462,0.895304097785309,
53.3254353950279));
#12999=CARTESIAN_POINT('Ctrl Pts',(-3.35621441819151,-3.45169000089377,
53.5216882775686));
#13000=CARTESIAN_POINT('Ctrl Pts',(1.02760649998635,-4.70344170676544,53.7179411601092));
#13001=CARTESIAN_POINT('Ctrl Pts',(4.48993935568372,-1.73746472231492,53.9141940426499));
#13002=CARTESIAN_POINT('Ctrl Pts',(3.92599798088014,2.78655323160816,54.1104469251905));
#13003=CARTESIAN_POINT('Ctrl Pts',(-0.158513097553788,4.81177853291072,
54.3066998077312));
#13004=CARTESIAN_POINT('Ctrl Pts',(-4.10088034235792,2.52212598392328,54.5029526902718));
#13005=CARTESIAN_POINT('Ctrl Pts',(-4.36585519522442,-2.02919872639653,
54.6992055728124));
#13006=CARTESIAN_POINT('Ctrl Pts',(-0.715826114120611,-4.76087513291625,
54.8954584553531));
#13007=CARTESIAN_POINT('Ctrl Pts',(3.57610745792964,-3.22332041697045,55.0917113378937));
#13008=CARTESIAN_POINT('Ctrl Pts',(4.66122950098068,1.20469024693651,55.2879642204344));
#13009=CARTESIAN_POINT('Ctrl Pts',(1.56647589315943,4.55241609858009,55.484217102975));
#13010=CARTESIAN_POINT('Ctrl Pts',(-2.93298745238425,3.81784280493093,55.6804699855157));
#13011=CARTESIAN_POINT('Ctrl Pts',(-4.80234582545348,-0.340313944034631,
55.8767228680562));
#13012=CARTESIAN_POINT('Ctrl Pts',(-2.36528497986683,-4.19330013797761,
56.0729757505969));
#13013=CARTESIAN_POINT('Ctrl Pts',(2.19280364949204,-4.28601812354619,56.2692286331376));
#13014=CARTESIAN_POINT('Ctrl Pts',(4.78453405953504,-0.53532464463174,56.4654815156782));
#13015=CARTESIAN_POINT('Ctrl Pts',(3.08581777161277,3.69541176115642,56.6617343982189));
#13016=CARTESIAN_POINT('Ctrl Pts',(-1.38005168522687,4.61235268558585,56.8579872807595));
#13017=CARTESIAN_POINT('Ctrl Pts',(-4.60838343823277,1.39324721451252,57.0542401633002));
#13018=CARTESIAN_POINT('Ctrl Pts',(-3.70422952075418,-3.0752278813035,57.2504930458408));
#13019=CARTESIAN_POINT('Ctrl Pts',(0.521629536475065,-4.78604707597658,
57.4467459283814));
#13020=CARTESIAN_POINT('Ctrl Pts',(4.27972167711132,-2.20506131912283,57.6429988109221));
#13021=CARTESIAN_POINT('Ctrl Pts',(4.20005816937483,2.35327177535572,57.8392516934627));
#13022=CARTESIAN_POINT('Ctrl Pts',(0.354047208354176,4.80135505247888,58.0355045760034));
#13023=CARTESIAN_POINT('Ctrl Pts',(-3.80941128116065,2.94389697917782,58.231757458544));
#13024=CARTESIAN_POINT('Ctrl Pts',(-4.55692312437015,-1.55342789265866,
58.4280103410846));
#13025=CARTESIAN_POINT('Ctrl Pts',(-1.21794262039674,-4.65778567664726,
58.6242632236253));
#13026=CARTESIAN_POINT('Ctrl Pts',(3.21290405064532,-3.58527203910813,58.8205161061659));
#13027=CARTESIAN_POINT('Ctrl Pts',(4.76323897107123,0.702103787022373,59.0167689887067));
#13028=CARTESIAN_POINT('Ctrl Pts',(2.04101883432086,4.36021469597944,59.2130218712472));
#13029=CARTESIAN_POINT('Ctrl Pts',(-2.50904505879833,4.10771146573851,59.4092747537879));
#13030=CARTESIAN_POINT('Ctrl Pts',(-4.81398196799173,0.173039324205733,
59.6055276363284));
#13031=CARTESIAN_POINT('Ctrl Pts',(-2.79222731195107,-3.9196797057246,59.8017805188692));
#13032=CARTESIAN_POINT('Ctrl Pts',(0.209391753472049,-4.29866844632042,
59.9326157738963));
#13033=CARTESIAN_POINT('Ctrl Pts',(1.46454565268177,-3.81708942591437,59.9980334014098));
#13034=CARTESIAN_POINT('Ctrl Pts',(1.46332546897508,-3.81390922438499,60.));
#13035=CARTESIAN_POINT('Ctrl Pts',(1.34436836356881,-3.84840020465489,60.));
#13036=CARTESIAN_POINT('Ctrl Pts',(1.22405644550263,-3.87694498383428,60.));
#13037=CARTESIAN_POINT('Ctrl Pts',(1.10278998189303,-3.89970205494259,60.));
#13038=CARTESIAN_POINT('Ctrl Pts',(0.979743769206862,-3.92279311679397,
60.));
#13039=CARTESIAN_POINT('Ctrl Pts',(0.855713935497655,-3.93992519841741,
60.));
#13040=CARTESIAN_POINT('Ctrl Pts',(0.731113253599479,-3.95120932990782,
60.));
#13041=CARTESIAN_POINT('Ctrl Pts',(0.606016724725583,-3.96253836646928,
60.));
#13042=CARTESIAN_POINT('Ctrl Pts',(0.480343917845818,-3.96797258676211,
60.));
#13043=CARTESIAN_POINT('Ctrl Pts',(0.354520267150776,-3.96757271750024,
60.));
#13044=CARTESIAN_POINT('Ctrl Pts',(0.236435009120947,-3.96719744095481,
60.));
#13045=CARTESIAN_POINT('Ctrl Pts',(0.118216376475947,-3.96168300047746,
60.));
#13046=CARTESIAN_POINT('Ctrl Pts',(0.000232491209287232,-3.95104119203084,
60.));
#13047=CARTESIAN_POINT('Ctrl Pts',(-0.0270686093560331,-3.94857871097302,
60.));
#13048=CARTESIAN_POINT('Ctrl Pts',(-0.0543570496058564,-3.9458415373458,
60.));
#13049=CARTESIAN_POINT('Ctrl Pts',(-0.0816280901417187,-3.94282955007168,
60.));
#13050=CARTESIAN_POINT('Ctrl Pts',(-0.0980670002502211,-3.94101393221939,
60.));
#13051=CARTESIAN_POINT('Ctrl Pts',(-0.11448987603851,-3.93909952500333,
60.));
#13052=CARTESIAN_POINT('Ctrl Pts',(-0.130895119287348,-3.93708671595757,
60.));
#13053=CARTESIAN_POINT('Ctrl Pts',(-0.253258278521662,-3.922073608865,60.));
#13054=CARTESIAN_POINT('Ctrl Pts',(-0.374653550889227,-3.90158893120011,
60.));
#13055=CARTESIAN_POINT('Ctrl Pts',(-0.494687238785102,-3.87573365348574,
60.));
#13056=CARTESIAN_POINT('Ctrl Pts',(-0.614101450198027,-3.85001181111594,
60.));
#13057=CARTESIAN_POINT('Ctrl Pts',(-0.732168902791401,-3.81897433807138,
60.));
#13058=CARTESIAN_POINT('Ctrl Pts',(-0.848484137137308,-3.78267264792025,
60.));
#13059=CARTESIAN_POINT('Ctrl Pts',(-0.962109235726436,-3.7472105423279,
60.));
#13060=CARTESIAN_POINT('Ctrl Pts',(-1.07406285827702,-3.70672450335135,
60.));
#13061=CARTESIAN_POINT('Ctrl Pts',(-1.18393954190618,-3.66122205541169,
60.));
#13062=CARTESIAN_POINT('Ctrl Pts',(-1.27514614729463,-3.62345131391892,
60.));
#13063=CARTESIAN_POINT('Ctrl Pts',(-1.36492137435496,-3.5822233159453,60.));
#13064=CARTESIAN_POINT('Ctrl Pts',(-1.45301378049063,-3.53752319123988,
60.));
#13065=CARTESIAN_POINT('Ctrl Pts',(-1.47260001339677,-3.52758468357708,
60.));
#13066=CARTESIAN_POINT('Ctrl Pts',(-1.49210297812145,-3.51747447034406,
60.));
#13067=CARTESIAN_POINT('Ctrl Pts',(-1.51151976882622,-3.5071922786389,60.));
#13068=CARTESIAN_POINT('Ctrl Pts',(-1.52703531384485,-3.49897599765215,
60.));
#13069=CARTESIAN_POINT('Ctrl Pts',(-1.54248829386977,-3.4906538686883,60.));
#13070=CARTESIAN_POINT('Ctrl Pts',(-1.55787301693303,-3.48222851609215,
60.));
#13071=CARTESIAN_POINT('Ctrl Pts',(-1.66023918258982,-3.42616829089158,
60.));
#13072=CARTESIAN_POINT('Ctrl Pts',(-1.75964967742654,-3.36550766599683,
60.));
#13073=CARTESIAN_POINT('Ctrl Pts',(-1.85574301784674,-3.30029197211021,
60.));
#13074=CARTESIAN_POINT('Ctrl Pts',(-1.95138228900223,-3.2353844415369,60.));
#13075=CARTESIAN_POINT('Ctrl Pts',(-2.04373633146293,-3.16596450359091,
60.));
#13076=CARTESIAN_POINT('Ctrl Pts',(-2.13241450197746,-3.09203869892246,
60.));
#13077=CARTESIAN_POINT('Ctrl Pts',(-2.14806574423071,-3.07899117357412,
60.));
#13078=CARTESIAN_POINT('Ctrl Pts',(-2.16360238068116,-3.06580319830772,
60.));
#13079=CARTESIAN_POINT('Ctrl Pts',(-2.17902212861498,-3.05247469509659,
60.));
#13080=CARTESIAN_POINT('Ctrl Pts',(-2.26873549460814,-2.97492836347992,
60.));
#13081=CARTESIAN_POINT('Ctrl Pts',(-2.3544959880784,-2.89262699475134,60.));
#13082=CARTESIAN_POINT('Ctrl Pts',(-2.43611517004137,-2.80597529075037,
60.));
#13083=CARTESIAN_POINT('Ctrl Pts',(-2.48139017941949,-2.75790868904081,
60.));
#13084=CARTESIAN_POINT('Ctrl Pts',(-2.52539005963298,-2.70850304152369,
60.));
#13085=CARTESIAN_POINT('Ctrl Pts',(-2.56807609809654,-2.65782521592468,
60.));
#13086=CARTESIAN_POINT('Ctrl Pts',(-2.58354147909752,-2.63946436752084,
60.));
#13087=CARTESIAN_POINT('Ctrl Pts',(-2.59883435230139,-2.62093651679172,
60.));
#13088=CARTESIAN_POINT('Ctrl Pts',(-2.61395271713795,-2.60224481794349,
60.));
#13089=CARTESIAN_POINT('Ctrl Pts',(-2.62426766003826,-2.58949186427332,
60.));
#13090=CARTESIAN_POINT('Ctrl Pts',(-2.63450128189901,-2.57666264063865,
60.));
#13091=CARTESIAN_POINT('Ctrl Pts',(-2.64464422032148,-2.56376952712175,
60.));
#13092=CARTESIAN_POINT('Ctrl Pts',(-2.71647381695367,-2.47246392073068,
60.));
#13093=CARTESIAN_POINT('Ctrl Pts',(-2.78387371613041,-2.37781639842496,
60.));
#13094=CARTESIAN_POINT('Ctrl Pts',(-2.84672278780816,-2.28023988477505,
60.));
#13095=CARTESIAN_POINT('Ctrl Pts',(-2.90983003259932,-2.18226254368803,
60.));
#13096=CARTESIAN_POINT('Ctrl Pts',(-2.96834927587283,-2.08133117047599,
60.));
#13097=CARTESIAN_POINT('Ctrl Pts',(-3.02211025220274,-1.97784096098337,
60.));
#13098=CARTESIAN_POINT('Ctrl Pts',(-3.07502331645505,-1.87598298744577,
60.));
#13099=CARTESIAN_POINT('Ctrl Pts',(-3.12332713951146,-1.77164536324422,
60.));
#13100=CARTESIAN_POINT('Ctrl Pts',(-3.16681056806896,-1.66519640248744,
60.));
#13101=CARTESIAN_POINT('Ctrl Pts',(-3.20826497072667,-1.56371456841652,
60.));
#13102=CARTESIAN_POINT('Ctrl Pts',(-3.24533818764054,-1.46031316007369,
60.));
#13103=CARTESIAN_POINT('Ctrl Pts',(-3.27780325480812,-1.35531477701105,
60.));
#13104=CARTESIAN_POINT('Ctrl Pts',(-3.28326313294003,-1.33765646222576,
60.));
#13105=CARTESIAN_POINT('Ctrl Pts',(-3.28858985830397,-1.31996173909606,
60.));
#13106=CARTESIAN_POINT('Ctrl Pts',(-3.29378192183614,-1.30223481302024,
60.));
#13107=CARTESIAN_POINT('Ctrl Pts',(-3.32564288426071,-1.19345399358192,
60.));
#13108=CARTESIAN_POINT('Ctrl Pts',(-3.35244706188043,-1.08342861884937,
60.));
#13109=CARTESIAN_POINT('Ctrl Pts',(-3.37400268186516,-0.972525911804353,
60.));
#13110=CARTESIAN_POINT('Ctrl Pts',(-3.38941338834796,-0.89323851169108,
60.));
#13111=CARTESIAN_POINT('Ctrl Pts',(-3.40214040744648,-0.813502527884589,
60.));
#13112=CARTESIAN_POINT('Ctrl Pts',(-3.4120970300337,-0.733453791823358,
60.));
#13113=CARTESIAN_POINT('Ctrl Pts',(-3.41707534132731,-0.693429423792743,
60.));
#13114=CARTESIAN_POINT('Ctrl Pts',(-3.42136083200587,-0.653326908117905,
60.));
#13115=CARTESIAN_POINT('Ctrl Pts',(-3.42494130955714,-0.613163563714322,
60.));
#13116=CARTESIAN_POINT('Ctrl Pts',(-3.42733857929183,-0.586272634053829,
60.));
#13117=CARTESIAN_POINT('Ctrl Pts',(-3.42941992625259,-0.559352204490316,
60.));
#13118=CARTESIAN_POINT('Ctrl Pts',(-3.43118099378155,-0.532414906879469,
60.));
#13119=CARTESIAN_POINT('Ctrl Pts',(-3.43205019462101,-0.519119606550955,
60.));
#13120=CARTESIAN_POINT('Ctrl Pts',(-3.43284129656963,-0.505821333168536,
60.));
#13121=CARTESIAN_POINT('Ctrl Pts',(-3.43355375141007,-0.492524272718991,
60.));
#13122=CARTESIAN_POINT('Ctrl Pts',(-3.43931430586481,-0.385010874731565,
60.));
#13123=CARTESIAN_POINT('Ctrl Pts',(-3.43994303873128,-0.277485424520412,
60.));
#13124=CARTESIAN_POINT('Ctrl Pts',(-3.43524294624951,-0.170275803271761,
60.));
#13125=CARTESIAN_POINT('Ctrl Pts',(-3.43095381794618,-0.072440319678238,
60.));
#13126=CARTESIAN_POINT('Ctrl Pts',(-3.42222653673074,0.0251324780656352,
60.));
#13127=CARTESIAN_POINT('Ctrl Pts',(-3.40887510827288,0.122182273906181,
60.));
#13128=CARTESIAN_POINT('Ctrl Pts',(-3.40196952873072,0.172378032872603,
60.));
#13129=CARTESIAN_POINT('Ctrl Pts',(-3.39382628966267,0.222433662010737,
60.));
#13130=CARTESIAN_POINT('Ctrl Pts',(-3.38446664719617,0.272313465330584,
60.));
#13131=CARTESIAN_POINT('Ctrl Pts',(-3.3787688286016,0.272628438300531,50.));
#13132=CARTESIAN_POINT('Ctrl Pts',(-3.398044957201,0.167781606543633,50.));
#13133=CARTESIAN_POINT('Ctrl Pts',(-3.4119369975876,0.0622133010350053,
50.));
#13134=CARTESIAN_POINT('Ctrl Pts',(-3.42067227660546,-0.0437408776964314,
50.));
#13135=CARTESIAN_POINT('Ctrl Pts',(-3.4296483594719,-0.15261587601,50.));
#13136=CARTESIAN_POINT('Ctrl Pts',(-3.4331795612354,-0.261898933983832,
50.));
#13137=CARTESIAN_POINT('Ctrl Pts',(-3.43146110672633,-0.371245945305364,
50.));
#13138=CARTESIAN_POINT('Ctrl Pts',(-3.43059312612378,-0.426476435418754,
50.));
#13139=CARTESIAN_POINT('Ctrl Pts',(-3.42838504090139,-0.481723495358662,
50.));
#13140=CARTESIAN_POINT('Ctrl Pts',(-3.42485710615297,-0.536943839237519,
50.));
#13141=CARTESIAN_POINT('Ctrl Pts',(-3.42359637193536,-0.55667724759124,
50.));
#13142=CARTESIAN_POINT('Ctrl Pts',(-3.42216768464111,-0.576397395127722,
50.));
#13143=CARTESIAN_POINT('Ctrl Pts',(-3.42057240953287,-0.596101939689996,
50.));
#13144=CARTESIAN_POINT('Ctrl Pts',(-3.41158937887145,-0.707058681294052,
50.));
#13145=CARTESIAN_POINT('Ctrl Pts',(-3.39732801924954,-0.817522731174477,
50.));
#13146=CARTESIAN_POINT('Ctrl Pts',(-3.37799845802815,-0.927138977536138,
50.));
#13147=CARTESIAN_POINT('Ctrl Pts',(-3.35829521492687,-1.03887434106446,
50.));
#13148=CARTESIAN_POINT('Ctrl Pts',(-3.33332592513191,-1.14972960302005,
50.));
#13149=CARTESIAN_POINT('Ctrl Pts',(-3.3032601024926,-1.25933625667802,50.));
#13150=CARTESIAN_POINT('Ctrl Pts',(-3.29844646564883,-1.27688464152349,
50.));
#13151=CARTESIAN_POINT('Ctrl Pts',(-3.29350208061623,-1.29440102123175,
50.));
#13152=CARTESIAN_POINT('Ctrl Pts',(-3.28842751996456,-1.31188387913012,
50.));
#13153=CARTESIAN_POINT('Ctrl Pts',(-3.2834078609544,-1.32917759009288,50.));
#13154=CARTESIAN_POINT('Ctrl Pts',(-3.27826010256289,-1.3464408573239,50.));
#13155=CARTESIAN_POINT('Ctrl Pts',(-3.27298715730616,-1.36366443683881,
50.));
#13156=CARTESIAN_POINT('Ctrl Pts',(-3.23910916783017,-1.47432370165853,
50.));
#13157=CARTESIAN_POINT('Ctrl Pts',(-3.20012754844998,-1.58315475274442,
50.));
#13158=CARTESIAN_POINT('Ctrl Pts',(-3.15627292953829,-1.68978377711049,
50.));
#13159=CARTESIAN_POINT('Ctrl Pts',(-3.1120226081207,-1.79737492070572,50.));
#13160=CARTESIAN_POINT('Ctrl Pts',(-3.0628108296211,-1.90272499793219,50.));
#13161=CARTESIAN_POINT('Ctrl Pts',(-3.00882082981536,-2.00545305375488,
50.));
#13162=CARTESIAN_POINT('Ctrl Pts',(-2.95521231287092,-2.10745525307056,
50.));
#13163=CARTESIAN_POINT('Ctrl Pts',(-2.89689260366845,-2.20687322975469,
50.));
#13164=CARTESIAN_POINT('Ctrl Pts',(-2.83399143376612,-2.30332392463489,
50.));
#13165=CARTESIAN_POINT('Ctrl Pts',(-2.77196506401352,-2.39843322821104,
50.));
#13166=CARTESIAN_POINT('Ctrl Pts',(-2.70548349258012,-2.49065802267417,
50.));
#13167=CARTESIAN_POINT('Ctrl Pts',(-2.63462677786824,-2.57960868853371,
50.));
#13168=CARTESIAN_POINT('Ctrl Pts',(-2.62467602866062,-2.59210045831754,
50.));
#13169=CARTESIAN_POINT('Ctrl Pts',(-2.61463966718517,-2.60452658608384,
50.));
#13170=CARTESIAN_POINT('Ctrl Pts',(-2.60452587293078,-2.61687649059976,
50.));
#13171=CARTESIAN_POINT('Ctrl Pts',(-2.52905384554601,-2.70903501275091,
50.));
#13172=CARTESIAN_POINT('Ctrl Pts',(-2.44915924290189,-2.79709501168693,
50.));
#13173=CARTESIAN_POINT('Ctrl Pts',(-2.36503095553586,-2.88066875053339,
50.));
#13174=CARTESIAN_POINT('Ctrl Pts',(-2.3451491342261,-2.90041951682089,50.));
#13175=CARTESIAN_POINT('Ctrl Pts',(-2.32503063734273,-2.91991966440883,
50.));
#13176=CARTESIAN_POINT('Ctrl Pts',(-2.30467755267561,-2.93916394474508,
50.));
#13177=CARTESIAN_POINT('Ctrl Pts',(-2.22198064086081,-3.01735565769346,
50.));
#13178=CARTESIAN_POINT('Ctrl Pts',(-2.13541444818756,-3.09132566298283,
50.));
#13179=CARTESIAN_POINT('Ctrl Pts',(-2.04539122416378,-3.16106159088775,
50.));
#13180=CARTESIAN_POINT('Ctrl Pts',(-1.95303496262569,-3.23260479172319,
50.));
#13181=CARTESIAN_POINT('Ctrl Pts',(-1.85703964938763,-3.29969204706846,
50.));
#13182=CARTESIAN_POINT('Ctrl Pts',(-1.75780798754775,-3.36227497304928,
50.));
#13183=CARTESIAN_POINT('Ctrl Pts',(-1.70235630506146,-3.39724696158808,
50.));
#13184=CARTESIAN_POINT('Ctrl Pts',(-1.64589330109836,-3.43081172826972,
50.));
#13185=CARTESIAN_POINT('Ctrl Pts',(-1.58848467446361,-3.46295546999867,
50.));
#13186=CARTESIAN_POINT('Ctrl Pts',(-1.56669561237047,-3.47515541320397,
50.));
#13187=CARTESIAN_POINT('Ctrl Pts',(-1.54477030125963,-3.4871506118423,50.));
#13188=CARTESIAN_POINT('Ctrl Pts',(-1.52271223344434,-3.49894015606824,
50.));
#13189=CARTESIAN_POINT('Ctrl Pts',(-1.50575545848698,-3.50800317328095,
50.));
#13190=CARTESIAN_POINT('Ctrl Pts',(-1.48872551819598,-3.51694176326732,
50.));
#13191=CARTESIAN_POINT('Ctrl Pts',(-1.47163483009586,-3.52575038926294,
50.));
#13192=CARTESIAN_POINT('Ctrl Pts',(-1.36499561930288,-3.58071277104894,
50.));
#13193=CARTESIAN_POINT('Ctrl Pts',(-1.25587296134188,-3.63068347298158,
50.));
#13194=CARTESIAN_POINT('Ctrl Pts',(-1.14472361822858,-3.67565706105989,
50.));
#13195=CARTESIAN_POINT('Ctrl Pts',(-1.03178949125138,-3.7213528138587,50.));
#13196=CARTESIAN_POINT('Ctrl Pts',(-0.916762391257988,-3.7618900713334,
50.));
#13197=CARTESIAN_POINT('Ctrl Pts',(-0.800081831029844,-3.79722493418074,
50.));
#13198=CARTESIAN_POINT('Ctrl Pts',(-0.682285258005057,-3.83289776385845,
50.));
#13199=CARTESIAN_POINT('Ctrl Pts',(-0.56280265193181,-3.86326859172821,
50.));
#13200=CARTESIAN_POINT('Ctrl Pts',(-0.44205744347992,-3.88824777960903,
50.));
#13201=CARTESIAN_POINT('Ctrl Pts',(-0.334854840094098,-3.91042533850035,
50.));
#13202=CARTESIAN_POINT('Ctrl Pts',(-0.226656168903308,-3.92835240650093,
50.));
#13203=CARTESIAN_POINT('Ctrl Pts',(-0.117746834687938,-3.94193358936827,
50.));
#13204=CARTESIAN_POINT('Ctrl Pts',(-0.0928091818766533,-3.94504335792532,
50.));
#13205=CARTESIAN_POINT('Ctrl Pts',(-0.0678276535994453,-3.94792574054485,
50.));
#13206=CARTESIAN_POINT('Ctrl Pts',(-0.0428407696516749,-3.95057590881759,
50.));
#13207=CARTESIAN_POINT('Ctrl Pts',(0.0829695540103623,-3.96391965063228,
50.));
#13208=CARTESIAN_POINT('Ctrl Pts',(0.209038870700189,-3.97139872228523,
50.));
#13209=CARTESIAN_POINT('Ctrl Pts',(0.334905058101018,-3.972971048347,50.));
#13210=CARTESIAN_POINT('Ctrl Pts',(0.460908954032592,-3.97454509466992,
50.));
#13211=CARTESIAN_POINT('Ctrl Pts',(0.586710165776045,-3.97019977642533,
50.));
#13212=CARTESIAN_POINT('Ctrl Pts',(0.711866498333914,-3.95984534068554,
50.));
#13213=CARTESIAN_POINT('Ctrl Pts',(0.834749370138242,-3.94967899293778,
50.));
#13214=CARTESIAN_POINT('Ctrl Pts',(0.957011452282639,-3.9337200035174,50.));
#13215=CARTESIAN_POINT('Ctrl Pts',(1.07824174393589,-3.91183445670416,50.));
#13216=CARTESIAN_POINT('Ctrl Pts',(1.14882044428184,-3.89909297576425,50.));
#13217=CARTESIAN_POINT('Ctrl Pts',(1.21904950303075,-3.88434180939321,50.));
#13218=CARTESIAN_POINT('Ctrl Pts',(1.28884726169396,-3.86754634556837,50.));
#13219=CARTESIAN_POINT('Ctrl Pts',(1.34761180649662,-3.85340580860388,50.));
#13220=CARTESIAN_POINT('Ctrl Pts',(1.40607062746006,-3.83781606804309,50.));
#13221=CARTESIAN_POINT('Ctrl Pts',(1.46419354633185,-3.82081011676438,50.));
#13222=CARTESIAN_POINT('Origin',(-5.03504358328054E-16,0.,50.));
#13223=CARTESIAN_POINT('Ctrl Pts',(3.17505078219416,-2.57026798806821,50.));
#13224=CARTESIAN_POINT('Ctrl Pts',(3.24523509733765,-2.46687553038923,50.));
#13225=CARTESIAN_POINT('Ctrl Pts',(3.31015861353681,-2.36019756641044,50.));
#13226=CARTESIAN_POINT('Ctrl Pts',(3.36981505207394,-2.25066384020241,50.));
#13227=CARTESIAN_POINT('Ctrl Pts',(3.43040434804249,-2.13941731730403,50.));
#13228=CARTESIAN_POINT('Ctrl Pts',(3.48556070638999,-2.02522414499354,50.));
#13229=CARTESIAN_POINT('Ctrl Pts',(3.53522634918029,-1.90851946139768,50.));
#13230=CARTESIAN_POINT('Ctrl Pts',(3.5564460412567,-1.85865727678377,50.));
#13231=CARTESIAN_POINT('Ctrl Pts',(3.57666279615249,-1.80833652507169,50.));
#13232=CARTESIAN_POINT('Ctrl Pts',(3.59586921884357,-1.75759093627737,50.));
#13233=CARTESIAN_POINT('Ctrl Pts',(3.6065618017966,-1.72933989617423,50.));
#13234=CARTESIAN_POINT('Ctrl Pts',(3.61694279150167,-1.70095237454767,50.));
#13235=CARTESIAN_POINT('Ctrl Pts',(3.62700082864274,-1.67246314294838,50.));
#13236=CARTESIAN_POINT('Ctrl Pts',(3.66865222780369,-1.554486211616,50.));
#13237=CARTESIAN_POINT('Ctrl Pts',(3.70480266953197,-1.43468347218372,50.));
#13238=CARTESIAN_POINT('Ctrl Pts',(3.73541042587578,-1.31348080674658,50.));
#13239=CARTESIAN_POINT('Ctrl Pts',(3.76589523593952,-1.19276499231163,50.));
#13240=CARTESIAN_POINT('Ctrl Pts',(3.79088177393648,-1.0706595858572,50.));
#13241=CARTESIAN_POINT('Ctrl Pts',(3.81027760599455,-0.94758574640565,50.));
#13242=CARTESIAN_POINT('Ctrl Pts',(3.81807683061491,-0.898096736813369,
50.));
#13243=CARTESIAN_POINT('Ctrl Pts',(3.82497150996076,-0.848451218381541,
50.));
#13244=CARTESIAN_POINT('Ctrl Pts',(3.83095329809871,-0.798677085168631,
50.));
#13245=CARTESIAN_POINT('Ctrl Pts',(3.83306694698269,-0.781089527954901,
50.));
#13246=CARTESIAN_POINT('Ctrl Pts',(3.83506545254141,-0.763495503405024,
50.));
#13247=CARTESIAN_POINT('Ctrl Pts',(3.8369487712744,-0.745896401652321,50.));
#13248=CARTESIAN_POINT('Ctrl Pts',(3.84995310709515,-0.62437441744116,50.));
#13249=CARTESIAN_POINT('Ctrl Pts',(3.85747000929851,-0.502607486434189,
50.));
#13250=CARTESIAN_POINT('Ctrl Pts',(3.85946271601747,-0.380991411560717,
50.));
#13251=CARTESIAN_POINT('Ctrl Pts',(3.86143713309906,-0.260491564121916,
50.));
#13252=CARTESIAN_POINT('Ctrl Pts',(3.85798820094272,-0.140138992815084,
50.));
#13253=CARTESIAN_POINT('Ctrl Pts',(3.84903013630596,-0.0203256074983453,
50.));
#13254=CARTESIAN_POINT('Ctrl Pts',(3.84031877784156,0.0961881028453232,
50.));
#13255=CARTESIAN_POINT('Ctrl Pts',(3.82639733308781,0.21219256465117,50.));
#13256=CARTESIAN_POINT('Ctrl Pts',(3.80714191444518,0.327310135268585,50.));
#13257=CARTESIAN_POINT('Ctrl Pts',(3.78801864936847,0.441637632310381,50.));
#13258=CARTESIAN_POINT('Ctrl Pts',(3.76363432380651,0.555091014364022,50.));
#13259=CARTESIAN_POINT('Ctrl Pts',(3.73382433235031,0.667273537351628,50.));
#13260=CARTESIAN_POINT('Ctrl Pts',(3.72965489737509,0.682964173682061,50.));
#13261=CARTESIAN_POINT('Ctrl Pts',(3.72537940927025,0.6986290799777,50.));
#13262=CARTESIAN_POINT('Ctrl Pts',(3.72100102262887,0.714254781139606,50.));
#13263=CARTESIAN_POINT('Ctrl Pts',(3.68974751216623,0.825793129565523,50.));
#13264=CARTESIAN_POINT('Ctrl Pts',(3.65321090588756,0.935503458745713,50.));
#13265=CARTESIAN_POINT('Ctrl Pts',(3.61131430658357,1.04303117745521,50.));
#13266=CARTESIAN_POINT('Ctrl Pts',(3.60007235780076,1.07188366492544,50.));
#13267=CARTESIAN_POINT('Ctrl Pts',(3.58844422947595,1.10057889493759,50.));
#13268=CARTESIAN_POINT('Ctrl Pts',(3.5764278521007,1.12910974135774,50.));
#13269=CARTESIAN_POINT('Ctrl Pts',(3.53097968982238,1.23701868076171,50.));
#13270=CARTESIAN_POINT('Ctrl Pts',(3.47998089180808,1.3425786226534,50.));
#13271=CARTESIAN_POINT('Ctrl Pts',(3.42377585100192,1.44551956867172,50.));
#13272=CARTESIAN_POINT('Ctrl Pts',(3.36714914422034,1.54923280653062,50.));
#13273=CARTESIAN_POINT('Ctrl Pts',(3.30523702670668,1.65028821482483,50.));
#13274=CARTESIAN_POINT('Ctrl Pts',(3.23835550909232,1.74837178168865,50.));
#13275=CARTESIAN_POINT('Ctrl Pts',(3.20504349173018,1.79722476228559,50.));
#13276=CARTESIAN_POINT('Ctrl Pts',(3.17049818267377,1.84533984771772,50.));
#13277=CARTESIAN_POINT('Ctrl Pts',(3.13475621275442,1.89267404943633,50.));
#13278=CARTESIAN_POINT('Ctrl Pts',(3.1196368449191,1.91269709821035,50.));
#13279=CARTESIAN_POINT('Ctrl Pts',(3.10430260645072,1.93258129321551,50.));
#13280=CARTESIAN_POINT('Ctrl Pts',(3.08875851336575,1.95232029170191,50.));
#13281=CARTESIAN_POINT('Ctrl Pts',(3.07718604865985,1.96701583309276,50.));
#13282=CARTESIAN_POINT('Ctrl Pts',(3.06550133267884,1.9816256810886,50.));
#13283=CARTESIAN_POINT('Ctrl Pts',(3.05371157276739,1.99614166688898,50.));
#13284=CARTESIAN_POINT('Ctrl Pts',(2.98053827720831,2.08623531826787,50.));
#13285=CARTESIAN_POINT('Ctrl Pts',(2.90324873921887,2.17280900608232,50.));
#13286=CARTESIAN_POINT('Ctrl Pts',(2.82218516087522,2.25561271799166,50.));
#13287=CARTESIAN_POINT('Ctrl Pts',(2.74120372507107,2.33833252406665,50.));
#13288=CARTESIAN_POINT('Ctrl Pts',(2.65645508440711,2.41729050520046,50.));
#13289=CARTESIAN_POINT('Ctrl Pts',(2.5682492184672,2.49219595040595,50.));
#13290=CARTESIAN_POINT('Ctrl Pts',(2.48188236538523,2.56553968454615,50.));
#13291=CARTESIAN_POINT('Ctrl Pts',(2.3922001582028,2.63499841901754,50.));
#13292=CARTESIAN_POINT('Ctrl Pts',(2.29947556791442,2.70025360331428,50.));
#13293=CARTESIAN_POINT('Ctrl Pts',(2.22429001464763,2.75316564228494,50.));
#13294=CARTESIAN_POINT('Ctrl Pts',(2.14710368697748,2.80331320719412,50.));
#13295=CARTESIAN_POINT('Ctrl Pts',(2.06805826776658,2.85050151206886,50.));
#13296=CARTESIAN_POINT('Ctrl Pts',(2.04933268687684,2.86168025498405,50.));
#13297=CARTESIAN_POINT('Ctrl Pts',(2.03049854742624,2.87269513025456,50.));
#13298=CARTESIAN_POINT('Ctrl Pts',(2.01158369015662,2.88352879838473,50.));
#13299=CARTESIAN_POINT('Ctrl Pts',(1.91478828735083,2.93896930504972,50.));
#13300=CARTESIAN_POINT('Ctrl Pts',(1.81576602416327,2.98973918263213,50.));
#13301=CARTESIAN_POINT('Ctrl Pts',(1.71479982556319,3.03557905684995,50.));
#13302=CARTESIAN_POINT('Ctrl Pts',(1.61533953705197,3.08073522969034,50.));
#13303=CARTESIAN_POINT('Ctrl Pts',(1.51399215317973,3.1211076533205,50.));
#13304=CARTESIAN_POINT('Ctrl Pts',(1.41101601441157,3.15639999041054,50.));
#13305=CARTESIAN_POINT('Ctrl Pts',(1.3110481444873,3.1906613232372,50.));
#13306=CARTESIAN_POINT('Ctrl Pts',(1.2095446961283,3.22013515814445,50.));
#13307=CARTESIAN_POINT('Ctrl Pts',(1.1067400605449,3.24450171044004,50.));
#13308=CARTESIAN_POINT('Ctrl Pts',(1.05060132164677,3.25780760379209,50.));
#13309=CARTESIAN_POINT('Ctrl Pts',(0.994074592830348,3.26958966548783,50.));
#13310=CARTESIAN_POINT('Ctrl Pts',(0.937198714841526,3.27978922887549,50.));
#13311=CARTESIAN_POINT('Ctrl Pts',(0.887344887209746,3.28872952646787,50.));
#13312=CARTESIAN_POINT('Ctrl Pts',(0.837222776659118,3.29645381842423,50.));
#13313=CARTESIAN_POINT('Ctrl Pts',(0.786872907515106,3.30296842846219,50.));
#13314=CARTESIAN_POINT('Ctrl Pts',(3.17769854739391,-2.57241140768573,50.0019668001262));
#13315=CARTESIAN_POINT('Ctrl Pts',(4.02357137049521,-1.5275051251144,50.0673844276397));
#13316=CARTESIAN_POINT('Ctrl Pts',(4.59067653632725,1.44432493371321,50.1982196826668));
#13317=CARTESIAN_POINT('Ctrl Pts',(1.32303540089108,4.6318390767834,50.3944725652074));
#13318=CARTESIAN_POINT('Ctrl Pts',(-3.13133040812979,3.65559906892329,50.5907254477481));
#13319=CARTESIAN_POINT('Ctrl Pts',(-4.77752052222781,-0.593745130084182,
50.7869783302887));
#13320=CARTESIAN_POINT('Ctrl Pts',(-2.13966303858673,-4.31314779114456,
50.9832312128294));
#13321=CARTESIAN_POINT('Ctrl Pts',(2.41695513486635,-4.16356472240538,51.1794840953701));
#13322=CARTESIAN_POINT('Ctrl Pts',(4.80618344626051,-0.281002499380672,
51.3757369779108));
#13323=CARTESIAN_POINT('Ctrl Pts',(2.88556513840277,3.85385660156029,51.5719898604514));
#13324=CARTESIAN_POINT('Ctrl Pts',(-1.62263998902743,4.53268077196006,51.768242742992));
#13325=CARTESIAN_POINT('Ctrl Pts',(-4.67576771837635,1.14698163614136,51.9644956255326));
#13326=CARTESIAN_POINT('Ctrl Pts',(-3.53598465659234,-3.26729247706627,
52.1607485080733));
#13327=CARTESIAN_POINT('Ctrl Pts',(0.77463139421997,-4.75165975509162,52.3570013906139));
#13328=CARTESIAN_POINT('Ctrl Pts',(4.39060991305368,-1.97506951667604,52.5532542731545));
#13329=CARTESIAN_POINT('Ctrl Pts',(4.06938635955616,2.57263455668398,52.7495071556952));
#13330=CARTESIAN_POINT('Ctrl Pts',(0.0990119801423522,4.81337131475641,
52.9457600382359));
#13331=CARTESIAN_POINT('Ctrl Pts',(-3.96014959737916,2.73780316381413,53.1420129207765));
#13332=CARTESIAN_POINT('Ctrl Pts',(-4.46811663431751,-1.79284249136897,
53.3382658033171));
#13333=CARTESIAN_POINT('Ctrl Pts',(-0.969378574065539,-4.71578783221568,
53.5345186858578));
#13334=CARTESIAN_POINT('Ctrl Pts',(3.39863268272756,-3.40993345113973,53.7307715683984));
#13335=CARTESIAN_POINT('Ctrl Pts',(4.71897980158013,0.95371891518651,53.9270244509391));
#13336=CARTESIAN_POINT('Ctrl Pts',(1.80766469802749,4.46214056271427,54.1232773334797));
#13337=CARTESIAN_POINT('Ctrl Pts',(-2.72464196043686,3.96921608382251,54.3195302160203));
#13338=CARTESIAN_POINT('Ctrl Pts',(-4.81367381553503,-0.0830331856687988,
54.515783098561));
#13339=CARTESIAN_POINT('Ctrl Pts',(-2.58612825661705,-4.06082389990848,
54.7120359811016));
#13340=CARTESIAN_POINT('Ctrl Pts',(1.96048237593438,-4.3971421364971,54.9082888636423));
#13341=CARTESIAN_POINT('Ctrl Pts',(4.74906488512995,-0.790400422274602,
55.1045417461829));
#13342=CARTESIAN_POINT('Ctrl Pts',(3.27900690378524,3.52511898176996,55.3007946287236));
#13343=CARTESIAN_POINT('Ctrl Pts',(-1.13144290403263,4.67954987897574,55.4970475112642));
#13344=CARTESIAN_POINT('Ctrl Pts',(-4.52729116726062,1.63767664469671,55.6933003938049));
#13345=CARTESIAN_POINT('Ctrl Pts',(-3.86337062611881,-2.8727543434015,55.8895532763454));
#13346=CARTESIAN_POINT('Ctrl Pts',(0.264959644539609,-4.80709335455575,
56.0858061588862));
#13347=CARTESIAN_POINT('Ctrl Pts',(4.15569200315892,-2.4307558570938,56.2820590414267));
#13348=CARTESIAN_POINT('Ctrl Pts',(4.31988058961095,2.12531922976485,56.4783119239675));
#13349=CARTESIAN_POINT('Ctrl Pts',(0.610292135893617,4.77555167097707,56.6745648065081));
#13350=CARTESIAN_POINT('Ctrl Pts',(-3.6465650167766,3.14339200176368,56.8708176890487));
#13351=CARTESIAN_POINT('Ctrl Pts',(-4.63342916476401,-1.30754909347115,
57.0670705715894));
#13352=CARTESIAN_POINT('Ctrl Pts',(-1.46534692102897,-4.58596875244958,
57.26332345413));
#13353=CARTESIAN_POINT('Ctrl Pts',(3.01675902475045,-3.7520010357832,57.4595763366706));
#13354=CARTESIAN_POINT('Ctrl Pts',(4.79364012442147,0.44650673356943,57.6558292192113));
#13355=CARTESIAN_POINT('Ctrl Pts',(2.27190706938155,4.24461933186031,57.852082101752));
#13356=CARTESIAN_POINT('Ctrl Pts',(-2.28711553473289,4.23644034017381,58.0483349842925));
#13357=CARTESIAN_POINT('Ctrl Pts',(-4.79521384845463,0.429315466689967,
58.2445878668332));
#13358=CARTESIAN_POINT('Ctrl Pts',(-3.00327566838071,-3.76280558753283,
58.4408407493739));
#13359=CARTESIAN_POINT('Ctrl Pts',(1.48177178817488,-4.5806667508406,58.6370936319145));
#13360=CARTESIAN_POINT('Ctrl Pts',(4.63811714181827,-1.29095555776593,58.8333465144552));
#13361=CARTESIAN_POINT('Ctrl Pts',(3.6352112313189,3.15651723066099,59.0295993969958));
#13362=CARTESIAN_POINT('Ctrl Pts',(-0.627304473579594,4.77319939024576,
59.2258522795364));
#13363=CARTESIAN_POINT('Ctrl Pts',(-4.32769908146539,2.1100764079135,59.4221051620771));
#13364=CARTESIAN_POINT('Ctrl Pts',(-4.1465008886248,-2.44617374698532,59.6183580446177));
#13365=CARTESIAN_POINT('Ctrl Pts',(-0.248607397570823,-4.80695631761555,
59.8146109271585));
#13366=CARTESIAN_POINT('Ctrl Pts',(3.87543306135802,-2.8610093484926,60.0108638096989));
#13367=CARTESIAN_POINT('Ctrl Pts',(4.51789674603907,1.65944634992689,60.2071616790379));
#13368=CARTESIAN_POINT('Ctrl Pts',(2.2528534253199,3.66744558551292,60.3380419208631));
#13369=CARTESIAN_POINT('Ctrl Pts',(0.943870013894813,3.9779614512679,60.403504535175));
#13370=CARTESIAN_POINT('Ctrl Pts',(2.9951670455048,-2.42464845575103,49.8663796336412));
#13371=CARTESIAN_POINT('Ctrl Pts',(3.79245173650198,-1.43976306888344,49.9317972611547));
#13372=CARTESIAN_POINT('Ctrl Pts',(4.32698157899718,1.36136086539945,50.0626325161818));
#13373=CARTESIAN_POINT('Ctrl Pts',(1.24703837500101,4.36577968487308,50.2588853987225));
#13374=CARTESIAN_POINT('Ctrl Pts',(-2.95146235778382,3.44561628471545,50.4551382812631));
#13375=CARTESIAN_POINT('Ctrl Pts',(-4.50309298191142,-0.559639569497738,
50.6513911638038));
#13376=CARTESIAN_POINT('Ctrl Pts',(-2.01675776543231,-4.0653944777181,50.8476440463444));
#13377=CARTESIAN_POINT('Ctrl Pts',(2.27812181125624,-3.92440367214893,51.043896928885));
#13378=CARTESIAN_POINT('Ctrl Pts',(4.53010946702169,-0.264861318119594,
51.2401498114257));
#13379=CARTESIAN_POINT('Ctrl Pts',(2.7198141929761,3.63248562408825,51.4364026939663));
#13380=CARTESIAN_POINT('Ctrl Pts',(-1.52943325157104,4.27231717341537,51.632655576507));
#13381=CARTESIAN_POINT('Ctrl Pts',(-4.4071850031217,1.08109738766354,51.8289084590476));
#13382=CARTESIAN_POINT('Ctrl Pts',(-3.33287269351643,-3.07961457305647,
52.0251613415883));
#13383=CARTESIAN_POINT('Ctrl Pts',(0.730135470617217,-4.4787176938397,52.2214142241289));
#13384=CARTESIAN_POINT('Ctrl Pts',(4.13840706571432,-1.86161872836576,52.4176671066696));
#13385=CARTESIAN_POINT('Ctrl Pts',(3.83563504775033,2.42485878675501,52.6139199892101));
#13386=CARTESIAN_POINT('Ctrl Pts',(0.0933245918735013,4.53688445417833,
52.8101728717508));
#13387=CARTESIAN_POINT('Ctrl Pts',(-3.73267299979315,2.5805398753321,53.0064257542915));
#13388=CARTESIAN_POINT('Ctrl Pts',(-4.2114616912152,-1.68985908129423,53.2026786368321));
#13389=CARTESIAN_POINT('Ctrl Pts',(-0.913696096831058,-4.44490630498251,
53.3989315193728));
#13390=CARTESIAN_POINT('Ctrl Pts',(3.20341041142166,-3.21406204770251,53.5951844019134));
#13391=CARTESIAN_POINT('Ctrl Pts',(4.44791492310913,0.898935950920812,53.7914372844541));
#13392=CARTESIAN_POINT('Ctrl Pts',(1.70382987942474,4.20582889362266,53.9876901669947));
#13393=CARTESIAN_POINT('Ctrl Pts',(-2.56813467010359,3.74121869442359,54.1839430495353));
#13394=CARTESIAN_POINT('Ctrl Pts',(-4.5371695788841,-0.0782636419689434,
54.380195932076));
#13395=CARTESIAN_POINT('Ctrl Pts',(-2.43757738946658,-3.82756442790307,
54.5764488146166));
#13396=CARTESIAN_POINT('Ctrl Pts',(1.84786949363316,-4.14456406899824,54.7727016971573));
#13397=CARTESIAN_POINT('Ctrl Pts',(4.47627187688111,-0.744998703382836,
54.968954579698));
#13398=CARTESIAN_POINT('Ctrl Pts',(3.09065610652554,3.32263115843381,55.1652074622385));
#13399=CARTESIAN_POINT('Ctrl Pts',(-1.06645122231876,4.41074991106344,55.3614603447792));
#13400=CARTESIAN_POINT('Ctrl Pts',(-4.26723715523765,1.54360618045763,55.5577132273198));
#13401=CARTESIAN_POINT('Ctrl Pts',(-3.64145314961115,-2.70773926817054,
55.7539661098605));
#13402=CARTESIAN_POINT('Ctrl Pts',(0.249739987565699,-4.53096710889666,
55.9502189924011));
#13403=CARTESIAN_POINT('Ctrl Pts',(3.91698317303808,-2.29112980046708,56.1464718749418));
#13404=CARTESIAN_POINT('Ctrl Pts',(4.0717405347118,2.00323788528963,56.3427247574824));
#13405=CARTESIAN_POINT('Ctrl Pts',(0.575236091874863,4.501237224263,56.5389776400231));
#13406=CARTESIAN_POINT('Ctrl Pts',(-3.43710116130976,2.96283111640888,56.7352305225637));
#13407=CARTESIAN_POINT('Ctrl Pts',(-4.36727843594967,-1.23244162299672,
56.9314834051044));
#13408=CARTESIAN_POINT('Ctrl Pts',(-1.38117532001182,-4.32254421688825,
57.127736287645));
#13409=CARTESIAN_POINT('Ctrl Pts',(2.84347211681614,-3.53648078616334,57.3239891701857));
#13410=CARTESIAN_POINT('Ctrl Pts',(4.51828665134137,0.420858754862052,57.5202420527263));
#13411=CARTESIAN_POINT('Ctrl Pts',(2.14140551193621,4.00080239012195,57.7164949352669));
#13412=CARTESIAN_POINT('Ctrl Pts',(-2.15574038151357,3.99309321129347,57.9127478178076));
#13413=CARTESIAN_POINT('Ctrl Pts',(-4.5197699784388,0.404654978682567,58.1090007003482));
#13414=CARTESIAN_POINT('Ctrl Pts',(-2.83076326351899,-3.54666470916903,
58.3052535828889));
#13415=CARTESIAN_POINT('Ctrl Pts',(1.39665671954312,-4.31754676975549,58.5015064654295));
#13416=CARTESIAN_POINT('Ctrl Pts',(4.37169712896714,-1.21680124346688,58.6977593479701));
#13417=CARTESIAN_POINT('Ctrl Pts',(3.4263995533575,2.97520241358248,58.8940122305108));
#13418=CARTESIAN_POINT('Ctrl Pts',(-0.591271216806967,4.49902006186603,
59.0902651130514));
#13419=CARTESIAN_POINT('Ctrl Pts',(-4.07910992132878,1.98887063269826,59.2865179955921));
#13420=CARTESIAN_POINT('Ctrl Pts',(-3.90832000913077,-2.30566206494264,
59.4827708781327));
#13421=CARTESIAN_POINT('Ctrl Pts',(-0.234327036805779,-4.53083794355226,
59.6790237606734));
#13422=CARTESIAN_POINT('Ctrl Pts',(3.65282270149852,-2.69666892239163,59.875276643214));
#13423=CARTESIAN_POINT('Ctrl Pts',(4.25838236286678,1.5641254030092,60.0715745125529));
#13424=CARTESIAN_POINT('Ctrl Pts',(2.12344633615567,3.45678232062606,60.2024547543781));
#13425=CARTESIAN_POINT('Ctrl Pts',(0.889652784458242,3.74946171558581,60.2679173686899));
#13426=CARTESIAN_POINT('Ctrl Pts',(2.81263554361569,-2.27688550381632,49.7307924671561));
#13427=CARTESIAN_POINT('Ctrl Pts',(3.56133210250875,-1.3520210126525,49.7962100946696));
#13428=CARTESIAN_POINT('Ctrl Pts',(4.06328662166709,1.27839679708567,49.9270453496967));
#13429=CARTESIAN_POINT('Ctrl Pts',(1.17104134911095,4.09972029296276,50.1232982322374));
#13430=CARTESIAN_POINT('Ctrl Pts',(-2.77159430743786,3.23563350050761,50.3195511147781));
#13431=CARTESIAN_POINT('Ctrl Pts',(-4.22866544159503,-0.525534008911289,
50.5158039973186));
#13432=CARTESIAN_POINT('Ctrl Pts',(-1.8938524922779,-3.81764116429163,50.7120568798594));
#13433=CARTESIAN_POINT('Ctrl Pts',(2.13928848764612,-3.68524262189247,50.9083097623999));
#13434=CARTESIAN_POINT('Ctrl Pts',(4.25403548778285,-0.248720136858517,
51.1045626449406));
#13435=CARTESIAN_POINT('Ctrl Pts',(2.55406324754943,3.41111464661623,51.3008155274813));
#13436=CARTESIAN_POINT('Ctrl Pts',(-1.43622651411465,4.01195357487067,51.4970684100218));
#13437=CARTESIAN_POINT('Ctrl Pts',(-4.13860228786703,1.01521313918572,51.6933212925626));
#13438=CARTESIAN_POINT('Ctrl Pts',(-3.12976073044053,-2.89193666904667,
51.8895741751032));
#13439=CARTESIAN_POINT('Ctrl Pts',(0.685639547014467,-4.20577563258779,
52.0858270576438));
#13440=CARTESIAN_POINT('Ctrl Pts',(3.88620421837496,-1.74816794005548,52.2820799401845));
#13441=CARTESIAN_POINT('Ctrl Pts',(3.60188373594449,2.27708301682602,52.4783328227251));
#13442=CARTESIAN_POINT('Ctrl Pts',(0.087637203604645,4.26039759360026,52.6745857052657));
#13443=CARTESIAN_POINT('Ctrl Pts',(-3.50519640220714,2.42327658685007,52.8708385878064));
#13444=CARTESIAN_POINT('Ctrl Pts',(-3.95480674811289,-1.58687567121949,
53.067091470347));
#13445=CARTESIAN_POINT('Ctrl Pts',(-0.858013619596578,-4.17402477774934,
53.2633443528877));
#13446=CARTESIAN_POINT('Ctrl Pts',(3.00818814011577,-3.01819064426531,53.4595972354283));
#13447=CARTESIAN_POINT('Ctrl Pts',(4.17685004463815,0.844152986655114,53.655850117969));
#13448=CARTESIAN_POINT('Ctrl Pts',(1.59999506082199,3.94951722453104,53.8521030005096));
#13449=CARTESIAN_POINT('Ctrl Pts',(-2.4116273797703,3.51322130502469,54.0483558830502));
#13450=CARTESIAN_POINT('Ctrl Pts',(-4.2606653422332,-0.0734940982690915,
54.2446087655909));
#13451=CARTESIAN_POINT('Ctrl Pts',(-2.2890265223161,-3.59430495589765,54.4408616481315));
#13452=CARTESIAN_POINT('Ctrl Pts',(1.73525661133193,-3.89198600149939,54.6371145306722));
#13453=CARTESIAN_POINT('Ctrl Pts',(4.20347886863225,-0.699596984491061,
54.8333674132129));
#13454=CARTESIAN_POINT('Ctrl Pts',(2.90230530926582,3.12014333509764,55.0296202957534));
#13455=CARTESIAN_POINT('Ctrl Pts',(-1.00145954060489,4.14194994315114,55.2258731782941));
#13456=CARTESIAN_POINT('Ctrl Pts',(-4.00718314321467,1.44953571621855,55.4221260608347));
#13457=CARTESIAN_POINT('Ctrl Pts',(-3.41953567310348,-2.54272419293957,
55.6183789433754));
#13458=CARTESIAN_POINT('Ctrl Pts',(0.234520330591796,-4.25484086323758,
55.8146318259161));
#13459=CARTESIAN_POINT('Ctrl Pts',(3.67827434291722,-2.15150374384035,56.0108847084567));
#13460=CARTESIAN_POINT('Ctrl Pts',(3.82360047981264,1.88115654081442,56.2071375909973));
#13461=CARTESIAN_POINT('Ctrl Pts',(0.540180047856109,4.22692277754893,56.403390473538));
#13462=CARTESIAN_POINT('Ctrl Pts',(-3.22763730584292,2.78227023105407,56.5996433560786));
#13463=CARTESIAN_POINT('Ctrl Pts',(-4.10112770713532,-1.15733415252229,
56.7958962386193));
#13464=CARTESIAN_POINT('Ctrl Pts',(-1.29700371899468,-4.05911968132693,
56.9921491211599));
#13465=CARTESIAN_POINT('Ctrl Pts',(2.67018520888184,-3.32096053654349,57.1884020037006));
#13466=CARTESIAN_POINT('Ctrl Pts',(4.24293317826126,0.395210776154675,57.3846548862412));
#13467=CARTESIAN_POINT('Ctrl Pts',(2.01090395449088,3.75698544838359,57.5809077687819));
#13468=CARTESIAN_POINT('Ctrl Pts',(-2.02436522829424,3.74974608241314,57.7771606513224));
#13469=CARTESIAN_POINT('Ctrl Pts',(-4.24432610842296,0.379994490675165,
57.9734135338631));
#13470=CARTESIAN_POINT('Ctrl Pts',(-2.65825085865726,-3.33052383080523,
58.1696664164038));
#13471=CARTESIAN_POINT('Ctrl Pts',(1.31154165091137,-4.0544267886704,58.3659192989444));
#13472=CARTESIAN_POINT('Ctrl Pts',(4.10527711611601,-1.14264692916782,58.562172181485));
#13473=CARTESIAN_POINT('Ctrl Pts',(3.21758787539612,2.79388759650396,58.7584250640257));
#13474=CARTESIAN_POINT('Ctrl Pts',(-0.555237960034345,4.2248407334863,58.9546779465664));
#13475=CARTESIAN_POINT('Ctrl Pts',(-3.83052076119216,1.86766485748302,59.1509308291069));
#13476=CARTESIAN_POINT('Ctrl Pts',(-3.67013912963673,-2.16515038289994,
59.3471837116477));
#13477=CARTESIAN_POINT('Ctrl Pts',(-0.220046676040735,-4.25471956948896,
59.5434365941882));
#13478=CARTESIAN_POINT('Ctrl Pts',(3.43021234163902,-2.53232849629068,59.739689476729));
#13479=CARTESIAN_POINT('Ctrl Pts',(3.99886797969449,1.46880445609153,59.9359873460677));
#13480=CARTESIAN_POINT('Ctrl Pts',(1.99403924699144,3.2461190557392,60.066867587893));
#13481=CARTESIAN_POINT('Ctrl Pts',(0.835435555021673,3.5209619799037,60.1323302022048));
#13482=CARTESIAN_POINT('Ctrl Pts',(2.63010404172658,-2.12912255188162,49.595205300671));
#13483=CARTESIAN_POINT('Ctrl Pts',(3.33021246851552,-1.26427895642155,49.6606229281846));
#13484=CARTESIAN_POINT('Ctrl Pts',(3.79959166433701,1.19543272877191,49.7914581832116));
#13485=CARTESIAN_POINT('Ctrl Pts',(1.0950443232209,3.83366090105244,49.9877110657523));
#13486=CARTESIAN_POINT('Ctrl Pts',(-2.59172625709189,3.02565071629977,50.1839639482929));
#13487=CARTESIAN_POINT('Ctrl Pts',(-3.95423790127865,-0.491428448324842,
50.3802168308336));
#13488=CARTESIAN_POINT('Ctrl Pts',(-1.77094721912348,-3.56988785086517,
50.5764697133742));
#13489=CARTESIAN_POINT('Ctrl Pts',(2.00045516403601,-3.446081571636,50.7727225959148));
#13490=CARTESIAN_POINT('Ctrl Pts',(3.97796150854402,-0.23257895559744,50.9689754784555));
#13491=CARTESIAN_POINT('Ctrl Pts',(2.38831230212276,3.18974366914418,51.1652283609961));
#13492=CARTESIAN_POINT('Ctrl Pts',(-1.34301977665826,3.75158997632597,51.3614812435369));
#13493=CARTESIAN_POINT('Ctrl Pts',(-3.87001957261238,0.949328890707901,
51.5577341260774));
#13494=CARTESIAN_POINT('Ctrl Pts',(-2.92664876736462,-2.70425876503685,
51.7539870086181));
#13495=CARTESIAN_POINT('Ctrl Pts',(0.641143623411707,-3.93283357133589,
51.9502398911587));
#13496=CARTESIAN_POINT('Ctrl Pts',(3.6340013710356,-1.6347171517452,52.1464927736993));
#13497=CARTESIAN_POINT('Ctrl Pts',(3.36813242413865,2.12930724689704,52.34274565624));
#13498=CARTESIAN_POINT('Ctrl Pts',(0.0819498153357979,3.9839107330222,52.5389985387806));
#13499=CARTESIAN_POINT('Ctrl Pts',(-3.27771980462114,2.26601329836803,52.7352514213213));
#13500=CARTESIAN_POINT('Ctrl Pts',(-3.69815180501057,-1.48389226114473,
52.9315043038619));
#13501=CARTESIAN_POINT('Ctrl Pts',(-0.802331142362098,-3.90314325051617,
53.1277571864026));
#13502=CARTESIAN_POINT('Ctrl Pts',(2.81296586880989,-2.82231924082809,53.3240100689432));
#13503=CARTESIAN_POINT('Ctrl Pts',(3.90578516616716,0.789370022389415,53.5202629514839));
#13504=CARTESIAN_POINT('Ctrl Pts',(1.49616024221923,3.69320555543942,53.7165158340245));
#13505=CARTESIAN_POINT('Ctrl Pts',(-2.25512008943702,3.28522391562577,53.9127687165651));
#13506=CARTESIAN_POINT('Ctrl Pts',(-3.98416110558228,-0.0687245545692351,
54.1090215991058));
#13507=CARTESIAN_POINT('Ctrl Pts',(-2.14047565516563,-3.36104548389223,
54.3052744816464));
#13508=CARTESIAN_POINT('Ctrl Pts',(1.62264372903072,-3.63940793400053,54.5015273641871));
#13509=CARTESIAN_POINT('Ctrl Pts',(3.93068586038341,-0.65419526559929,54.6977802467277));
#13510=CARTESIAN_POINT('Ctrl Pts',(2.71395451200611,2.91765551176149,54.8940331292684));
#13511=CARTESIAN_POINT('Ctrl Pts',(-0.936467858891026,3.87314997523886,
55.090286011809));
#13512=CARTESIAN_POINT('Ctrl Pts',(-3.7471291311917,1.35546525197946,55.2865388943497));
#13513=CARTESIAN_POINT('Ctrl Pts',(-3.19761819659582,-2.37770911770861,
55.4827917768903));
#13514=CARTESIAN_POINT('Ctrl Pts',(0.219300673617886,-3.9787146175785,55.6790446594309));
#13515=CARTESIAN_POINT('Ctrl Pts',(3.43956551279636,-2.01187768721363,55.8752975419716));
#13516=CARTESIAN_POINT('Ctrl Pts',(3.5754604249135,1.75907519633921,56.0715504245122));
#13517=CARTESIAN_POINT('Ctrl Pts',(0.505124003837354,3.95260833083485,56.2678033070529));
#13518=CARTESIAN_POINT('Ctrl Pts',(-3.01817345037608,2.60170934569926,56.4640561895935));
#13519=CARTESIAN_POINT('Ctrl Pts',(-3.83497697832098,-1.08222668204786,
56.6603090721341));
#13520=CARTESIAN_POINT('Ctrl Pts',(-1.21283211797753,-3.7956951457656,56.8565619546748));
#13521=CARTESIAN_POINT('Ctrl Pts',(2.49689830094754,-3.10544028692363,57.0528148372155));
#13522=CARTESIAN_POINT('Ctrl Pts',(3.96757970518115,0.369562797447294,57.2490677197561));
#13523=CARTESIAN_POINT('Ctrl Pts',(1.88040239704553,3.51316850664524,57.4453206022968));
#13524=CARTESIAN_POINT('Ctrl Pts',(-1.89299007507492,3.5063989535328,57.6415734848374));
#13525=CARTESIAN_POINT('Ctrl Pts',(-3.96888223840713,0.355334002667765,
57.837826367378));
#13526=CARTESIAN_POINT('Ctrl Pts',(-2.48573845379553,-3.11438295244143,
58.0340792499187));
#13527=CARTESIAN_POINT('Ctrl Pts',(1.22642658227961,-3.79130680758531,58.2303321324593));
#13528=CARTESIAN_POINT('Ctrl Pts',(3.83885710326488,-1.06849261486876,58.4265850149999));
#13529=CARTESIAN_POINT('Ctrl Pts',(3.00877619743473,2.61257277942545,58.6228378975406));
#13530=CARTESIAN_POINT('Ctrl Pts',(-0.519204703261722,3.95066140510655,
58.8190907800813));
#13531=CARTESIAN_POINT('Ctrl Pts',(-3.58193160105556,1.74645908226778,59.0153436626219));
#13532=CARTESIAN_POINT('Ctrl Pts',(-3.4319582501427,-2.02463870085725,59.2115965451625));
#13533=CARTESIAN_POINT('Ctrl Pts',(-0.205766315275689,-3.97860119542568,
59.4078494277032));
#13534=CARTESIAN_POINT('Ctrl Pts',(3.20760198177951,-2.36798807018971,59.6041023102438));
#13535=CARTESIAN_POINT('Ctrl Pts',(3.73935359652219,1.37348350917383,59.8004001795827));
#13536=CARTESIAN_POINT('Ctrl Pts',(1.8646321578272,3.03545579085233,59.931280421408));
#13537=CARTESIAN_POINT('Ctrl Pts',(0.781218325585102,3.29246224422161,59.9967430357197));
#13538=CARTESIAN_POINT('Ctrl Pts',(0.784811935329597,3.29764693208115,60.));
#13539=CARTESIAN_POINT('Ctrl Pts',(0.889235603863764,3.28374633008718,60.));
#13540=CARTESIAN_POINT('Ctrl Pts',(0.992623261153783,3.26463846910174,60.));
#13541=CARTESIAN_POINT('Ctrl Pts',(1.09473595312137,3.24065669353082,60.));
#13542=CARTESIAN_POINT('Ctrl Pts',(1.20064317507693,3.2157837499296,60.));
#13543=CARTESIAN_POINT('Ctrl Pts',(1.3051794749988,3.18566793874592,60.));
#13544=CARTESIAN_POINT('Ctrl Pts',(1.40808566984841,3.15062538127982,60.));
#13545=CARTESIAN_POINT('Ctrl Pts',(1.51283637750168,3.11495471346514,60.));
#13546=CARTESIAN_POINT('Ctrl Pts',(1.61589871569635,3.07417889385732,60.));
#13547=CARTESIAN_POINT('Ctrl Pts',(1.71699714510354,3.02857636387343,60.));
#13548=CARTESIAN_POINT('Ctrl Pts',(1.78322715166281,2.99870195457091,60.));
#13549=CARTESIAN_POINT('Ctrl Pts',(1.84861426059305,2.9667549850191,60.));
#13550=CARTESIAN_POINT('Ctrl Pts',(1.91307826822121,2.93280201322383,60.));
#13551=CARTESIAN_POINT('Ctrl Pts',(1.94433236805735,2.91634058599851,60.));
#13552=CARTESIAN_POINT('Ctrl Pts',(1.97536889450896,2.89940780269719,60.));
#13553=CARTESIAN_POINT('Ctrl Pts',(2.00618011160133,2.88200955967882,60.));
#13554=CARTESIAN_POINT('Ctrl Pts',(2.03056702399939,2.86823894402617,60.));
#13555=CARTESIAN_POINT('Ctrl Pts',(2.05481756915562,2.85417358949421,60.));
#13556=CARTESIAN_POINT('Ctrl Pts',(2.07888625271118,2.83984169026282,60.));
#13557=CARTESIAN_POINT('Ctrl Pts',(2.17718404178886,2.78130944837773,60.));
#13558=CARTESIAN_POINT('Ctrl Pts',(2.2725670919976,2.71827226665768,60.));
#13559=CARTESIAN_POINT('Ctrl Pts',(2.36475625773662,2.65106472009617,60.));
#13560=CARTESIAN_POINT('Ctrl Pts',(2.45801085040187,2.58308045829727,60.));
#13561=CARTESIAN_POINT('Ctrl Pts',(2.54799808861466,2.51082853560115,60.));
#13562=CARTESIAN_POINT('Ctrl Pts',(2.63441837229004,2.43460216440961,60.));
#13563=CARTESIAN_POINT('Ctrl Pts',(2.72073546283663,2.35846681395307,60.));
#13564=CARTESIAN_POINT('Ctrl Pts',(2.80349489384814,2.27836603613578,60.));
#13565=CARTESIAN_POINT('Ctrl Pts',(2.88237584537992,2.19454559636136,60.));
#13566=CARTESIAN_POINT('Ctrl Pts',(2.95189189665301,2.12067648251395,60.));
#13567=CARTESIAN_POINT('Ctrl Pts',(3.01839575888545,2.04391761646293,60.));
#13568=CARTESIAN_POINT('Ctrl Pts',(3.08164607665535,1.96441162407651,60.));
#13569=CARTESIAN_POINT('Ctrl Pts',(3.09160214974873,1.95189678621529,60.));
#13570=CARTESIAN_POINT('Ctrl Pts',(3.10147565654979,1.93931615773848,60.));
#13571=CARTESIAN_POINT('Ctrl Pts',(3.11125942805904,1.92667863680468,60.));
#13572=CARTESIAN_POINT('Ctrl Pts',(3.18384639438312,1.83291936354545,60.));
#13573=CARTESIAN_POINT('Ctrl Pts',(3.25159841668943,1.73590401314964,60.));
#13574=CARTESIAN_POINT('Ctrl Pts',(3.31421073674484,1.63593934473944,60.));
#13575=CARTESIAN_POINT('Ctrl Pts',(3.37660547873583,1.53632205395468,60.));
#13576=CARTESIAN_POINT('Ctrl Pts',(3.43389695780907,1.4337753814893,60.));
#13577=CARTESIAN_POINT('Ctrl Pts',(3.48575479573506,1.32856043853129,60.));
#13578=CARTESIAN_POINT('Ctrl Pts',(3.4931113037334,1.31363473780076,60.));
#13579=CARTESIAN_POINT('Ctrl Pts',(3.50035840622805,1.2986552783797,60.));
#13580=CARTESIAN_POINT('Ctrl Pts',(3.50749509871695,1.28362274566985,60.));
#13581=CARTESIAN_POINT('Ctrl Pts',(3.55683940162616,1.17968526361056,60.));
#13582=CARTESIAN_POINT('Ctrl Pts',(3.60090919697516,1.07321295524336,60.));
#13583=CARTESIAN_POINT('Ctrl Pts',(3.63979310801694,0.964595844985372,60.));
#13584=CARTESIAN_POINT('Ctrl Pts',(3.66420924373342,0.896392569282407,60.));
#13585=CARTESIAN_POINT('Ctrl Pts',(3.68657974486052,0.827342990746825,60.));
#13586=CARTESIAN_POINT('Ctrl Pts',(3.7069172792925,0.757538875098194,60.));
#13587=CARTESIAN_POINT('Ctrl Pts',(3.71289219481231,0.737031291185787,60.));
#13588=CARTESIAN_POINT('Ctrl Pts',(3.71869159509938,0.716458563232633,60.));
#13589=CARTESIAN_POINT('Ctrl Pts',(3.72431568230938,0.695822974884761,60.));
#13590=CARTESIAN_POINT('Ctrl Pts',(3.72862390834875,0.680015471242239,60.));
#13591=CARTESIAN_POINT('Ctrl Pts',(3.73282894190367,0.664172025657236,60.));
#13592=CARTESIAN_POINT('Ctrl Pts',(3.73692780152788,0.648306312974997,60.));
#13593=CARTESIAN_POINT('Ctrl Pts',(3.76710608338592,0.531493347150171,60.));
#13594=CARTESIAN_POINT('Ctrl Pts',(3.79158238148832,0.41329696895828,60.));
#13595=CARTESIAN_POINT('Ctrl Pts',(3.8105094559077,0.294179008852515,60.));
#13596=CARTESIAN_POINT('Ctrl Pts',(3.82934522625211,0.175635672955355,60.));
#13597=CARTESIAN_POINT('Ctrl Pts',(3.84268518208166,0.0561787816862602,
60.));
#13598=CARTESIAN_POINT('Ctrl Pts',(3.85063242918259,-0.063766621316311,
60.));
#13599=CARTESIAN_POINT('Ctrl Pts',(3.858704791944,-0.18560035723804,60.));
#13600=CARTESIAN_POINT('Ctrl Pts',(3.86121348940923,-0.30793892891327,60.));
#13601=CARTESIAN_POINT('Ctrl Pts',(3.85821592230841,-0.43035561873873,60.));
#13602=CARTESIAN_POINT('Ctrl Pts',(3.85526835997703,-0.550730179682494,
60.));
#13603=CARTESIAN_POINT('Ctrl Pts',(3.84699662600882,-0.671181149539089,
60.));
#13604=CARTESIAN_POINT('Ctrl Pts',(3.83340642503076,-0.791307982107533,
60.));
#13605=CARTESIAN_POINT('Ctrl Pts',(3.83135847340105,-0.809410285592786,
60.));
#13606=CARTESIAN_POINT('Ctrl Pts',(3.82918993653534,-0.827502340964368,
60.));
#13607=CARTESIAN_POINT('Ctrl Pts',(3.82690230603326,-0.845572403651534,
60.));
#13608=CARTESIAN_POINT('Ctrl Pts',(3.81116757337382,-0.969861533939128,
60.));
#13609=CARTESIAN_POINT('Ctrl Pts',(3.78978713160578,-1.0932500409073,60.));
#13610=CARTESIAN_POINT('Ctrl Pts',(3.76284273210423,-1.21528813763156,60.));
#13611=CARTESIAN_POINT('Ctrl Pts',(3.73586199351469,-1.33749082340648,60.));
#13612=CARTESIAN_POINT('Ctrl Pts',(3.70330231983611,-1.45834038572235,60.));
#13613=CARTESIAN_POINT('Ctrl Pts',(3.665194221274,-1.57738923136754,60.));
#13614=CARTESIAN_POINT('Ctrl Pts',(3.65552125866432,-1.60760734972301,60.));
#13615=CARTESIAN_POINT('Ctrl Pts',(3.64549055351521,-1.6377094291362,60.));
#13616=CARTESIAN_POINT('Ctrl Pts',(3.6351020718132,-1.66768807850306,60.));
#13617=CARTESIAN_POINT('Ctrl Pts',(3.62847368432654,-1.68681600402967,60.));
#13618=CARTESIAN_POINT('Ctrl Pts',(3.62169927309294,-1.70589468101949,60.));
#13619=CARTESIAN_POINT('Ctrl Pts',(3.61477991705996,-1.72491906517069,60.));
#13620=CARTESIAN_POINT('Ctrl Pts',(3.57054791692283,-1.84653248676284,60.));
#13621=CARTESIAN_POINT('Ctrl Pts',(3.52049512035426,-1.96566066503241,60.));
#13622=CARTESIAN_POINT('Ctrl Pts',(3.46468375047193,-2.0818202580808,60.));
#13623=CARTESIAN_POINT('Ctrl Pts',(3.4088723805896,-2.19797985112919,60.));
#13624=CARTESIAN_POINT('Ctrl Pts',(3.34730245526163,-2.31117192238551,60.));
#13625=CARTESIAN_POINT('Ctrl Pts',(3.27997999600525,-2.42090362774469,60.));
#13626=CARTESIAN_POINT('Ctrl Pts',(3.24835722849275,-2.47244690536188,60.));
#13627=CARTESIAN_POINT('Ctrl Pts',(3.21546442815301,-2.52322646076057,60.));
#13628=CARTESIAN_POINT('Ctrl Pts',(3.18134623828594,-2.57322545645539,59.9999999999999));
#13629=CARTESIAN_POINT('Origin',(0.,0.,60.));
#13630=CARTESIAN_POINT('',(8.,9.79717439317883E-16,58.5));
#13631=CARTESIAN_POINT('Origin',(0.,0.,58.5));
#13632=CARTESIAN_POINT('',(8.,9.79717439317883E-16,60.));
#13633=CARTESIAN_POINT('',(8.,-9.79717439317883E-16,60.));
#13634=CARTESIAN_POINT('Origin',(0.,0.,60.));
#13635=CARTESIAN_POINT('Origin',(0.,0.,58.5));
#13636=CARTESIAN_POINT('',(-5.,-6.12323399573677E-16,58.5));
#13637=CARTESIAN_POINT('Origin',(0.,0.,58.5));
#13638=CARTESIAN_POINT('Origin',(0.,0.,28.));
#13639=CARTESIAN_POINT('',(-5.,-6.12323399573677E-16,28.));
#13640=CARTESIAN_POINT('Origin',(0.,0.,28.));
#13641=CARTESIAN_POINT('Origin',(0.,0.,0.));
#13642=CARTESIAN_POINT('',(-5.,-6.12323399573677E-16,0.));
#13643=CARTESIAN_POINT('Origin',(0.,0.,60.));
#13644=CARTESIAN_POINT('',(0.,0.,0.));
#13645=CARTESIAN_POINT('Origin',(0.,0.,-41.3107734492731));
#13646=CARTESIAN_POINT('',(2.26878001451759,-2.28883263001592,-38.0956657793148));
#13647=CARTESIAN_POINT('',(2.26878020134171,-2.28883244482855,-38.344825298285));
#13648=CARTESIAN_POINT('',(2.26878020078428,-2.2888324453811,-41.3107734492731));
#13649=CARTESIAN_POINT('',(1.84084363913124,2.64526222873462,-39.));
#13650=CARTESIAN_POINT('Ctrl Pts',(2.26878001451759,-2.28883263001592,-38.0956657793148));
#13651=CARTESIAN_POINT('Ctrl Pts',(2.17427930154028,-2.38250541593696,-38.1031821119126));
#13652=CARTESIAN_POINT('Ctrl Pts',(2.07398878675681,-2.47031457822959,-38.1107887399296));
#13653=CARTESIAN_POINT('Ctrl Pts',(1.91972359255967,-2.58931774641987,-38.122253635876));
#13654=CARTESIAN_POINT('Ctrl Pts',(1.869930754377,-2.62550248948013,-38.1259203852923));
#13655=CARTESIAN_POINT('Ctrl Pts',(1.78247137899517,-2.68530931588415,-38.1323246749032));
#13656=CARTESIAN_POINT('Ctrl Pts',(1.74529506510832,-2.70961900969796,-38.1350361091484));
#13657=CARTESIAN_POINT('Ctrl Pts',(1.66652723587141,-2.75883189158207,-38.1407651395205));
#13658=CARTESIAN_POINT('Ctrl Pts',(1.62485268027866,-2.78358039315739,-38.1437873718118));
#13659=CARTESIAN_POINT('Ctrl Pts',(1.50737368546323,-2.84980824849279,-38.152289114961));
#13660=CARTESIAN_POINT('Ctrl Pts',(1.43043989539902,-2.88919055487944,-38.1578375993854));
#13661=CARTESIAN_POINT('Ctrl Pts',(1.24367634917405,-2.97550547877898,-38.1712616004222));
#13662=CARTESIAN_POINT('Ctrl Pts',(1.13264029483711,-3.01951748271545,-38.1792092104411));
#13663=CARTESIAN_POINT('Ctrl Pts',(0.821702195093543,-3.12319787988501,
-38.2012225741584));
#13664=CARTESIAN_POINT('Ctrl Pts',(0.618038901880371,-3.16979441051984,
-38.2154007525052));
#13665=CARTESIAN_POINT('Ctrl Pts',(0.373706171312501,-3.20123374711232,
-38.2312996909552));
#13666=CARTESIAN_POINT('Ctrl Pts',(0.336033961644013,-3.20540719232247,
-38.2337192936363));
#13667=CARTESIAN_POINT('Ctrl Pts',(0.273065766336089,-3.21126060431635,
-38.2377013562446));
#13668=CARTESIAN_POINT('Ctrl Pts',(0.247808888654028,-3.21330834128441,
-38.2392816759083));
#13669=CARTESIAN_POINT('Ctrl Pts',(0.192163688630469,-3.21715978698585,
-38.2427243257972));
#13670=CARTESIAN_POINT('Ctrl Pts',(0.161769713007847,-3.21883126234038,
-38.2445800156828));
#13671=CARTESIAN_POINT('Ctrl Pts',(0.0639424290906524,-3.2228218988923,
-38.2504862289476));
#13672=CARTESIAN_POINT('Ctrl Pts',(-0.00354499632442759,-3.22345440752924,
-38.2544591921075));
#13673=CARTESIAN_POINT('Ctrl Pts',(-0.180335593062599,-3.21955823055032,
-38.2647129799248));
#13674=CARTESIAN_POINT('Ctrl Pts',(-0.289476570193864,-3.21158557147246,
-38.27089041191));
#13675=CARTESIAN_POINT('Ctrl Pts',(-0.610562095813819,-3.17162599647257,
-38.2891052733638));
#13676=CARTESIAN_POINT('Ctrl Pts',(-0.819933794119309,-3.12405146962742,
-38.3010735787721));
#13677=CARTESIAN_POINT('Ctrl Pts',(-1.08212018107994,-3.03628326866418,
-38.3173351951035));
#13678=CARTESIAN_POINT('Ctrl Pts',(-1.14061879793893,-3.01479488427622,
-38.3210459815119));
#13679=CARTESIAN_POINT('Ctrl Pts',(-1.23984078362437,-2.97504622312177,
-38.3275046740137));
#13680=CARTESIAN_POINT('Ctrl Pts',(-1.28087621313628,-2.9576106954346,-38.3302254250328));
#13681=CARTESIAN_POINT('Ctrl Pts',(-1.36560691285732,-2.91951541461419,
-38.3359541594752));
#13682=CARTESIAN_POINT('Ctrl Pts',(-1.40922533877395,-2.898712826262,-38.3389663623536));
#13683=CARTESIAN_POINT('Ctrl Pts',(-1.52838881523734,-2.83855581542678,
-38.3473783120707));
#13684=CARTESIAN_POINT('Ctrl Pts',(-1.60286243813911,-2.79717740831116,
-38.3528443328577));
#13685=CARTESIAN_POINT('Ctrl Pts',(-1.77510703048615,-2.69233749314807,
-38.3659908953008));
#13686=CARTESIAN_POINT('Ctrl Pts',(-1.87124496435387,-2.62642813890307,
-38.3737389737698));
#13687=CARTESIAN_POINT('Ctrl Pts',(-2.13061290652,-2.42713193467413,-38.3956945626229));
#13688=CARTESIAN_POINT('Ctrl Pts',(-2.2846508285143,-2.28273074097921,-38.4100357637933));
#13689=CARTESIAN_POINT('Ctrl Pts',(-2.44953378773206,-2.0946268219425,-38.4262100603979));
#13690=CARTESIAN_POINT('Ctrl Pts',(-2.47501979126649,-2.06445020581086,
-38.4287358608301));
#13691=CARTESIAN_POINT('Ctrl Pts',(-2.51586899692722,-2.01423866107835,
-38.4328169626678));
#13692=CARTESIAN_POINT('Ctrl Pts',(-2.53156252201413,-1.99447876822622,
-38.4343930553287));
#13693=CARTESIAN_POINT('Ctrl Pts',(-2.56488148344358,-1.95149944427592,
-38.4377543381736));
#13694=CARTESIAN_POINT('Ctrl Pts',(-2.58242682080637,-1.92822170973902,
-38.4395344840916));
#13695=CARTESIAN_POINT('Ctrl Pts',(-2.63534880786377,-1.85599075527485,
-38.4449464787116));
#13696=CARTESIAN_POINT('Ctrl Pts',(-2.66966885102523,-1.80627633665412,
-38.4485167828663));
#13697=CARTESIAN_POINT('Ctrl Pts',(-2.75236188219421,-1.67898026072075,
-38.457355493476));
#13698=CARTESIAN_POINT('Ctrl Pts',(-2.79887016946234,-1.60024941733983,
-38.4625516254117));
#13699=CARTESIAN_POINT('Ctrl Pts',(-2.96357549248282,-1.29222487473665,
-38.482258049921));
#13700=CARTESIAN_POINT('Ctrl Pts',(-3.05743459791969,-1.05105193063969,
-38.4965057754337));
#13701=CARTESIAN_POINT('Ctrl Pts',(-3.13556507642905,-0.74667707418331,
-38.5150730985969));
#13702=CARTESIAN_POINT('Ctrl Pts',(-3.14814455250686,-0.691722713896159,
-38.5184431351841));
#13703=CARTESIAN_POINT('Ctrl Pts',(-3.16790661457513,-0.593628696447907,
-38.5245056101752));
#13704=CARTESIAN_POINT('Ctrl Pts',(-3.17566463409302,-0.550618918493252,
-38.52717947519));
#13705=CARTESIAN_POINT('Ctrl Pts',(-3.19040727652036,-0.458161281488515,
-38.5329670697561));
#13706=CARTESIAN_POINT('Ctrl Pts',(-3.19712190130789,-0.408682593610614,
-38.536088398376));
#13707=CARTESIAN_POINT('Ctrl Pts',(-3.21348182352234,-0.262762107780036,
-38.5453712122579));
#13708=CARTESIAN_POINT('Ctrl Pts',(-3.21992891269857,-0.166024689612769,
-38.5516259899797));
#13709=CARTESIAN_POINT('Ctrl Pts',(-3.22513213349805,0.0764132141607757,
-38.5675420461662));
#13710=CARTESIAN_POINT('Ctrl Pts',(-3.21838798756779,0.222012007419459,
-38.577323546392));
#13711=CARTESIAN_POINT('Ctrl Pts',(-3.18400643390368,0.52225814946355,-38.5976867794836));
#13712=CARTESIAN_POINT('Ctrl Pts',(-3.15486494240396,0.676375973455781,
-38.6082464805641));
#13713=CARTESIAN_POINT('Ctrl Pts',(-3.10379610272837,0.868530916512614,
-38.6211444334022));
#13714=CARTESIAN_POINT('Ctrl Pts',(-3.09216399532717,0.909075578314394,
-38.6238495537467));
#13715=CARTESIAN_POINT('Ctrl Pts',(-3.07286290510045,0.971687147383015,
-38.6279894493481));
#13716=CARTESIAN_POINT('Ctrl Pts',(-3.06574461517715,0.993917707105095,
-38.6294518780201));
#13717=CARTESIAN_POINT('Ctrl Pts',(-3.04974423717555,1.04207906636557,-38.6326010065231));
#13718=CARTESIAN_POINT('Ctrl Pts',(-3.04077165134808,1.06797779819059,-38.6342825222027));
#13719=CARTESIAN_POINT('Ctrl Pts',(-3.01455442083262,1.14064157875144,-38.6389747727755));
#13720=CARTESIAN_POINT('Ctrl Pts',(-2.99655318293537,1.18712727360001,-38.6419464813996));
#13721=CARTESIAN_POINT('Ctrl Pts',(-2.9010718496155,1.41766451215537,-38.6566189025427));
#13722=CARTESIAN_POINT('Ctrl Pts',(-2.80767645097417,1.59466540573218,-38.6676942323365));
#13723=CARTESIAN_POINT('Ctrl Pts',(-2.61471693746718,1.89019917412492,-38.6875721856302));
#13724=CARTESIAN_POINT('Ctrl Pts',(-2.52190748015245,2.01235543870383,-38.6962748297064));
#13725=CARTESIAN_POINT('Ctrl Pts',(-2.37926698100997,2.17466280210837,-38.708978581507));
#13726=CARTESIAN_POINT('Ctrl Pts',(-2.33639660435145,2.22065751993029,-38.7127213559991));
#13727=CARTESIAN_POINT('Ctrl Pts',(-2.26075171756163,2.29719876128185,-38.7192227871496));
#13728=CARTESIAN_POINT('Ctrl Pts',(-2.22863445874217,2.32837037958883,-38.7219535599213));
#13729=CARTESIAN_POINT('Ctrl Pts',(-2.16052169967961,2.39177698215744,-38.7276911734426));
#13730=CARTESIAN_POINT('Ctrl Pts',(-2.12442968793483,2.42389134615721,-38.7307019823683));
#13731=CARTESIAN_POINT('Ctrl Pts',(-2.02315964388885,2.51000087189528,-38.7390769872662));
#13732=CARTESIAN_POINT('Ctrl Pts',(-1.95655899876813,2.56225568923481,-38.7445059190418));
#13733=CARTESIAN_POINT('Ctrl Pts',(-1.79446994891085,2.679423335291,-38.757537810221));
#13734=CARTESIAN_POINT('Ctrl Pts',(-1.69739993545653,2.74194488012524,-38.765206115763));
#13735=CARTESIAN_POINT('Ctrl Pts',(-1.41578970221266,2.90263306073517,-38.7869492357482));
#13736=CARTESIAN_POINT('Ctrl Pts',(-1.22474714851479,2.98826727907264,-38.80115617944));
#13737=CARTESIAN_POINT('Ctrl Pts',(-0.988108431002874,3.06780403406154,
-38.8173102259719));
#13738=CARTESIAN_POINT('Ctrl Pts',(-0.949216612935885,3.0800597444351,-38.8199193969883));
#13739=CARTESIAN_POINT('Ctrl Pts',(-0.885417164203674,3.09884108781853,
-38.8241141588516));
#13740=CARTESIAN_POINT('Ctrl Pts',(-0.860646447621111,3.10581189149313,
-38.82572186273));
#13741=CARTESIAN_POINT('Ctrl Pts',(-0.80685420215233,3.12025666910299,-38.8291655931871));
#13742=CARTESIAN_POINT('Ctrl Pts',(-0.77780753709691,3.12762385346042,-38.8309962483499));
#13743=CARTESIAN_POINT('Ctrl Pts',(-0.687972593484296,3.14907994088346,
-38.8365810976268));
#13744=CARTESIAN_POINT('Ctrl Pts',(-0.626871872190585,3.1618101498719,-38.8402717951017));
#13745=CARTESIAN_POINT('Ctrl Pts',(-0.470797425980772,3.18962510812534,
-38.8495130003313));
#13746=CARTESIAN_POINT('Ctrl Pts',(-0.375446345794052,3.20224927869193,
-38.8549865745452));
#13747=CARTESIAN_POINT('Ctrl Pts',(-0.0462376421054875,3.23092610076355,
-38.8736916624537));
#13748=CARTESIAN_POINT('Ctrl Pts',(0.1886962329817,3.22574130191479,-38.8867647878528));
#13749=CARTESIAN_POINT('Ctrl Pts',(0.479095622825629,3.18747865900904,-38.9040671818742));
#13750=CARTESIAN_POINT('Ctrl Pts',(0.536981939125614,3.17823891517948,-38.9075700890541));
#13751=CARTESIAN_POINT('Ctrl Pts',(0.638510243371634,3.15918026514406,-38.9138276720672));
#13752=CARTESIAN_POINT('Ctrl Pts',(0.682260731435794,3.15002147196495,-38.9165618329659));
#13753=CARTESIAN_POINT('Ctrl Pts',(0.77500019524035,3.12858462174404,-38.9224447898967));
#13754=CARTESIAN_POINT('Ctrl Pts',(0.823919025984935,3.1160590549255,-38.9256005523133));
#13755=CARTESIAN_POINT('Ctrl Pts',(0.965343684771793,3.07628454572699,-38.9348854227035));
#13756=CARTESIAN_POINT('Ctrl Pts',(1.05693958008847,3.04602870622226,-38.9411043850465));
#13757=CARTESIAN_POINT('Ctrl Pts',(1.39244536538294,2.91824874149358,-38.9646496396527));
#13758=CARTESIAN_POINT('Ctrl Pts',(1.62542595403343,2.7951718562419,-38.9826478213699));
#13759=CARTESIAN_POINT('Ctrl Pts',(1.84084363913124,2.64526222873462,-39.));
#13760=CARTESIAN_POINT('',(-1.87158653173895,2.62360084935064,-39.));
#13761=CARTESIAN_POINT('Origin',(0.,0.,-39.));
#13762=CARTESIAN_POINT('Ctrl Pts',(-1.87158653173894,2.62360084935064,-39.));
#13763=CARTESIAN_POINT('Ctrl Pts',(-1.89041153088413,2.61017174298758,-38.998572528826));
#13764=CARTESIAN_POINT('Ctrl Pts',(-1.90909197228119,2.59654004106516,-38.9971558584858));
#13765=CARTESIAN_POINT('Ctrl Pts',(-1.95205518984536,2.56447410407947,-38.9938937119439));
#13766=CARTESIAN_POINT('Ctrl Pts',(-1.97622658142679,2.54589385197734,-38.9920554271223));
#13767=CARTESIAN_POINT('Ctrl Pts',(-2.11761273738408,2.43398489791101,-38.9812640905256));
#13768=CARTESIAN_POINT('Ctrl Pts',(-2.22847532036539,2.33291030558068,-38.972638751804));
#13769=CARTESIAN_POINT('Ctrl Pts',(-2.45378047976953,2.09672449385349,-38.9538741497549));
#13770=CARTESIAN_POINT('Ctrl Pts',(-2.56494030377983,1.9591754907227,-38.943761890126));
#13771=CARTESIAN_POINT('Ctrl Pts',(-2.70202935873906,1.75774238346185,-38.9293276413066));
#13772=CARTESIAN_POINT('Ctrl Pts',(-2.73804212889853,1.70110124467118,-38.9253080656617));
#13773=CARTESIAN_POINT('Ctrl Pts',(-2.7972715271659,1.60118566111969,-38.9182533281895));
#13774=CARTESIAN_POINT('Ctrl Pts',(-2.82131635429567,1.55842779260394,-38.9152452891496));
#13775=CARTESIAN_POINT('Ctrl Pts',(-2.87032957175881,1.46641515134169,-38.9087844952294));
#13776=CARTESIAN_POINT('Ctrl Pts',(-2.89502646778123,1.41703438608332,-38.9053243733345));
#13777=CARTESIAN_POINT('Ctrl Pts',(-2.96365280279685,1.27052724868404,-38.8950659041947));
#13778=CARTESIAN_POINT('Ctrl Pts',(-3.00404362508528,1.17183427025286,-38.888162253539));
#13779=CARTESIAN_POINT('Ctrl Pts',(-3.11469824109349,0.857896153677981,
-38.8662091689328));
#13780=CARTESIAN_POINT('Ctrl Pts',(-3.16723264101671,0.637143388502542,
-38.8507362932036));
#13781=CARTESIAN_POINT('Ctrl Pts',(-3.20635666106965,0.334171303476188,
-38.8301398159638));
#13782=CARTESIAN_POINT('Ctrl Pts',(-3.21360260543384,0.255251114411016,
-38.8248382630747));
#13783=CARTESIAN_POINT('Ctrl Pts',(-3.22097521621672,0.120559799427511,
-38.8159668223204));
#13784=CARTESIAN_POINT('Ctrl Pts',(-3.22257723171047,0.0649060951656778,
-38.8123524644896));
#13785=CARTESIAN_POINT('Ctrl Pts',(-3.22281887525591,-0.0194166743170859,
-38.8069780507899));
#13786=CARTESIAN_POINT('Ctrl Pts',(-3.22251888196611,-0.0480697788259077,
-38.8051696340464));
#13787=CARTESIAN_POINT('Ctrl Pts',(-3.22124484231817,-0.101575361005251,
-38.801830260307));
#13788=CARTESIAN_POINT('Ctrl Pts',(-3.22036528638933,-0.126425308028545,
-38.8002950559868));
#13789=CARTESIAN_POINT('Ctrl Pts',(-3.2173435110204,-0.190734249366148,
-38.7963596350244));
#13790=CARTESIAN_POINT('Ctrl Pts',(-3.21476310027856,-0.230168102610655,
-38.7939823101881));
#13791=CARTESIAN_POINT('Ctrl Pts',(-3.19301600015096,-0.489269564107375,
-38.7785383714708));
#13792=CARTESIAN_POINT('Ctrl Pts',(-3.15207109455574,-0.706545733759861,
-38.7663900090102));
#13793=CARTESIAN_POINT('Ctrl Pts',(-3.05831375244858,-1.02207212315941,
-38.7478935118536));
#13794=CARTESIAN_POINT('Ctrl Pts',(-3.02213455571994,-1.12455109747725,
-38.7417495527388));
#13795=CARTESIAN_POINT('Ctrl Pts',(-2.95020911571181,-1.29957030206577,
-38.7308116176625));
#13796=CARTESIAN_POINT('Ctrl Pts',(-2.91678025577592,-1.37295601985905,
-38.7260825036295));
#13797=CARTESIAN_POINT('Ctrl Pts',(-2.85999748547326,-1.48615305518561,
-38.7185078126796));
#13798=CARTESIAN_POINT('Ctrl Pts',(-2.83847941782484,-1.52684995346584,
-38.7157255651867));
#13799=CARTESIAN_POINT('Ctrl Pts',(-2.79551671447219,-1.60405591198758,
-38.7103247828989));
#13800=CARTESIAN_POINT('Ctrl Pts',(-2.77420970383786,-1.64063076723599,
-38.7077116372666));
#13801=CARTESIAN_POINT('Ctrl Pts',(-2.72180549934165,-1.72664491662706,
-38.7014294811597));
#13802=CARTESIAN_POINT('Ctrl Pts',(-2.6900734781015,-1.77567784329784,-38.6977374421781));
#13803=CARTESIAN_POINT('Ctrl Pts',(-2.49035070894802,-2.06664368980951,
-38.675131534682));
#13804=CARTESIAN_POINT('Ctrl Pts',(-2.29119094673413,-2.2854414502584,-38.6549583088328));
#13805=CARTESIAN_POINT('Ctrl Pts',(-2.00881142332894,-2.52114717574195,
-38.6301828262148));
#13806=CARTESIAN_POINT('Ctrl Pts',(-1.95086142283051,-2.56625160460457,
-38.6252772206526));
#13807=CARTESIAN_POINT('Ctrl Pts',(-1.84932298700513,-2.63985324858534,
-38.6170417746014));
#13808=CARTESIAN_POINT('Ctrl Pts',(-1.80649232547213,-2.66934577441787,
-38.6136711242149));
#13809=CARTESIAN_POINT('Ctrl Pts',(-1.74045357961071,-2.71250106297437,
-38.6086503493814));
#13810=CARTESIAN_POINT('Ctrl Pts',(-1.71775850292413,-2.7269298816449,-38.6069555181186));
#13811=CARTESIAN_POINT('Ctrl Pts',(-1.67301805736663,-2.75459417412688,
-38.6036778302482));
#13812=CARTESIAN_POINT('Ctrl Pts',(-1.65099021493799,-2.76785294000404,
-38.6020931929567));
#13813=CARTESIAN_POINT('Ctrl Pts',(-1.59316223246176,-2.80172409973461,
-38.5980022509281));
#13814=CARTESIAN_POINT('Ctrl Pts',(-1.5571193099854,-2.82191488812873,-38.595520372194));
#13815=CARTESIAN_POINT('Ctrl Pts',(-1.33642960592855,-2.9400260537686,-38.580670697332));
#13816=CARTESIAN_POINT('Ctrl Pts',(-1.14298665592021,-3.02049626713358,
-38.5690793358358));
#13817=CARTESIAN_POINT('Ctrl Pts',(-0.831668191154774,-3.1157702891105,
-38.5507599418689));
#13818=CARTESIAN_POINT('Ctrl Pts',(-0.71847800015837,-3.14380083137577,
-38.5441690601075));
#13819=CARTESIAN_POINT('Ctrl Pts',(-0.520026841832245,-3.18166653884345,
-38.532487348396));
#13820=CARTESIAN_POINT('Ctrl Pts',(-0.435431101271444,-3.19434311466749,
-38.5274698152538));
#13821=CARTESIAN_POINT('Ctrl Pts',(-0.301967547722453,-3.20894226469868,
-38.5194351893927));
#13822=CARTESIAN_POINT('Ctrl Pts',(-0.253387136188485,-3.21314323354393,
-38.5164864377643));
#13823=CARTESIAN_POINT('Ctrl Pts',(-0.159628485629201,-3.21911150423433,
-38.5107399795707));
#13824=CARTESIAN_POINT('Ctrl Pts',(-0.114471451348873,-3.2210333903642,
-38.5079476311848));
#13825=CARTESIAN_POINT('Ctrl Pts',(-0.0157008584167212,-3.22315749462958,
-38.5017809707694));
#13826=CARTESIAN_POINT('Ctrl Pts',(0.0379066963205851,-3.22297274489809,
-38.4983959863226));
#13827=CARTESIAN_POINT('Ctrl Pts',(0.324041235736702,-3.21484713055911,
-38.4801171400821));
#13828=CARTESIAN_POINT('Ctrl Pts',(0.555171700199884,-3.18308015954396,
-38.4645356060155));
#13829=CARTESIAN_POINT('Ctrl Pts',(0.874788367132247,-3.10326305727819,
-38.442442416998));
#13830=CARTESIAN_POINT('Ctrl Pts',(0.96764531124071,-3.07557480588518,-38.4359661394279));
#13831=CARTESIAN_POINT('Ctrl Pts',(1.11831641141395,-3.02314650521573,-38.4254823938246));
#13832=CARTESIAN_POINT('Ctrl Pts',(1.17690569238394,-3.00082328775732,-38.421412607669));
#13833=CARTESIAN_POINT('Ctrl Pts',(1.26252884001002,-2.96530589042621,-38.4155107480571));
#13834=CARTESIAN_POINT('Ctrl Pts',(1.29008681005575,-2.95342077414907,-38.4136184429141));
#13835=CARTESIAN_POINT('Ctrl Pts',(1.34094489582743,-2.93063912210334,-38.4101449343738));
#13836=CARTESIAN_POINT('Ctrl Pts',(1.36428579455454,-2.9198464314739,-38.4085588540844));
#13837=CARTESIAN_POINT('Ctrl Pts',(1.42419223168782,-2.8912708217501,-38.4045046193086));
#13838=CARTESIAN_POINT('Ctrl Pts',(1.46055474404909,-2.87307338068009,-38.4020593485357));
#13839=CARTESIAN_POINT('Ctrl Pts',(1.68165533362765,-2.75714165121245,-38.3872298414131));
#13840=CARTESIAN_POINT('Ctrl Pts',(1.85688661530079,-2.64230687976265,-38.375621741074));
#13841=CARTESIAN_POINT('Ctrl Pts',(2.10657127239634,-2.44149166216285,-38.3575681122106));
#13842=CARTESIAN_POINT('Ctrl Pts',(2.1896836487191,-2.36723604007207,-38.3512617948146));
#13843=CARTESIAN_POINT('Ctrl Pts',(2.26878020134171,-2.28883244482855,-38.344825298285));
#13844=CARTESIAN_POINT('Origin',(0.,0.,-41.3107734492731));
#13845=CARTESIAN_POINT('',(2.26877996761345,-2.28883267650912,-36.8483014782414));
#13846=CARTESIAN_POINT('',(2.26878021215172,-2.28883243411325,-37.0933419659928));
#13847=CARTESIAN_POINT('',(2.26878020078428,-2.2888324453811,-41.3107734492731));
#13848=CARTESIAN_POINT('Ctrl Pts',(2.26877996761344,-2.28883267650913,-36.8483014782414));
#13849=CARTESIAN_POINT('Ctrl Pts',(2.22656546202223,-2.33067733628309,-36.8522391846632));
#13850=CARTESIAN_POINT('Ctrl Pts',(2.18317988826702,-2.37136742025256,-36.8561392081494));
#13851=CARTESIAN_POINT('Ctrl Pts',(2.11075868590298,-2.43561231691168,-36.8623833035587));
#13852=CARTESIAN_POINT('Ctrl Pts',(2.08241891546805,-2.45988644521745,-36.8647640214435));
#13853=CARTESIAN_POINT('Ctrl Pts',(2.03422178204832,-2.49973911779116,-36.8687003436139));
#13854=CARTESIAN_POINT('Ctrl Pts',(2.01459232639169,-2.51558578269246,-36.8702729882877));
#13855=CARTESIAN_POINT('Ctrl Pts',(1.97074503194305,-2.55014074084834,-36.8737172375388));
#13856=CARTESIAN_POINT('Ctrl Pts',(1.94644359286332,-2.56873729265205,-36.8755818053609));
#13857=CARTESIAN_POINT('Ctrl Pts',(1.86656824073359,-2.62807694755233,-36.8815809932148));
#13858=CARTESIAN_POINT('Ctrl Pts',(1.80994891970962,-2.66738667634847,-36.8856340353954));
#13859=CARTESIAN_POINT('Ctrl Pts',(1.65698097380178,-2.76647393784538,-36.8961889940548));
#13860=CARTESIAN_POINT('Ctrl Pts',(1.55866343852762,-2.82303646750421,-36.9025792107261));
#13861=CARTESIAN_POINT('Ctrl Pts',(1.27212214763379,-2.96834219976459,-36.9206475149131));
#13862=CARTESIAN_POINT('Ctrl Pts',(1.07802946847273,-3.04420666120054,-36.9322768815636));
#13863=CARTESIAN_POINT('Ctrl Pts',(0.817433353335214,-3.11799315220279,
-36.9481932970282));
#13864=CARTESIAN_POINT('Ctrl Pts',(0.75639125589621,-3.13336083025854,-36.951938746646));
#13865=CARTESIAN_POINT('Ctrl Pts',(0.65139547328786,-3.15654719577191,-36.9584326283996));
#13866=CARTESIAN_POINT('Ctrl Pts',(0.607656632736124,-3.16525818512124,
-36.9611527690314));
#13867=CARTESIAN_POINT('Ctrl Pts',(0.516559441526132,-3.18144329121965,
-36.9668556214862));
#13868=CARTESIAN_POINT('Ctrl Pts',(0.469187086298851,-3.18877377161861,
-36.9698420269909));
#13869=CARTESIAN_POINT('Ctrl Pts',(0.339146236760602,-3.20593610539624,
-36.9781031196637));
#13870=CARTESIAN_POINT('Ctrl Pts',(0.256237029098309,-3.21362523549382,
-36.9834403536453));
#13871=CARTESIAN_POINT('Ctrl Pts',(0.0608915632147329,-3.22413451724012,
-36.9961807350572));
#13872=CARTESIAN_POINT('Ctrl Pts',(-0.0515763266788825,-3.2242964598372,
-37.0036454861312));
#13873=CARTESIAN_POINT('Ctrl Pts',(-0.377242808422039,-3.2077211125975,
-37.0255118287511));
#13874=CARTESIAN_POINT('Ctrl Pts',(-0.589066298771854,-3.17565658689,-37.0400778136248));
#13875=CARTESIAN_POINT('Ctrl Pts',(-0.836336814109508,-3.11261581597723,
-37.0566133944375));
#13876=CARTESIAN_POINT('Ctrl Pts',(-0.876312396007306,-3.1015985284818,
-37.0592700731461));
#13877=CARTESIAN_POINT('Ctrl Pts',(-0.940583574594114,-3.08254343633048,
-37.0635026256295));
#13878=CARTESIAN_POINT('Ctrl Pts',(-0.965014841209167,-3.07498260518654,
-37.0651022753642));
#13879=CARTESIAN_POINT('Ctrl Pts',(-1.01659581645663,-3.05834428457822,
-37.0684566605088));
#13880=CARTESIAN_POINT('Ctrl Pts',(-1.04371917407903,-3.04919452269436,
-37.0702075178538));
#13881=CARTESIAN_POINT('Ctrl Pts',(-1.12417147106392,-3.02085548280124,
-37.0753718167645));
#13882=CARTESIAN_POINT('Ctrl Pts',(-1.17712226169957,-3.00061882444818,
-37.0787324587866));
#13883=CARTESIAN_POINT('Ctrl Pts',(-1.30598297217461,-2.94743438703454,
-37.0868784798277));
#13884=CARTESIAN_POINT('Ctrl Pts',(-1.38121164644181,-2.91293954888571,
-37.0916061304529));
#13885=CARTESIAN_POINT('Ctrl Pts',(-1.69144739912402,-2.75596172690494,
-37.1112983327154));
#13886=CARTESIAN_POINT('Ctrl Pts',(-1.91219153594532,-2.60764988758928,
-37.1258917416526));
#13887=CARTESIAN_POINT('Ctrl Pts',(-2.15721263353127,-2.39501325979633,
-37.1450212180986));
#13888=CARTESIAN_POINT('Ctrl Pts',(-2.20104154479816,-2.35479730056485,
-37.1485710324401));
#13889=CARTESIAN_POINT('Ctrl Pts',(-2.27542291640106,-2.28265575892519,
-37.1548423691386));
#13890=CARTESIAN_POINT('Ctrl Pts',(-2.30647877449684,-2.25127122588317,
-37.1575409291374));
#13891=CARTESIAN_POINT('Ctrl Pts',(-2.37085500912079,-2.18348309534915,
-37.1633142658819));
#13892=CARTESIAN_POINT('Ctrl Pts',(-2.40400336629703,-2.14693253240028,
-37.1663952099519));
#13893=CARTESIAN_POINT('Ctrl Pts',(-2.49644478741192,-2.04017725659565,
-37.1753111672561));
#13894=CARTESIAN_POINT('Ctrl Pts',(-2.55358829565566,-1.96818294426044,
-37.1812270680578));
#13895=CARTESIAN_POINT('Ctrl Pts',(-2.68530530037351,-1.78682661140694,
-37.1958965725635));
#13896=CARTESIAN_POINT('Ctrl Pts',(-2.75636778853909,-1.67512559756117,
-37.2047440612377));
#13897=CARTESIAN_POINT('Ctrl Pts',(-2.90792107484353,-1.40102032046565,
-37.2258238768182));
#13898=CARTESIAN_POINT('Ctrl Pts',(-2.98199181887782,-1.23555487708316,
-37.238074921831));
#13899=CARTESIAN_POINT('Ctrl Pts',(-3.05523282257704,-1.02631719928974,
-37.252428709054));
#13900=CARTESIAN_POINT('Ctrl Pts',(-3.06795312656356,-0.987642927626157,
-37.2550352577364));
#13901=CARTESIAN_POINT('Ctrl Pts',(-3.08743004550622,-0.924413857459189,
-37.2592103671183));
#13902=CARTESIAN_POINT('Ctrl Pts',(-3.09463422985292,-0.900002454551657,
-37.2608015267464));
#13903=CARTESIAN_POINT('Ctrl Pts',(-3.10939766023268,-0.847701861001912,
-37.2641633380954));
#13904=CARTESIAN_POINT('Ctrl Pts',(-3.11687240680839,-0.819791919985914,
-37.2659296063928));
#13905=CARTESIAN_POINT('Ctrl Pts',(-3.13827826839333,-0.735335445456807,
-37.2712013590898));
#13906=CARTESIAN_POINT('Ctrl Pts',(-3.15105372240961,-0.678505717752124,
-37.2746506684513));
#13907=CARTESIAN_POINT('Ctrl Pts',(-3.17891307704552,-0.536720748012749,
-37.2830834212154));
#13908=CARTESIAN_POINT('Ctrl Pts',(-3.19213968603264,-0.451445793672037,
-37.2880036293125));
#13909=CARTESIAN_POINT('Ctrl Pts',(-3.23087576436145,-0.112323534104255,
-37.3073099808694));
#13910=CARTESIAN_POINT('Ctrl Pts',(-3.22963530472755,0.143613498771788,
-37.3213889182298));
#13911=CARTESIAN_POINT('Ctrl Pts',(-3.19071554804759,0.45736858803147,-37.3400006676139));
#13912=CARTESIAN_POINT('Ctrl Pts',(-3.1814701780575,0.517782327082446,-37.3436427334051));
#13913=CARTESIAN_POINT('Ctrl Pts',(-3.16256191119151,0.62151918679783,-37.3500179182935));
#13914=CARTESIAN_POINT('Ctrl Pts',(-3.15371106808167,0.664973792715772,
-37.3527255770841));
#13915=CARTESIAN_POINT('Ctrl Pts',(-3.13328502681066,0.755648800556685,
-37.3584601315694));
#13916=CARTESIAN_POINT('Ctrl Pts',(-3.1215323300654,0.80281734008179,-37.361491949208));
#13917=CARTESIAN_POINT('Ctrl Pts',(-3.08569003217087,0.933950180492215,
-37.3700643226131));
#13918=CARTESIAN_POINT('Ctrl Pts',(-3.05924860296201,1.01722254567061,-37.3756758970466));
#13919=CARTESIAN_POINT('Ctrl Pts',(-2.98802080924565,1.21351041314089,-37.3893079125053));
#13920=CARTESIAN_POINT('Ctrl Pts',(-2.94016050826175,1.3252652804794,-37.3974039158715));
#13921=CARTESIAN_POINT('Ctrl Pts',(-2.79541636473548,1.61657255940743,-37.419261693474));
#13922=CARTESIAN_POINT('Ctrl Pts',(-2.6876070469541,1.7900941156866,-37.4331167519453));
#13923=CARTESIAN_POINT('Ctrl Pts',(-2.54086284320336,1.98282830846227,-37.4487612471043));
#13924=CARTESIAN_POINT('Ctrl Pts',(-2.51705578706488,2.0129636235733,-37.4512143910582));
#13925=CARTESIAN_POINT('Ctrl Pts',(-2.47664069178851,2.06228309955132,-37.4552313417631));
#13926=CARTESIAN_POINT('Ctrl Pts',(-2.46033516072461,2.08170885608321,-37.4568138685713));
#13927=CARTESIAN_POINT('Ctrl Pts',(-2.4242346770514,2.12370068041981,-37.4602332901854));
#13928=CARTESIAN_POINT('Ctrl Pts',(-2.40435103968709,2.14618605423676,-37.4620641605057));
#13929=CARTESIAN_POINT('Ctrl Pts',(-2.34037455674722,2.21652846608821,-37.4678035365746));
#13930=CARTESIAN_POINT('Ctrl Pts',(-2.29514289246163,2.26333200410626,-37.471640077336));
#13931=CARTESIAN_POINT('Ctrl Pts',(-2.17477526409264,2.38056029568585,-37.4813957823589));
#13932=CARTESIAN_POINT('Ctrl Pts',(-2.09762540973359,2.44881289968059,-37.487223094372));
#13933=CARTESIAN_POINT('Ctrl Pts',(-1.8388721672032,2.6565084350534,-37.5059091950354));
#13934=CARTESIAN_POINT('Ctrl Pts',(-1.64567290055719,2.78033087841417,-37.5186475156818));
#13935=CARTESIAN_POINT('Ctrl Pts',(-1.38660072774091,2.90983746461253,-37.5357030378488));
#13936=CARTESIAN_POINT('Ctrl Pts',(-1.33145051273807,2.93548198566862,-37.5393283976233));
#13937=CARTESIAN_POINT('Ctrl Pts',(-1.23491971576535,2.97708820394792,-37.5456848044145));
#13938=CARTESIAN_POINT('Ctrl Pts',(-1.19387337201152,2.9937847208708,-37.5483908505492));
#13939=CARTESIAN_POINT('Ctrl Pts',(-1.10698457413611,3.02705762747664,-37.5541322270884));
#13940=CARTESIAN_POINT('Ctrl Pts',(-1.06108439000323,3.04345071288269,-37.5571726978799));
#13941=CARTESIAN_POINT('Ctrl Pts',(-0.931197344000002,3.08654398550227,
-37.5658041048123));
#13942=CARTESIAN_POINT('Ctrl Pts',(-0.846466550857527,3.11084785851076,
-37.5714676993067));
#13943=CARTESIAN_POINT('Ctrl Pts',(-0.64106341765264,3.16075175310816,-37.5852732810637));
#13944=CARTESIAN_POINT('Ctrl Pts',(-0.519712022346255,3.18295605398513,
-37.5934937229118));
#13945=CARTESIAN_POINT('Ctrl Pts',(-0.19912849305455,3.22279106802224,-37.6152079394678));
#13946=CARTESIAN_POINT('Ctrl Pts',(0.0010100672380102,3.22893827289216,
-37.6287794571775));
#13947=CARTESIAN_POINT('Ctrl Pts',(0.239210334686556,3.21409476085178,-37.6442006335225));
#13948=CARTESIAN_POINT('Ctrl Pts',(0.277938100015091,3.21097764456997,-37.6466835403259));
#13949=CARTESIAN_POINT('Ctrl Pts',(0.341906645307251,3.2046628492782,-37.6507343620222));
#13950=CARTESIAN_POINT('Ctrl Pts',(0.367181967903874,3.20186534735771,-37.6523216745831));
#13951=CARTESIAN_POINT('Ctrl Pts',(0.422023658344153,3.19513738894977,-37.6557345600265));
#13952=CARTESIAN_POINT('Ctrl Pts',(0.451572968407502,3.19109525181101,-37.6575544676143));
#13953=CARTESIAN_POINT('Ctrl Pts',(0.544151207460026,3.17711942422927,-37.6632083345519));
#13954=CARTESIAN_POINT('Ctrl Pts',(0.606946870924651,3.16572344993154,-37.6669734338793));
#13955=CARTESIAN_POINT('Ctrl Pts',(0.766878093718888,3.13176510842158,-37.6764754408824));
#13956=CARTESIAN_POINT('Ctrl Pts',(0.863381578175057,3.10654615806019,-37.6821264776748));
#13957=CARTESIAN_POINT('Ctrl Pts',(1.18383383824032,3.00671351396365,-37.701042629767));
#13958=CARTESIAN_POINT('Ctrl Pts',(1.4006954226164,2.91201514955137,-37.7141566257034));
#13959=CARTESIAN_POINT('Ctrl Pts',(1.65721649088791,2.76465902735695,-37.7315932656678));
#13960=CARTESIAN_POINT('Ctrl Pts',(1.70831540366137,2.73337956605624,-37.7351674005065));
#13961=CARTESIAN_POINT('Ctrl Pts',(1.79555896916883,2.67657244486789,-37.7414666677254));
#13962=CARTESIAN_POINT('Ctrl Pts',(1.83210537742337,2.65169033956436,-37.7441682072329));
#13963=CARTESIAN_POINT('Ctrl Pts',(1.9081861862424,2.59756806694281,-37.7499328752155));
#13964=CARTESIAN_POINT('Ctrl Pts',(1.94758614415828,2.56815929828049,-37.7530018489588));
#13965=CARTESIAN_POINT('Ctrl Pts',(2.05772358588289,2.4819585511367,-37.7618293980166));
#13966=CARTESIAN_POINT('Ctrl Pts',(2.1267529474346,2.42306914216833,-37.7676662136421));
#13967=CARTESIAN_POINT('Ctrl Pts',(2.28799626571639,2.27330776958204,-37.7820595395862));
#13968=CARTESIAN_POINT('Ctrl Pts',(2.37739572758953,2.17964220445891,-37.7907047886177));
#13969=CARTESIAN_POINT('Ctrl Pts',(2.58145336776289,1.9383150342948,-37.8119672389101));
#13970=CARTESIAN_POINT('Ctrl Pts',(2.68938145637623,1.78555382187953,-37.8246189284822));
#13971=CARTESIAN_POINT('Ctrl Pts',(2.80377266717897,1.58952737727943,-37.8393071831893));
#13972=CARTESIAN_POINT('Ctrl Pts',(2.82341196639628,1.55437564829835,-37.841884019212));
#13973=CARTESIAN_POINT('Ctrl Pts',(2.85434878912896,1.49648073382498,-37.8460250691588));
#13974=CARTESIAN_POINT('Ctrl Pts',(2.86604503278857,1.47395645639384,-37.8476111927161));
#13975=CARTESIAN_POINT('Ctrl Pts',(2.89055298824072,1.42536464879731,-37.8509768166654));
#13976=CARTESIAN_POINT('Ctrl Pts',(2.90328055141569,1.39925806745773,-37.852751638427));
#13977=CARTESIAN_POINT('Ctrl Pts',(2.94086659208732,1.31944063753356,-37.8580876884661));
#13978=CARTESIAN_POINT('Ctrl Pts',(2.96460126551952,1.2652115024049,-37.8615906009248));
#13979=CARTESIAN_POINT('Ctrl Pts',(3.02005082158743,1.12837704823534,-37.8702000133257));
#13980=CARTESIAN_POINT('Ctrl Pts',(3.04988390963164,1.04506053216023,-37.8752396878314));
#13981=CARTESIAN_POINT('Ctrl Pts',(3.15053554888574,0.722736983060389,-37.8943235197578));
#13982=CARTESIAN_POINT('Ctrl Pts',(3.1969720521322,0.477060361114301,-37.9080953797963));
#13983=CARTESIAN_POINT('Ctrl Pts',(3.2190412275143,0.166567907088179,-37.926401410525));
#13984=CARTESIAN_POINT('Ctrl Pts',(3.22165222442586,0.104534703803008,-37.9300981335659));
#13985=CARTESIAN_POINT('Ctrl Pts',(3.22305591521284,-0.00197835242181084,
-37.9365343329445));
#13986=CARTESIAN_POINT('Ctrl Pts',(3.22272203532739,-0.0464298595534938,
-37.939246806003));
#13987=CARTESIAN_POINT('Ctrl Pts',(3.2201106075036,-0.139020218365842,-37.9449583445058));
#13988=CARTESIAN_POINT('Ctrl Pts',(3.21767245203043,-0.18714312022975,-37.9479616256255));
#13989=CARTESIAN_POINT('Ctrl Pts',(3.20796289165827,-0.319835277845849,
-37.9563453308025));
#13990=CARTESIAN_POINT('Ctrl Pts',(3.19842851436289,-0.40419492256789,-37.9617916941235));
#13991=CARTESIAN_POINT('Ctrl Pts',(3.16801459310315,-0.602701299123028,
-37.9748836704233));
#13992=CARTESIAN_POINT('Ctrl Pts',(3.14427935947758,-0.716288347962332,
-37.9825962776455));
#13993=CARTESIAN_POINT('Ctrl Pts',(3.06068975381992,-1.03057642115649,-38.0044246240833));
#13994=CARTESIAN_POINT('Ctrl Pts',(2.9873309965288,-1.22709855207136,-38.0186739640594));
#13995=CARTESIAN_POINT('Ctrl Pts',(2.87766210121168,-1.45148762481557,-38.034841967959));
#13996=CARTESIAN_POINT('Ctrl Pts',(2.85920660834066,-1.4875124890563,-38.0374329869506));
#13997=CARTESIAN_POINT('Ctrl Pts',(2.828070157859,-1.5455685217396,-38.0415897612611));
#13998=CARTESIAN_POINT('Ctrl Pts',(2.81579896211066,-1.56781352432736,-38.0431777700064));
#13999=CARTESIAN_POINT('Ctrl Pts',(2.78897719051659,-1.61510450283525,-38.046540640982));
#14000=CARTESIAN_POINT('Ctrl Pts',(2.77434984684862,-1.64010346937344,-38.04831097003));
#14001=CARTESIAN_POINT('Ctrl Pts',(2.72909016981954,-1.7151162292903,-38.0536110953751));
#14002=CARTESIAN_POINT('Ctrl Pts',(2.69742649943247,-1.76449652722705,-38.0570838083759));
#14003=CARTESIAN_POINT('Ctrl Pts',(2.61538227873249,-1.88507158489489,-38.0655922661487));
#14004=CARTESIAN_POINT('Ctrl Pts',(2.56342602756872,-1.95513885638657,-38.0705632772635));
#14005=CARTESIAN_POINT('Ctrl Pts',(2.43364121459208,-2.11608163164715,-38.0822536746435));
#14006=CARTESIAN_POINT('Ctrl Pts',(2.35353954212797,-2.20481568628638,-38.088924234407));
#14007=CARTESIAN_POINT('Ctrl Pts',(2.26878001451759,-2.28883263001591,-38.0956657793148));
#14008=CARTESIAN_POINT('Ctrl Pts',(2.26878020134171,-2.28883244482855,-38.344825298285));
#14009=CARTESIAN_POINT('Ctrl Pts',(2.27165473796579,-2.2859830917466,-38.3445913823381));
#14010=CARTESIAN_POINT('Ctrl Pts',(2.27452397086319,-2.2831282600329,-38.3443572989667));
#14011=CARTESIAN_POINT('Ctrl Pts',(2.33728119711145,-2.22045029895543,-38.3392240548976));
#14012=CARTESIAN_POINT('Ctrl Pts',(2.39479059336495,-2.15830009166445,-38.3342536326079));
#14013=CARTESIAN_POINT('Ctrl Pts',(2.48117376581954,-2.05723801477477,-38.3262930186285));
#14014=CARTESIAN_POINT('Ctrl Pts',(2.51173240763389,-2.01981470641953,-38.3233698719877));
#14015=CARTESIAN_POINT('Ctrl Pts',(2.56895635862974,-1.94642842073486,-38.3176751722873));
#14016=CARTESIAN_POINT('Ctrl Pts',(2.5957362913412,-1.9105688069594,-38.3149089432171));
#14017=CARTESIAN_POINT('Ctrl Pts',(2.65831344742135,-1.82302992032227,-38.3081891338843));
#14018=CARTESIAN_POINT('Ctrl Pts',(2.6933610757823,-1.77083984024132,-38.3042092848356));
#14019=CARTESIAN_POINT('Ctrl Pts',(2.8084074537765,-1.58819891998019,-38.2903617376354));
#14020=CARTESIAN_POINT('Ctrl Pts',(2.88062399551668,-1.45310837738793,-38.2802432098167));
#14021=CARTESIAN_POINT('Ctrl Pts',(3.02443360285753,-1.13087431368775,-38.2565738867371));
#14022=CARTESIAN_POINT('Ctrl Pts',(3.08874124059288,-0.94114693343855,-38.2429612400691));
#14023=CARTESIAN_POINT('Ctrl Pts',(3.14661130301666,-0.698170179423578,
-38.2266496987288));
#14024=CARTESIAN_POINT('Ctrl Pts',(3.15703825191403,-0.649395378250362,
-38.2234317481557));
#14025=CARTESIAN_POINT('Ctrl Pts',(3.17143641476915,-0.573463212716543,
-38.2185282831025));
#14026=CARTESIAN_POINT('Ctrl Pts',(3.17619965662134,-0.546465783410158,
-38.216805500934));
#14027=CARTESIAN_POINT('Ctrl Pts',(3.18437954695069,-0.496376033402855,
-38.2136512529005));
#14028=CARTESIAN_POINT('Ctrl Pts',(3.18789081486779,-0.47330166209682,-38.2122148635845));
#14029=CARTESIAN_POINT('Ctrl Pts',(3.19704019465122,-0.408446798069404,
-38.2082192915786));
#14030=CARTESIAN_POINT('Ctrl Pts',(3.20210985605113,-0.366589191315778,
-38.2056888441778));
#14031=CARTESIAN_POINT('Ctrl Pts',(3.22210160425585,-0.169138840918346,
-38.1939290625036));
#14032=CARTESIAN_POINT('Ctrl Pts',(3.22651440091117,-0.0126808017563364,
-38.1851190847756));
#14033=CARTESIAN_POINT('Ctrl Pts',(3.21306128460206,0.289168827813927,-38.1681348769976));
#14034=CARTESIAN_POINT('Ctrl Pts',(3.19668896002065,0.434233744232097,-38.1599758637728));
#14035=CARTESIAN_POINT('Ctrl Pts',(3.15316504134073,0.673108926160731,-38.1460328667813));
#14036=CARTESIAN_POINT('Ctrl Pts',(3.13148095010002,0.767691412365471,-38.1403778406849));
#14037=CARTESIAN_POINT('Ctrl Pts',(3.09222195982493,0.909271679335177,-38.131616180453));
#14038=CARTESIAN_POINT('Ctrl Pts',(3.07776113113975,0.957077660267318,-38.128605585575));
#14039=CARTESIAN_POINT('Ctrl Pts',(3.04857486485327,1.04604899943607,-38.1228939317893));
#14040=CARTESIAN_POINT('Ctrl Pts',(3.03411118073422,1.08728849400791,-38.1202018145761));
#14041=CARTESIAN_POINT('Ctrl Pts',(2.99908732392589,1.18100296592571,-38.1139755340226));
#14042=CARTESIAN_POINT('Ctrl Pts',(2.97798073577599,1.23325702772943,-38.1104242587957));
#14043=CARTESIAN_POINT('Ctrl Pts',(2.85262327461581,1.52159681219223,-38.0903663194394));
#14044=CARTESIAN_POINT('Ctrl Pts',(2.7216890709309,1.74501638187759,-38.0729606187827));
#14045=CARTESIAN_POINT('Ctrl Pts',(2.5102820556353,2.02310252600544,-38.0494496077613));
#14046=CARTESIAN_POINT('Ctrl Pts',(2.45193721640244,2.09343384765107,-38.0433298838923));
#14047=CARTESIAN_POINT('Ctrl Pts',(2.35019718567448,2.20597714833772,-38.0333455934372));
#14048=CARTESIAN_POINT('Ctrl Pts',(2.30846019730029,2.24961651861663,-38.0294222082498));
#14049=CARTESIAN_POINT('Ctrl Pts',(2.24479241847086,2.31254705214783,-38.0237178621356));
#14050=CARTESIAN_POINT('Ctrl Pts',(2.22378780579074,2.33275262487673,-38.0218788319707));
#14051=CARTESIAN_POINT('Ctrl Pts',(2.18408947651563,2.36991719229273,-38.0184869689903));
#14052=CARTESIAN_POINT('Ctrl Pts',(2.16546596637975,2.38694606527149,-38.0169295276647));
#14053=CARTESIAN_POINT('Ctrl Pts',(2.11717928420632,2.43006789568504,-38.0129722320241));
#14054=CARTESIAN_POINT('Ctrl Pts',(2.08723188216769,2.4558382441225,-38.0105940023849));
#14055=CARTESIAN_POINT('Ctrl Pts',(1.90741400056747,2.60490901225448,-37.996705216883));
#14056=CARTESIAN_POINT('Ctrl Pts',(1.74711244564422,2.71503104984654,-37.9858786194218));
#14057=CARTESIAN_POINT('Ctrl Pts',(1.46796802255642,2.87177146020033,-37.9678804646102));
#14058=CARTESIAN_POINT('Ctrl Pts',(1.35455454523371,2.92697473963885,-37.9607782171537));
#14059=CARTESIAN_POINT('Ctrl Pts',(1.15570854589672,3.0097241715196,-37.9483547195677));
#14060=CARTESIAN_POINT('Ctrl Pts',(1.07182567112627,3.04060679029611,-37.9431233706838));
#14061=CARTESIAN_POINT('Ctrl Pts',(0.940123047463643,3.08296732769151,-37.9348543001324));
#14062=CARTESIAN_POINT('Ctrl Pts',(0.893139190966295,3.09690504992285,-37.9318940797336));
#14063=CARTESIAN_POINT('Ctrl Pts',(0.803052859161704,3.12140857221847,-37.9261892204013));
#14064=CARTESIAN_POINT('Ctrl Pts',(0.760013997471235,3.13216599044381,-37.9234513557489));
#14065=CARTESIAN_POINT('Ctrl Pts',(0.657686482147988,3.15550921112142,-37.9169071005329));
#14066=CARTESIAN_POINT('Ctrl Pts',(0.598239500672287,3.16731726001198,-37.9130777288064));
#14067=CARTESIAN_POINT('Ctrl Pts',(0.312020075524238,3.21582438418708,-37.8944976847947));
#14068=CARTESIAN_POINT('Ctrl Pts',(0.0821172869127146,3.22987774663927,
-37.8790812014648));
#14069=CARTESIAN_POINT('Ctrl Pts',(-0.249118151567528,3.21472381895837,
-37.8567654922359));
#14070=CARTESIAN_POINT('Ctrl Pts',(-0.350676446671104,3.2052358492194,-37.8499206341811));
#14071=CARTESIAN_POINT('Ctrl Pts',(-0.51566289264444,3.18188517695293,-37.8389357872099));
#14072=CARTESIAN_POINT('Ctrl Pts',(-0.579425121929288,3.17089406489248,
-37.8347245081003));
#14073=CARTESIAN_POINT('Ctrl Pts',(-0.672221685925151,3.15200507709747,
-37.8286844756345));
#14074=CARTESIAN_POINT('Ctrl Pts',(-0.701542258503872,3.14560910070194,
-37.8267892111906));
#14075=CARTESIAN_POINT('Ctrl Pts',(-0.755555731291702,3.13303378668247,
-37.8233274876798));
#14076=CARTESIAN_POINT('Ctrl Pts',(-0.780270237289268,3.12697034897802,
-37.8217557123886));
#14077=CARTESIAN_POINT('Ctrl Pts',(-0.842426723475524,3.110938076983,-37.8178294684548));
#14078=CARTESIAN_POINT('Ctrl Pts',(-0.879765219573846,3.10058574433759,
-37.815495039914));
#14079=CARTESIAN_POINT('Ctrl Pts',(-1.10940055459906,3.0324353491069,-37.8012372224427));
#14080=CARTESIAN_POINT('Ctrl Pts',(-1.29615333912781,2.95743778531122,-37.7900550043966));
#14081=CARTESIAN_POINT('Ctrl Pts',(-1.58386467065014,2.80936935740552,-37.7718567513543));
#14082=CARTESIAN_POINT('Ctrl Pts',(-1.68970081467572,2.74701517829149,-37.7649309759927));
#14083=CARTESIAN_POINT('Ctrl Pts',(-1.86476915145129,2.62991963582593,-37.7527718483158));
#14084=CARTESIAN_POINT('Ctrl Pts',(-1.93578556139886,2.57809497685447,-37.7476227465077));
#14085=CARTESIAN_POINT('Ctrl Pts',(-2.04273006991471,2.49313935566136,-37.7394557677428));
#14086=CARTESIAN_POINT('Ctrl Pts',(-2.08017502740776,2.46198323741499,-37.736512301795));
#14087=CARTESIAN_POINT('Ctrl Pts',(-2.1503292694726,2.40086805639257,-37.7308250287658));
#14088=CARTESIAN_POINT('Ctrl Pts',(-2.18315446071986,2.37105876993493,-37.7280876212882));
#14089=CARTESIAN_POINT('Ctrl Pts',(-2.25961185074089,2.29869213355574,-37.7215212625154));
#14090=CARTESIAN_POINT('Ctrl Pts',(-2.30267103764056,2.25555681683872,-37.7176686810892));
#14091=CARTESIAN_POINT('Ctrl Pts',(-2.5204886100954,2.02461338064273,-37.6973396820467));
#14092=CARTESIAN_POINT('Ctrl Pts',(-2.67356470774371,1.81767279471486,-37.6800049339823));
#14093=CARTESIAN_POINT('Ctrl Pts',(-2.84296091881277,1.520218010426,-37.6570025041703));
#14094=CARTESIAN_POINT('Ctrl Pts',(-2.88245381252503,1.44393594396125,-37.6512637040534));
#14095=CARTESIAN_POINT('Ctrl Pts',(-2.9434697895925,1.31357332854842,-37.64180917393));
#14096=CARTESIAN_POINT('Ctrl Pts',(-2.96666074642067,1.26032304650454,-37.6380419089829));
#14097=CARTESIAN_POINT('Ctrl Pts',(-2.9992062980479,1.17970850993814,-37.632507870223));
#14098=CARTESIAN_POINT('Ctrl Pts',(-3.00965160544775,1.15280004331367,-37.630688281417));
#14099=CARTESIAN_POINT('Ctrl Pts',(-3.02862287431501,1.10191130135672,-37.6273035930529));
#14100=CARTESIAN_POINT('Ctrl Pts',(-3.03722863417711,1.07796441786877,-37.6257345581336));
#14101=CARTESIAN_POINT('Ctrl Pts',(-3.05887059356578,1.01542473126594,-37.6216930730648));
#14102=CARTESIAN_POINT('Ctrl Pts',(-3.07146080753454,0.976680879071006,
-37.619244202684));
#14103=CARTESIAN_POINT('Ctrl Pts',(-3.13576063457448,0.765253878824999,
-37.6061245389506));
#14104=CARTESIAN_POINT('Ctrl Pts',(-3.17365247230519,0.588686371692925,
-37.5960306659801));
#14105=CARTESIAN_POINT('Ctrl Pts',(-3.21345246228294,0.278279245276633,
-37.5784425206236));
#14106=CARTESIAN_POINT('Ctrl Pts',(-3.22218255573067,0.145785185533111,
-37.5709850725669));
#14107=CARTESIAN_POINT('Ctrl Pts',(-3.22309832160539,-0.0788896773562119,
-37.5580454959396));
#14108=CARTESIAN_POINT('Ctrl Pts',(-3.21953156783552,-0.170882403457803,
-37.5526655478121));
#14109=CARTESIAN_POINT('Ctrl Pts',(-3.20801406649237,-0.311765193062044,
-37.5442235958648));
#14110=CARTESIAN_POINT('Ctrl Pts',(-3.20286548072224,-0.360838060283908,
-37.5412453473283));
#14111=CARTESIAN_POINT('Ctrl Pts',(-3.19098467755158,-0.453519194078132,
-37.535539155528));
#14112=CARTESIAN_POINT('Ctrl Pts',(-3.18447940253439,-0.497145360915337,
-37.5328187782859));
#14113=CARTESIAN_POINT('Ctrl Pts',(-3.1671265731411,-0.599122854422057,
-37.5263731989797));
#14114=CARTESIAN_POINT('Ctrl Pts',(-3.15555869138312,-0.657333666120761,
-37.5226266992922));
#14115=CARTESIAN_POINT('Ctrl Pts',(-3.08905306072559,-0.949545461999719,
-37.5034658351552));
#14116=CARTESIAN_POINT('Ctrl Pts',(-3.00967224895398,-1.17716791912406,
-37.4873036305016));
#14117=CARTESIAN_POINT('Ctrl Pts',(-2.8633944082986,-1.48212104540801,-37.4645354758524));
#14118=CARTESIAN_POINT('Ctrl Pts',(-2.81702941848359,-1.56845697060663,
-37.4579631907309));
#14119=CARTESIAN_POINT('Ctrl Pts',(-2.73444297117563,-1.70672832789192,
-37.4473512783489));
#14120=CARTESIAN_POINT('Ctrl Pts',(-2.70049699380034,-1.75994801506134,
-37.4432450221919));
#14121=CARTESIAN_POINT('Ctrl Pts',(-2.64831334313962,-1.83669145117825,
-37.4373274845656));
#14122=CARTESIAN_POINT('Ctrl Pts',(-2.63127964940723,-1.86101225332141,
-37.4354527676264));
#14123=CARTESIAN_POINT('Ctrl Pts',(-2.59902664965847,-1.9057349229102,-37.4320116797367));
#14124=CARTESIAN_POINT('Ctrl Pts',(-2.58389874989663,-1.92619635664796,
-37.4304403967975));
#14125=CARTESIAN_POINT('Ctrl Pts',(-2.54495411727566,-1.97758681487464,
-37.4264974566633));
#14126=CARTESIAN_POINT('Ctrl Pts',(-2.52081508416879,-2.00826608877016,
-37.4241463904307));
#14127=CARTESIAN_POINT('Ctrl Pts',(-2.3707921899393,-2.1919676012109,-37.4100348518224));
#14128=CARTESIAN_POINT('Ctrl Pts',(-2.23156057411662,-2.33356644108525,
-37.3989932589583));
#14129=CARTESIAN_POINT('Ctrl Pts',(-1.98545025213148,-2.54155279390823,
-37.3808751831953));
#14130=CARTESIAN_POINT('Ctrl Pts',(-1.88617116396231,-2.61607709750948,
-37.3738802891545));
#14131=CARTESIAN_POINT('Ctrl Pts',(-1.70916031291056,-2.73362637923154,
-37.3616180156489));
#14132=CARTESIAN_POINT('Ctrl Pts',(-1.63349357892053,-2.77950337699727,
-37.3564371575791));
#14133=CARTESIAN_POINT('Ctrl Pts',(-1.51330441669205,-2.84577033926732,
-37.3482320588409));
#14134=CARTESIAN_POINT('Ctrl Pts',(-1.47004101513924,-2.86835808676202,
-37.3452834965974));
#14135=CARTESIAN_POINT('Ctrl Pts',(-1.38654949681861,-2.90956377465475,
-37.3395931763765));
#14136=CARTESIAN_POINT('Ctrl Pts',(-1.34641731772463,-2.92835123774248,
-37.336857982385));
#14137=CARTESIAN_POINT('Ctrl Pts',(-1.25040069938937,-2.97090938185656,
-37.3303082532387));
#14138=CARTESIAN_POINT('Ctrl Pts',(-1.19420821932128,-2.99393894765704,
-37.3264704241723));
#14139=CARTESIAN_POINT('Ctrl Pts',(-0.922691703143771,-3.09635546071641,
-37.3078923355994));
#14140=CARTESIAN_POINT('Ctrl Pts',(-0.699973903237812,-3.15416932650819,
-37.2924866311282));
#14141=CARTESIAN_POINT('Ctrl Pts',(-0.371595256884859,-3.20289767077732,
-37.2701339895035));
#14142=CARTESIAN_POINT('Ctrl Pts',(-0.269478967605364,-3.21310120746428,
-37.2632435857226));
#14143=CARTESIAN_POINT('Ctrl Pts',(-0.102211660402182,-3.22178292120925,
-37.2521973768242));
#14144=CARTESIAN_POINT('Ctrl Pts',(-0.037285516713679,-3.22318838502173,
-37.2479690811891));
#14145=CARTESIAN_POINT('Ctrl Pts',(0.057640407328837,-3.22237413426154,
-37.2419130170813));
#14146=CARTESIAN_POINT('Ctrl Pts',(0.0876341397706829,-3.22169798233136,
-37.2400179163342));
#14147=CARTESIAN_POINT('Ctrl Pts',(0.142977769507828,-3.21967685214438,
-37.2365604018247));
#14148=CARTESIAN_POINT('Ctrl Pts',(0.16832679075914,-3.21845114938461,-37.2349925782557));
#14149=CARTESIAN_POINT('Ctrl Pts',(0.232072714007886,-3.21461360458662,
-37.2310857203621));
#14150=CARTESIAN_POINT('Ctrl Pts',(0.270441858641376,-3.21161328055527,
-37.2287663813698));
#14151=CARTESIAN_POINT('Ctrl Pts',(0.510892767642874,-3.18847085508226,
-37.2143835673812));
#14152=CARTESIAN_POINT('Ctrl Pts',(0.710767523240319,-3.14995015062899,
-37.2030822114829));
#14153=CARTESIAN_POINT('Ctrl Pts',(1.02258776042949,-3.05863780125785,-37.1848089044967));
#14154=CARTESIAN_POINT('Ctrl Pts',(1.13743272318657,-3.01781303086743,-37.1779349305185));
#14155=CARTESIAN_POINT('Ctrl Pts',(1.33031802021586,-2.93666877169308,-37.1658523433417));
#14156=CARTESIAN_POINT('Ctrl Pts',(1.40952906066172,-2.89948194125591,-37.1607264147894));
#14157=CARTESIAN_POINT('Ctrl Pts',(1.53026951546676,-2.836680768831,-37.1525878490591));
#14158=CARTESIAN_POINT('Ctrl Pts',(1.57289841346733,-2.81326727797083,-37.1496487849099));
#14159=CARTESIAN_POINT('Ctrl Pts',(1.65335182683059,-2.76667877970481,-37.1439656231952));
#14160=CARTESIAN_POINT('Ctrl Pts',(1.69125979135601,-2.74366975961099,-37.1412278169675));
#14161=CARTESIAN_POINT('Ctrl Pts',(1.78021565882626,-2.68713204233637,-37.1346530707924));
#14162=CARTESIAN_POINT('Ctrl Pts',(1.83080742514473,-2.65292099259234,-37.1307922927997));
#14163=CARTESIAN_POINT('Ctrl Pts',(2.01842830872305,-2.5181248694824,-37.1159967540171));
#14164=CARTESIAN_POINT('Ctrl Pts',(2.14828130876245,-2.40827565919211,-37.1047397524462));
#14165=CARTESIAN_POINT('Ctrl Pts',(2.26878021215176,-2.28883243411322,-37.0933419659928));
#14166=CARTESIAN_POINT('Origin',(0.,0.,-41.3107734492731));
#14167=CARTESIAN_POINT('',(2.26878020052865,-2.28883244563449,-35.5935118781384));
#14168=CARTESIAN_POINT('',(2.26878031087686,-2.28883233625302,-35.8411988517434));
#14169=CARTESIAN_POINT('',(2.26878020078428,-2.2888324453811,-41.3107734492731));
#14170=CARTESIAN_POINT('Ctrl Pts',(2.26878020052865,-2.28883244563449,-35.5935118781384));
#14171=CARTESIAN_POINT('Ctrl Pts',(2.26354090144405,-2.29402584371414,-35.5939651056608));
#14172=CARTESIAN_POINT('Ctrl Pts',(2.25828373912089,-2.29920128299245,-35.5944191016049));
#14173=CARTESIAN_POINT('Ctrl Pts',(2.21867188016905,-2.33793043921428,-35.5978341633605));
#14174=CARTESIAN_POINT('Ctrl Pts',(2.18359041128584,-2.37072903991118,-35.6008265966311));
#14175=CARTESIAN_POINT('Ctrl Pts',(2.08533156771503,-2.4585622132953,-35.6091284325938));
#14176=CARTESIAN_POINT('Ctrl Pts',(2.02072402227752,-2.51193319617988,-35.614501462253));
#14177=CARTESIAN_POINT('Ctrl Pts',(1.86381843778374,-2.63157606181455,-35.6273559894686));
#14178=CARTESIAN_POINT('Ctrl Pts',(1.76995242735959,-2.69560321212375,-35.6349007857385));
#14179=CARTESIAN_POINT('Ctrl Pts',(1.49276364673534,-2.86394782860756,-35.6566541046229));
#14180=CARTESIAN_POINT('Ctrl Pts',(1.30231380304113,-2.95542318951066,-35.6710132350367));
#14181=CARTESIAN_POINT('Ctrl Pts',(1.06492003862431,-3.04200905587315,-35.6873951051703));
#14182=CARTESIAN_POINT('Ctrl Pts',(1.02527125238563,-3.05560027112643,-35.6900815707981));
#14183=CARTESIAN_POINT('Ctrl Pts',(0.963128167203858,-3.07555641233828,
-35.6942037504232));
#14184=CARTESIAN_POINT('Ctrl Pts',(0.940811702225469,-3.08245625379665,
-35.6956665444774));
#14185=CARTESIAN_POINT('Ctrl Pts',(0.892043499132521,-3.09695547891241,
-35.6988222243865));
#14186=CARTESIAN_POINT('Ctrl Pts',(0.865565458393363,-3.10445992109168,
-35.7005097615375));
#14187=CARTESIAN_POINT('Ctrl Pts',(0.7901364035587,-3.12479800629861,-35.7052525540808));
#14188=CARTESIAN_POINT('Ctrl Pts',(0.740972936182149,-3.13681969877855,
-35.7082672403231));
#14189=CARTESIAN_POINT('Ctrl Pts',(0.623315263681643,-3.16266904611618,
-35.715344096899));
#14190=CARTESIAN_POINT('Ctrl Pts',(0.554613593254188,-3.1754373207095,-35.7193667605599));
#14191=CARTESIAN_POINT('Ctrl Pts',(0.354464290981182,-3.20594052595851,
-35.7309037114525));
#14192=CARTESIAN_POINT('Ctrl Pts',(0.222269848251562,-3.21780941008953,
-35.7383024390774));
#14193=CARTESIAN_POINT('Ctrl Pts',(-0.0581403100300363,-3.22561872952891,
-35.7541104422919));
#14194=CARTESIAN_POINT('Ctrl Pts',(-0.206094044542116,-3.21955218789992,
-35.7625220916176));
#14195=CARTESIAN_POINT('Ctrl Pts',(-0.415109772789401,-3.19651267891872,
-35.7748860055901));
#14196=CARTESIAN_POINT('Ctrl Pts',(-0.476904236459283,-3.1878787676546,
-35.778600272211));
#14197=CARTESIAN_POINT('Ctrl Pts',(-0.582298553132052,-3.17002015577549,
-35.7850582445273));
#14198=CARTESIAN_POINT('Ctrl Pts',(-0.626030075138798,-3.16167446764726,
-35.7877745208966));
#14199=CARTESIAN_POINT('Ctrl Pts',(-0.716648593786405,-3.14242715613542,
-35.7934861806598));
#14200=CARTESIAN_POINT('Ctrl Pts',(-0.763492081499223,-3.13137559102172,
-35.7964856151189));
#14201=CARTESIAN_POINT('Ctrl Pts',(-0.891759464810913,-3.09806489205968,
-35.8048349783755));
#14202=CARTESIAN_POINT('Ctrl Pts',(-0.972579014633753,-3.07365077547407,
-35.8102498045939));
#14203=CARTESIAN_POINT('Ctrl Pts',(-1.16095434485393,-3.00857227787655,
-35.8232384370307));
#14204=CARTESIAN_POINT('Ctrl Pts',(-1.26747417942642,-2.96527027270289,
-35.8308775671399));
#14205=CARTESIAN_POINT('Ctrl Pts',(-1.55796622961292,-2.82866426343408,
-35.8524171422834));
#14206=CARTESIAN_POINT('Ctrl Pts',(-1.73564626281591,-2.72325891450911,
-35.8664501191032));
#14207=CARTESIAN_POINT('Ctrl Pts',(-1.93682175994712,-2.57617831349985,
-35.8826250535428));
#14208=CARTESIAN_POINT('Ctrl Pts',(-1.97108524325117,-2.55005815578797,
-35.8853894518258));
#14209=CARTESIAN_POINT('Ctrl Pts',(-2.02324996571201,-2.50861145630289,
-35.8896004995417));
#14210=CARTESIAN_POINT('Ctrl Pts',(-2.04152314618931,-2.49376325965712,
-35.8910760734246));
#14211=CARTESIAN_POINT('Ctrl Pts',(-2.08054793985152,-2.46133648896671,
-35.8942253632126));
#14212=CARTESIAN_POINT('Ctrl Pts',(-2.10124322674253,-2.44369271025123,
-35.8958943009146));
#14213=CARTESIAN_POINT('Ctrl Pts',(-2.15850879656005,-2.39360543380923,
-35.9005170867573));
#14214=CARTESIAN_POINT('Ctrl Pts',(-2.19456919951827,-2.36058759056946,
-35.9034335846283));
#14215=CARTESIAN_POINT('Ctrl Pts',(-2.27783208525988,-2.28079204148107,
-35.9102197763547));
#14216=CARTESIAN_POINT('Ctrl Pts',(-2.32436735996572,-2.23334919300036,
-35.9140543068686));
#14217=CARTESIAN_POINT('Ctrl Pts',(-2.52351336619857,-2.0173466082862,-35.9308299985919));
#14218=CARTESIAN_POINT('Ctrl Pts',(-2.65950097101085,-1.83435707226531,
-35.9433333446844));
#14219=CARTESIAN_POINT('Ctrl Pts',(-2.82328562500885,-1.55697045956263,
-35.9618602949035));
#14220=CARTESIAN_POINT('Ctrl Pts',(-2.86784359159268,-1.4732853251386,-35.967393536816));
#14221=CARTESIAN_POINT('Ctrl Pts',(-2.93008660238295,-1.34282866866419,
-35.9760204010245));
#14222=CARTESIAN_POINT('Ctrl Pts',(-2.9504806285277,-1.29740509821388,-35.9790239820137));
#14223=CARTESIAN_POINT('Ctrl Pts',(-2.98692010291811,-1.21093612069053,
-35.9847513708787));
#14224=CARTESIAN_POINT('Ctrl Pts',(-3.00319191667718,-1.16999829316909,
-35.9874669183777));
#14225=CARTESIAN_POINT('Ctrl Pts',(-3.03913559849512,-1.07387327498605,
-35.9938581341467));
#14226=CARTESIAN_POINT('Ctrl Pts',(-3.05815131467147,-1.01845905122748,
-35.997553915797));
#14227=CARTESIAN_POINT('Ctrl Pts',(-3.13436292744262,-0.774941887613437,
-36.013854970905));
#14228=CARTESIAN_POINT('Ctrl Pts',(-3.17578194538343,-0.582370067358845,
-36.0269346893612));
#14229=CARTESIAN_POINT('Ctrl Pts',(-3.22113441339815,-0.207678306326374,
-36.0523363672066));
#14230=CARTESIAN_POINT('Ctrl Pts',(-3.22771416946683,-0.026581414062457,
-36.0645824543539));
#14231=CARTESIAN_POINT('Ctrl Pts',(-3.21711584209016,0.194783298034463,
-36.0789319368598));
#14232=CARTESIAN_POINT('Ctrl Pts',(-3.21439855691865,0.235408448348466,
-36.081538718959));
#14233=CARTESIAN_POINT('Ctrl Pts',(-3.20873265899732,0.301330420113932,
-36.0857141027372));
#14234=CARTESIAN_POINT('Ctrl Pts',(-3.20625283717842,0.326662229438198,
-36.087305308439));
#14235=CARTESIAN_POINT('Ctrl Pts',(-3.20031757435715,0.3806832538367,-36.0906672383803));
#14236=CARTESIAN_POINT('Ctrl Pts',(-3.19677600772745,0.409360001350443,
-36.0924335792214));
#14237=CARTESIAN_POINT('Ctrl Pts',(-3.18493514338627,0.49567796082553,-36.0977053171184));
#14238=CARTESIAN_POINT('Ctrl Pts',(-3.17545846841295,0.553148160072557,
-36.1011545492486));
#14239=CARTESIAN_POINT('Ctrl Pts',(-3.14809473551754,0.695022387610974,
-36.1095869599579));
#14240=CARTESIAN_POINT('Ctrl Pts',(-3.12836642481632,0.779026098282429,
-36.1145069189186));
#14241=CARTESIAN_POINT('Ctrl Pts',(-3.03705563323056,1.10791259091326,-36.1338134750345));
#14242=CARTESIAN_POINT('Ctrl Pts',(-2.93989136922043,1.34469707506539,-36.1478928416227));
#14243=CARTESIAN_POINT('Ctrl Pts',(-2.78610860079051,1.62094126662066,-36.1665050202827));
#14244=CARTESIAN_POINT('Ctrl Pts',(-2.75487467292528,1.6734743977719,-36.1701471075011));
#14245=CARTESIAN_POINT('Ctrl Pts',(-2.69842956222401,1.76254421451183,-36.1765225081536));
#14246=CARTESIAN_POINT('Ctrl Pts',(-2.67392169209843,1.79950734901087,-36.1792303670357));
#14247=CARTESIAN_POINT('Ctrl Pts',(-2.62096552875842,1.87590525363985,-36.1849655544831));
#14248=CARTESIAN_POINT('Ctrl Pts',(-2.59237201101042,1.91522525571623,-36.1879978097528));
#14249=CARTESIAN_POINT('Ctrl Pts',(-2.50993334790275,2.02335981279647,-36.1965722591115));
#14250=CARTESIAN_POINT('Ctrl Pts',(-2.45416635020851,2.09064958200223,-36.2021855155395));
#14251=CARTESIAN_POINT('Ctrl Pts',(-2.31444534459754,2.24593679900908,-36.2158229478985));
#14252=CARTESIAN_POINT('Ctrl Pts',(-2.22811187230057,2.33160949522023,-36.2239227649028));
#14253=CARTESIAN_POINT('Ctrl Pts',(-1.98469415084609,2.54727223292994,-36.2457756443501));
#14254=CARTESIAN_POINT('Ctrl Pts',(-1.81976548560901,2.66759617722323,-36.2596214630228));
#14255=CARTESIAN_POINT('Ctrl Pts',(-1.61153798554035,2.79115363381581,-36.2752587787306));
#14256=CARTESIAN_POINT('Ctrl Pts',(-1.57815156720587,2.81016569152845,-36.2777129437919));
#14257=CARTESIAN_POINT('Ctrl Pts',(-1.5221699285708,2.84073222909436,-36.2817311405092));
#14258=CARTESIAN_POINT('Ctrl Pts',(-1.49976472430271,2.85262455054892,-36.2833139129441));
#14259=CARTESIAN_POINT('Ctrl Pts',(-1.45054739343048,2.87800806875332,-36.2867334176054));
#14260=CARTESIAN_POINT('Ctrl Pts',(-1.42368340388327,2.89139134360469,-36.2885641342824));
#14261=CARTESIAN_POINT('Ctrl Pts',(-1.33801520572887,2.93258653390383,-36.2943019864602));
#14262=CARTESIAN_POINT('Ctrl Pts',(-1.278551101498,2.95899589389115,-36.2981372201688));
#14263=CARTESIAN_POINT('Ctrl Pts',(-1.12307554049099,3.02248308835779,-36.3078883725895));
#14264=CARTESIAN_POINT('Ctrl Pts',(-1.02601350786151,3.05679590004349,-36.3137125568083));
#14265=CARTESIAN_POINT('Ctrl Pts',(-0.708237972260232,3.15228809390823,
-36.3323998912176));
#14266=CARTESIAN_POINT('Ctrl Pts',(-0.482627985629584,3.19461776418244,
-36.3451421882252));
#14267=CARTESIAN_POINT('Ctrl Pts',(-0.193837355632865,3.21748982242873,
-36.3622013383093));
#14268=CARTESIAN_POINT('Ctrl Pts',(-0.133110872217195,3.22057362616077,
-36.3658257830755));
#14269=CARTESIAN_POINT('Ctrl Pts',(-0.0280403261118533,3.22293258004212,
-36.3721811356575));
#14270=CARTESIAN_POINT('Ctrl Pts',(0.0162695635558281,3.22301344731505,
-36.3748870676241));
#14271=CARTESIAN_POINT('Ctrl Pts',(0.109299029638245,3.22126482714555,-36.3806287578051));
#14272=CARTESIAN_POINT('Ctrl Pts',(0.158003353452588,3.21924337409048,-36.3836696682562));
#14273=CARTESIAN_POINT('Ctrl Pts',(0.294618091048819,3.2104656425767,-36.3923041652124));
#14274=CARTESIAN_POINT('Ctrl Pts',(0.382318988508141,3.20120592937546,-36.3979705006071));
#14275=CARTESIAN_POINT('Ctrl Pts',(0.591572778784733,3.17039084675088,-36.4117850715972));
#14276=CARTESIAN_POINT('Ctrl Pts',(0.712479943286171,3.14542599256789,-36.4200119174888));
#14277=CARTESIAN_POINT('Ctrl Pts',(1.02450433014471,3.06208337111606,-36.441720909037));
#14278=CARTESIAN_POINT('Ctrl Pts',(1.21216502597076,2.99276270421163,-36.4552801299156));
#14279=CARTESIAN_POINT('Ctrl Pts',(1.42726638373711,2.88972989686238,-36.4706915708696));
#14280=CARTESIAN_POINT('Ctrl Pts',(1.46201480193291,2.87230590845259,-36.4731757721629));
#14281=CARTESIAN_POINT('Ctrl Pts',(1.51895972856227,2.84245059308457,-36.4772277656719));
#14282=CARTESIAN_POINT('Ctrl Pts',(1.54133870739029,2.83037792334745,-36.4788149951191));
#14283=CARTESIAN_POINT('Ctrl Pts',(1.58962559705208,2.80358620626423,-36.4822260193326));
#14284=CARTESIAN_POINT('Ctrl Pts',(1.61547618744904,2.78877069542717,-36.4840441848412));
#14285=CARTESIAN_POINT('Ctrl Pts',(1.69591130173054,2.74117780055491,-36.4896881486924));
#14286=CARTESIAN_POINT('Ctrl Pts',(1.74973495249272,2.70713862986431,-36.4934453713537));
#14287=CARTESIAN_POINT('Ctrl Pts',(1.88486629158105,2.61596347736303,-36.5029198393972));
#14288=CARTESIAN_POINT('Ctrl Pts',(1.96460586562053,2.55662115101025,-36.5085517749056));
#14289=CARTESIAN_POINT('Ctrl Pts',(2.22479866420522,2.3436118923492,-36.5275029417947));
#14290=CARTESIAN_POINT('Ctrl Pts',(2.39099481993979,2.1737940910071,-36.5406669302415));
#14291=CARTESIAN_POINT('Ctrl Pts',(2.57394562628078,1.94023102217013,-36.5581552824553));
#14292=CARTESIAN_POINT('Ctrl Pts',(2.6094965878973,1.89214677089969,-36.5617229272965));
#14293=CARTESIAN_POINT('Ctrl Pts',(2.66895747794847,1.806858000927,-36.5680141628378));
#14294=CARTESIAN_POINT('Ctrl Pts',(2.69347782595103,1.77009795282878,-36.5707143100193));
#14295=CARTESIAN_POINT('Ctrl Pts',(2.74368098157445,1.69137563538036,-36.5764792659022));
#14296=CARTESIAN_POINT('Ctrl Pts',(2.76917404639804,1.6493063860622,-36.5795499883659));
#14297=CARTESIAN_POINT('Ctrl Pts',(2.83902330206339,1.52785197110619,-36.5883937027893));
#14298=CARTESIAN_POINT('Ctrl Pts',(2.88099351072359,1.44715544802375,-36.5942454597321));
#14299=CARTESIAN_POINT('Ctrl Pts',(2.97451804017407,1.24709347451989,-36.6086916588234));
#14300=CARTESIAN_POINT('Ctrl Pts',(3.02236999044531,1.1261770577313,-36.6173758456667));
#14301=CARTESIAN_POINT('Ctrl Pts',(3.12050857877369,0.826411934281973,-36.6385985929753));
#14302=CARTESIAN_POINT('Ctrl Pts',(3.16289990345324,0.645447927472846,-36.6511683208497));
#14303=CARTESIAN_POINT('Ctrl Pts',(3.19527156673198,0.42188450113924,-36.665789298792));
#14304=CARTESIAN_POINT('Ctrl Pts',(3.20030532758923,0.38182858154707,-36.6683731381609));
#14305=CARTESIAN_POINT('Ctrl Pts',(3.20727806948035,0.316433148956264,-36.6725223378304));
#14306=CARTESIAN_POINT('Ctrl Pts',(3.20967224437507,0.291147394506173,-36.6741097649234));
#14307=CARTESIAN_POINT('Ctrl Pts',(3.21416154468152,0.236908320488248,-36.6774757767755));
#14308=CARTESIAN_POINT('Ctrl Pts',(3.21616491157962,0.207950447403865,-36.6792497342344));
#14309=CARTESIAN_POINT('Ctrl Pts',(3.22105371632892,0.120051725813268,-36.6845748383974));
#14310=CARTESIAN_POINT('Ctrl Pts',(3.22271204948684,0.0610524349901548,
-36.6880681142143));
#14311=CARTESIAN_POINT('Ctrl Pts',(3.22280501060443,-0.0860024722208844,
-36.6966449989047));
#14312=CARTESIAN_POINT('Ctrl Pts',(3.21925300262627,-0.174012354868599,
-36.7016625240194));
#14313=CARTESIAN_POINT('Ctrl Pts',(3.19177948652545,-0.511131051920171,
-36.720782694854));
#14314=CARTESIAN_POINT('Ctrl Pts',(3.14249326600938,-0.757259053267211,
-36.7346073127618));
#14315=CARTESIAN_POINT('Ctrl Pts',(3.04611802014202,-1.05409483015323,-36.7529653371432));
#14316=CARTESIAN_POINT('Ctrl Pts',(3.02530655092486,-1.11241649105303,-36.756652989525));
#14317=CARTESIAN_POINT('Ctrl Pts',(2.98668945696848,-1.21151959429912,-36.7630803984826));
#14318=CARTESIAN_POINT('Ctrl Pts',(2.96969504595494,-1.25259916821432,-36.7657934563463));
#14319=CARTESIAN_POINT('Ctrl Pts',(2.93247480316839,-1.33755065939312,-36.7715131782093));
#14320=CARTESIAN_POINT('Ctrl Pts',(2.91210142483516,-1.38134540825479,-36.774524207285));
#14321=CARTESIAN_POINT('Ctrl Pts',(2.85298125850654,-1.50130475331785,-36.7829527395469));
#14322=CARTESIAN_POINT('Ctrl Pts',(2.81218007840505,-1.57640704471713,-36.7884372819794));
#14323=CARTESIAN_POINT('Ctrl Pts',(2.70844608590889,-1.75047838560856,-36.8016515477586));
#14324=CARTESIAN_POINT('Ctrl Pts',(2.64300243359661,-1.84780659276855,-36.8094500858079));
#14325=CARTESIAN_POINT('Ctrl Pts',(2.47958917365417,-2.06433946078963,-36.8276623645477));
#14326=CARTESIAN_POINT('Ctrl Pts',(2.37811192243085,-2.18045859068994,-36.8381031557792));
#14327=CARTESIAN_POINT('Ctrl Pts',(2.26877996761344,-2.28883267650913,-36.8483014782414));
#14328=CARTESIAN_POINT('Ctrl Pts',(2.26878021215176,-2.28883243411322,-37.0933419659928));
#14329=CARTESIAN_POINT('Ctrl Pts',(2.3293632006447,-2.22878020685655,-37.0876115240873));
#14330=CARTESIAN_POINT('Ctrl Pts',(2.38758199684161,-2.16630275406731,-37.0818495827687));
#14331=CARTESIAN_POINT('Ctrl Pts',(2.49946924069445,-2.03622041415379,-37.070319701331));
#14332=CARTESIAN_POINT('Ctrl Pts',(2.55301074649338,-1.96867407175026,-37.0645609767881));
#14333=CARTESIAN_POINT('Ctrl Pts',(2.6380727781611,-1.85204634736598,-37.055078673354));
#14334=CARTESIAN_POINT('Ctrl Pts',(2.67108499195885,-1.80410905988064,-37.0513032307019));
#14335=CARTESIAN_POINT('Ctrl Pts',(2.71851485329101,-1.73107736394836,-37.045759840595));
#14336=CARTESIAN_POINT('Ctrl Pts',(2.73392108909224,-1.70664216101776,-37.0439388447458));
#14337=CARTESIAN_POINT('Ctrl Pts',(2.76228110319835,-1.66029168255183,-37.0405523428823));
#14338=CARTESIAN_POINT('Ctrl Pts',(2.7753071965688,-1.6384246581854,-37.0389828798441));
#14339=CARTESIAN_POINT('Ctrl Pts',(2.8084966117567,-1.58117754786866,-37.0349416966247));
#14340=CARTESIAN_POINT('Ctrl Pts',(2.82825157760693,-1.54556430087423,-37.0324935120232));
#14341=CARTESIAN_POINT('Ctrl Pts',(2.93196347960186,-1.34994640937079,-37.0193482395171));
#14342=CARTESIAN_POINT('Ctrl Pts',(3.0030334547773,-1.18345625097854,-37.0092307604122));
#14343=CARTESIAN_POINT('Ctrl Pts',(3.12188889640058,-0.824051868495065,
-36.9879545046333));
#14344=CARTESIAN_POINT('Ctrl Pts',(3.16657046584812,-0.630930709019529,
-36.9768194958653));
#14345=CARTESIAN_POINT('Ctrl Pts',(3.20111379056032,-0.377319400385622,
-36.9617066486205));
#14346=CARTESIAN_POINT('Ctrl Pts',(3.20740073335664,-0.319498594491366,
-36.9582315643087));
#14347=CARTESIAN_POINT('Ctrl Pts',(3.21569091535942,-0.217682928409825,
-36.9520434981848));
#14348=CARTESIAN_POINT('Ctrl Pts',(3.21836325773751,-0.173757219754812,
-36.9493514970819));
#14349=CARTESIAN_POINT('Ctrl Pts',(3.22214940303129,-0.0798231851999515,
-36.9435409237611));
#14350=CARTESIAN_POINT('Ctrl Pts',(3.2230000094219,-0.0298164427737187,
-36.9404150710669));
#14351=CARTESIAN_POINT('Ctrl Pts',(3.22208389723299,0.11642774257034,-36.9311714818407));
#14352=CARTESIAN_POINT('Ctrl Pts',(3.21717037149344,0.212584052119634,-36.9249628364989));
#14353=CARTESIAN_POINT('Ctrl Pts',(3.18755941271854,0.520626446370249,-36.9046634560514));
#14354=CARTESIAN_POINT('Ctrl Pts',(3.14614052381762,0.73032374168661,-36.8901773842451));
#14355=CARTESIAN_POINT('Ctrl Pts',(3.06319476412836,1.00412545347833,-36.8710213754367));
#14356=CARTESIAN_POINT('Ctrl Pts',(3.03970119454276,1.07314854162765,-36.8661758613724));
#14357=CARTESIAN_POINT('Ctrl Pts',(2.99544007236552,1.19002911794051,-36.8580009986111));
#14358=CARTESIAN_POINT('Ctrl Pts',(2.97581472189264,1.23828830629115,-36.8546349451425));
#14359=CARTESIAN_POINT('Ctrl Pts',(2.94393564573099,1.31153840349947,-36.8495619178843));
#14360=CARTESIAN_POINT('Ctrl Pts',(2.93251463023895,1.33688000202048,-36.8478136508048));
#14361=CARTESIAN_POINT('Ctrl Pts',(2.90961938170543,1.38597556806677,-36.8444443942661));
#14362=CARTESIAN_POINT('Ctrl Pts',(2.8981787909384,1.40974216743345,-36.8428219287517));
#14363=CARTESIAN_POINT('Ctrl Pts',(2.86662730329719,1.47327911253003,-36.8385008068562));
#14364=CARTESIAN_POINT('Ctrl Pts',(2.84598035853446,1.51277878983917,-36.8358318021515));
#14365=CARTESIAN_POINT('Ctrl Pts',(2.72611603084671,1.73094512479043,-36.821118478065));
#14366=CARTESIAN_POINT('Ctrl Pts',(2.61088983290953,1.90030277117432,-36.8097815085896));
#14367=CARTESIAN_POINT('Ctrl Pts',(2.40738484442296,2.14562107373458,-36.7918369811821));
#14368=CARTESIAN_POINT('Ctrl Pts',(2.32975290967503,2.22967281374451,-36.7853644909927));
#14369=CARTESIAN_POINT('Ctrl Pts',(2.18752728874511,2.36810506254828,-36.7738822963538));
#14370=CARTESIAN_POINT('Ctrl Pts',(2.12496095515062,2.42440436570682,-36.7689430996895));
#14371=CARTESIAN_POINT('Ctrl Pts',(2.0232919774748,2.50892790000559,-36.7610287398567));
#14372=CARTESIAN_POINT('Ctrl Pts',(1.98563521641259,2.53883478281596,-36.7581201032712));
#14373=CARTESIAN_POINT('Ctrl Pts',(1.91183788837063,2.59479806362307,-36.7524540178461));
#14374=CARTESIAN_POINT('Ctrl Pts',(1.87579827453292,2.62096959724471,-36.7497018671816));
#14375=CARTESIAN_POINT('Ctrl Pts',(1.78789734481723,2.6820604679368,-36.7430189310875));
#14376=CARTESIAN_POINT('Ctrl Pts',(1.73554131265916,2.71623282913346,-36.739062102272));
#14377=CARTESIAN_POINT('Ctrl Pts',(1.55370611120304,2.82751104012485,-36.7253905954449));
#14378=CARTESIAN_POINT('Ctrl Pts',(1.41984161191822,2.89704364316559,-36.7154331439458));
#14379=CARTESIAN_POINT('Ctrl Pts',(1.09579421580223,3.03749411006707,-36.6917583912923));
#14380=CARTESIAN_POINT('Ctrl Pts',(0.902787712234111,3.1003410204323,-36.6779654776262));
#14381=CARTESIAN_POINT('Ctrl Pts',(0.657527378304204,3.15533798471728,-36.66156732129));
#14382=CARTESIAN_POINT('Ctrl Pts',(0.609660039406449,3.16493526701714,-36.6584203903634));
#14383=CARTESIAN_POINT('Ctrl Pts',(0.534825948879233,3.17817833683819,-36.6536017463083));
#14384=CARTESIAN_POINT('Ctrl Pts',(0.508001471684254,3.18257615153751,-36.6518945662789));
#14385=CARTESIAN_POINT('Ctrl Pts',(0.457833939013362,3.1901505317259,-36.6487431403305));
#14386=CARTESIAN_POINT('Ctrl Pts',(0.43450581242328,3.19341151400356,-36.6472943812467));
#14387=CARTESIAN_POINT('Ctrl Pts',(0.368360183675865,3.20191958326549,-36.6432283770199));
#14388=CARTESIAN_POINT('Ctrl Pts',(0.325468588981579,3.20656339930327,-36.6406413189473));
#14389=CARTESIAN_POINT('Ctrl Pts',(0.0772558646317259,3.22840489205267,
-36.6258899543271));
#14390=CARTESIAN_POINT('Ctrl Pts',(-0.129262899783675,3.22674375193573,
-36.614459744368));
#14391=CARTESIAN_POINT('Ctrl Pts',(-0.448489763055395,3.19345779336678,
-36.5963920988824));
#14392=CARTESIAN_POINT('Ctrl Pts',(-0.562029973236523,3.17544263665794,
-36.5898904051983));
#14393=CARTESIAN_POINT('Ctrl Pts',(-0.756880953879801,3.1337469797369,-36.5783642992438));
#14394=CARTESIAN_POINT('Ctrl Pts',(-0.838670004772175,3.11285558371548,
-36.5734112518962));
#14395=CARTESIAN_POINT('Ctrl Pts',(-0.965663684523506,3.07504911826834,
-36.5654803458133));
#14396=CARTESIAN_POINT('Ctrl Pts',(-1.01147136058358,3.06028736409196,-36.5625695300077));
#14397=CARTESIAN_POINT('Ctrl Pts',(-1.098985711136,3.02990591429566,-36.5569025203809));
#14398=CARTESIAN_POINT('Ctrl Pts',(-1.14073303816111,3.01443647682831,-36.5541517019343));
#14399=CARTESIAN_POINT('Ctrl Pts',(-1.24018606445976,2.97522244460751,-36.5474779805147));
#14400=CARTESIAN_POINT('Ctrl Pts',(-1.29754694079023,2.95065775230396,-36.5435292174281));
#14401=CARTESIAN_POINT('Ctrl Pts',(-1.54863581723115,2.83439177346074,-36.5257861834419));
#14402=CARTESIAN_POINT('Ctrl Pts',(-1.733622720393,2.72517481304542,-36.511430163473));
#14403=CARTESIAN_POINT('Ctrl Pts',(-1.99502983227976,2.53338968175026,-36.4895926955401));
#14404=CARTESIAN_POINT('Ctrl Pts',(-2.08029953091262,2.46385125852985,-36.4821913202758));
#14405=CARTESIAN_POINT('Ctrl Pts',(-2.21204941030082,2.34468260880668,-36.470457319682));
#14406=CARTESIAN_POINT('Ctrl Pts',(-2.2608090660935,2.29770380726449,-36.4660423163337));
#14407=CARTESIAN_POINT('Ctrl Pts',(-2.32928382990072,2.22743788388161,-36.4597780894231));
#14408=CARTESIAN_POINT('Ctrl Pts',(-2.35020314631228,2.2053543973062,-36.4578551799428));
#14409=CARTESIAN_POINT('Ctrl Pts',(-2.38792184549556,2.16439025886892,-36.4543764471158));
#14410=CARTESIAN_POINT('Ctrl Pts',(-2.40481591436229,2.1456039686541,-36.4528144856812));
#14411=CARTESIAN_POINT('Ctrl Pts',(-2.44632368301413,2.09834087570868,-36.4489635681865));
#14412=CARTESIAN_POINT('Ctrl Pts',(-2.47066243935511,2.06962831888913,-36.4466929738892));
#14413=CARTESIAN_POINT('Ctrl Pts',(-2.62789688096676,1.87741005359106,-36.4318900954008));
#14414=CARTESIAN_POINT('Ctrl Pts',(-2.74500115013186,1.70161684466447,-36.4201896049185));
#14415=CARTESIAN_POINT('Ctrl Pts',(-2.89981434048922,1.41110681433615,-36.4016689136764));
#14416=CARTESIAN_POINT('Ctrl Pts',(-2.94970902206995,1.30359508714166,-36.3949755180019));
#14417=CARTESIAN_POINT('Ctrl Pts',(-3.02542151465806,1.11370449768179,-36.3831618702812));
#14418=CARTESIAN_POINT('Ctrl Pts',(-3.05405935049314,1.0325854935536,-36.3781187150349));
#14419=CARTESIAN_POINT('Ctrl Pts',(-3.09368826396924,0.904185818639147,
-36.3700795738229));
#14420=CARTESIAN_POINT('Ctrl Pts',(-3.1069149443198,0.857635251862282,-36.3671540043573));
#14421=CARTESIAN_POINT('Ctrl Pts',(-3.13026387493227,0.76781433008927,-36.3614789016122));
#14422=CARTESIAN_POINT('Ctrl Pts',(-3.14054911583673,0.724597626116939,
-36.3587352283597));
#14423=CARTESIAN_POINT('Ctrl Pts',(-3.1629732805215,0.620903553731744,-36.3521151103149));
#14424=CARTESIAN_POINT('Ctrl Pts',(-3.1742752650122,0.560265054473821,-36.3482139011018));
#14425=CARTESIAN_POINT('Ctrl Pts',(-3.21812448121106,0.280680609944262,
-36.33007897963));
#14426=CARTESIAN_POINT('Ctrl Pts',(-3.22979689244493,0.0590957213635396,
-36.3152368439635));
#14427=CARTESIAN_POINT('Ctrl Pts',(-3.21333312897307,-0.268214814711256,
-36.2931647987562));
#14428=CARTESIAN_POINT('Ctrl Pts',(-3.20272109471427,-0.374203673708924,
-36.2860055246003));
#14429=CARTESIAN_POINT('Ctrl Pts',(-3.17700427150586,-0.545132774536986,
-36.2745961397821));
#14430=CARTESIAN_POINT('Ctrl Pts',(-3.16509874051347,-0.610472828562163,
-36.2702683406673));
#14431=CARTESIAN_POINT('Ctrl Pts',(-3.14484894598609,-0.704950980272161,
-36.2641013987289));
#14432=CARTESIAN_POINT('Ctrl Pts',(-3.13810018109963,-0.734410095383784,
-36.2621915473615));
#14433=CARTESIAN_POINT('Ctrl Pts',(-3.12493895610913,-0.788362088487279,
-36.2587232018279));
#14434=CARTESIAN_POINT('Ctrl Pts',(-3.1186510706632,-0.812879940919055,
-36.2571589035257));
#14435=CARTESIAN_POINT('Ctrl Pts',(-3.10220023504282,-0.874022652333175,
-36.2532838048014));
#14436=CARTESIAN_POINT('Ctrl Pts',(-3.09167719487609,-0.910546154656176,
-36.2509919509918));
#14437=CARTESIAN_POINT('Ctrl Pts',(-3.01957730679511,-1.1451114648457,-36.2363716006436));
#14438=CARTESIAN_POINT('Ctrl Pts',(-2.93964476949381,-1.33702496849744,
-36.2248442199179));
#14439=CARTESIAN_POINT('Ctrl Pts',(-2.78526891677148,-1.62565927197093,
-36.2064316310738));
#14440=CARTESIAN_POINT('Ctrl Pts',(-2.72287280848679,-1.7281355464251,-36.1996601759258));
#14441=CARTESIAN_POINT('Ctrl Pts',(-2.60580124597897,-1.898268718711,-36.1877300085402));
#14442=CARTESIAN_POINT('Ctrl Pts',(-2.55383160173638,-1.96762970265087,
-36.1826507867877));
#14443=CARTESIAN_POINT('Ctrl Pts',(-2.46851431462195,-2.07241560396686,
-36.174568300428));
#14444=CARTESIAN_POINT('Ctrl Pts',(-2.43705128269534,-2.10932454297226,
-36.1716368206507));
#14445=CARTESIAN_POINT('Ctrl Pts',(-2.37521939414734,-2.17862811997138,
-36.1659582170153));
#14446=CARTESIAN_POINT('Ctrl Pts',(-2.34499025547948,-2.21113275370532,
-36.1632171424686));
#14447=CARTESIAN_POINT('Ctrl Pts',(-2.27136394556417,-2.28709288345824,
-36.1566171003333));
#14448=CARTESIAN_POINT('Ctrl Pts',(-2.22737834136518,-2.32995127812476,
-36.1527337795605));
#14449=CARTESIAN_POINT('Ctrl Pts',(-2.01753986888988,-2.52303759016171,
-36.1344654577454));
#14450=CARTESIAN_POINT('Ctrl Pts',(-1.83757175526662,-2.65696979043442,
-36.1194553422679));
#14451=CARTESIAN_POINT('Ctrl Pts',(-1.5546848266988,-2.82491735448134,-36.097299387746));
#14452=CARTESIAN_POINT('Ctrl Pts',(-1.46156738123851,-2.87419998621752,
-36.0902203807229));
#14453=CARTESIAN_POINT('Ctrl Pts',(-1.30646206170698,-2.94679912206043,
-36.078919129597));
#14454=CARTESIAN_POINT('Ctrl Pts',(-1.24587425542452,-2.97292225469375,
-36.0746207415771));
#14455=CARTESIAN_POINT('Ctrl Pts',(-1.15648138123724,-3.00825157800046,
-36.0684866633764));
#14456=CARTESIAN_POINT('Ctrl Pts',(-1.12828397849175,-3.01894056944114,
-36.0665812584264));
#14457=CARTESIAN_POINT('Ctrl Pts',(-1.07613164413316,-3.03787751489069,
-36.0631163856028));
#14458=CARTESIAN_POINT('Ctrl Pts',(-1.05222419946695,-3.0462408606694,-36.0615512279953));
#14459=CARTESIAN_POINT('Ctrl Pts',(-0.992076986397332,-3.06648904320856,
-36.0576675683651));
#14460=CARTESIAN_POINT('Ctrl Pts',(-0.955720632842481,-3.07801399534661,
-36.0553682195607));
#14461=CARTESIAN_POINT('Ctrl Pts',(-0.721519958336437,-3.14770547721308,
-36.0408127560886));
#14462=CARTESIAN_POINT('Ctrl Pts',(-0.518661636472471,-3.18742064519333,
-36.029347028721));
#14463=CARTESIAN_POINT('Ctrl Pts',(-0.193542023589923,-3.21918582058902,
-36.010972564263));
#14464=CARTESIAN_POINT('Ctrl Pts',(-0.073146526034735,-3.22416861074646,
-36.0041731332972));
#14465=CARTESIAN_POINT('Ctrl Pts',(0.134101229839968,-3.22113037301194,
-35.9922013000168));
#14466=CARTESIAN_POINT('Ctrl Pts',(0.220869375881308,-3.21634559109624,
-35.9871092559391));
#14467=CARTESIAN_POINT('Ctrl Pts',(0.355645001954417,-3.20343403313489,
-35.9790113854823));
#14468=CARTESIAN_POINT('Ctrl Pts',(0.403843594446042,-3.1977152699262,-35.9760778345149));
#14469=CARTESIAN_POINT('Ctrl Pts',(0.495827415973493,-3.18468863401984,
-35.9703980338708));
#14470=CARTESIAN_POINT('Ctrl Pts',(0.539627004562982,-3.17756021432315,
-35.9676579005885));
#14471=CARTESIAN_POINT('Ctrl Pts',(0.643560070621952,-3.15843422448798,
-35.9610649905727));
#14472=CARTESIAN_POINT('Ctrl Pts',(0.70352393929789,-3.14562070005593,-35.9571880051658));
#14473=CARTESIAN_POINT('Ctrl Pts',(1.00974351257171,-3.07099181385787,-35.9369979642906));
#14474=CARTESIAN_POINT('Ctrl Pts',(1.24840617831193,-2.98194843288396,-35.919848896879));
#14475=CARTESIAN_POINT('Ctrl Pts',(1.55119609875955,-2.82620307115287,-35.8969661843085));
#14476=CARTESIAN_POINT('Ctrl Pts',(1.62666041847073,-2.78345297153647,-35.8911704167628));
#14477=CARTESIAN_POINT('Ctrl Pts',(1.74994341087111,-2.70688548565644,-35.8816360030103));
#14478=CARTESIAN_POINT('Ctrl Pts',(1.79873059856379,-2.67471495584634,-35.8778448521494));
#14479=CARTESIAN_POINT('Ctrl Pts',(1.87032490588861,-2.6246597819614,-35.8722834962769));
#14480=CARTESIAN_POINT('Ctrl Pts',(1.89380754044571,-2.60776673889777,-35.8704597744819));
#14481=CARTESIAN_POINT('Ctrl Pts',(1.9375086163502,-2.57542715407489,-35.8670713503549));
#14482=CARTESIAN_POINT('Ctrl Pts',(1.95777682129483,-2.5600536349338,-35.8655026220409));
#14483=CARTESIAN_POINT('Ctrl Pts',(2.00993409369761,-2.5195104111105,-35.8614679039294));
#14484=CARTESIAN_POINT('Ctrl Pts',(2.04153418781651,-2.49397399119942,-35.8590252877775));
#14485=CARTESIAN_POINT('Ctrl Pts',(2.1404817407716,-2.41087191038697,-35.8513527509625));
#14486=CARTESIAN_POINT('Ctrl Pts',(2.20591396337446,-2.35114792362527,-35.8462418756784));
#14487=CARTESIAN_POINT('Ctrl Pts',(2.26878031087686,-2.28883233625302,-35.8411988517434));
#14488=CARTESIAN_POINT('Origin',(0.,0.,-41.3107734492731));
#14489=CARTESIAN_POINT('',(2.26878010865581,-2.28883253670244,-34.3485046109761));
#14490=CARTESIAN_POINT('',(2.26878020184338,-2.28883244433128,-34.5957191253299));
#14491=CARTESIAN_POINT('',(2.26878020078428,-2.2888324453811,-41.3107734492731));
#14492=CARTESIAN_POINT('Ctrl Pts',(2.2687801086558,-2.28883253670245,-34.3485046109761));
#14493=CARTESIAN_POINT('Ctrl Pts',(2.15700584426002,-2.39962754841884,-34.3575848935098));
#14494=CARTESIAN_POINT('Ctrl Pts',(2.03721275441062,-2.50213866773743,-34.366358323638));
#14495=CARTESIAN_POINT('Ctrl Pts',(1.81827356931631,-2.66328125615279,-34.3816629304255));
#14496=CARTESIAN_POINT('Ctrl Pts',(1.72266971123268,-2.7260947863319,-34.3881340470896));
#14497=CARTESIAN_POINT('Ctrl Pts',(1.5512683466518,-2.82608592203579,-34.3996141200708));
#14498=CARTESIAN_POINT('Ctrl Pts',(1.47697419281886,-2.86561349792613,-34.4045526052959));
#14499=CARTESIAN_POINT('Ctrl Pts',(1.35792484610279,-2.92309243929206,-34.4124660255598));
#14500=CARTESIAN_POINT('Ctrl Pts',(1.31416629502935,-2.94302495384176,-34.4153744560725));
#14501=CARTESIAN_POINT('Ctrl Pts',(1.22904826684484,-2.97952031683764,-34.4210402393136));
#14502=CARTESIAN_POINT('Ctrl Pts',(1.18775893223603,-2.99621917983728,-34.4237922965348));
#14503=CARTESIAN_POINT('Ctrl Pts',(1.08771353214931,-3.03428814414662,-34.430475145985));
#14504=CARTESIAN_POINT('Ctrl Pts',(1.02865763813113,-3.05481388859171,-34.4344319849203));
#14505=CARTESIAN_POINT('Ctrl Pts',(0.825336125197219,-3.11891696388786,
-34.4481038307153));
#14506=CARTESIAN_POINT('Ctrl Pts',(0.678642483971953,-3.15408589545084,
-34.4580616438956));
#14507=CARTESIAN_POINT('Ctrl Pts',(0.330259734717609,-3.21217510004361,
-34.4817377001873));
#14508=CARTESIAN_POINT('Ctrl Pts',(0.12777831773368,-3.22657988157259,-34.495531584636));
#14509=CARTESIAN_POINT('Ctrl Pts',(-0.123517059971134,-3.22075201923825,
-34.5119305997965));
#14510=CARTESIAN_POINT('Ctrl Pts',(-0.172285430652327,-3.21851181774909,
-34.515077531067));
#14511=CARTESIAN_POINT('Ctrl Pts',(-0.248102191478151,-3.21330073025679,
-34.519896112185));
#14512=CARTESIAN_POINT('Ctrl Pts',(-0.275194031599388,-3.21109399499259,
-34.5216032320977));
#14513=CARTESIAN_POINT('Ctrl Pts',(-0.325704457999064,-3.20633574169521,
-34.5247545381566));
#14514=CARTESIAN_POINT('Ctrl Pts',(-0.349128932961697,-3.20386974433673,
-34.5262032379756));
#14515=CARTESIAN_POINT('Ctrl Pts',(-0.4153669684613,-3.19616146903437,-34.5302689168139));
#14516=CARTESIAN_POINT('Ctrl Pts',(-0.458106839413337,-3.19031603007539,
-34.5328557156488));
#14517=CARTESIAN_POINT('Ctrl Pts',(-0.704254303229759,-3.1516019675485,
-34.5476072367903));
#14518=CARTESIAN_POINT('Ctrl Pts',(-0.904272043636709,-3.10014171965664,
-34.5590377638131));
#14519=CARTESIAN_POINT('Ctrl Pts',(-1.20603458439057,-2.99078534656033,
-34.5771058785864));
#14520=CARTESIAN_POINT('Ctrl Pts',(-1.31187208619722,-2.9458964546036,-34.583607721888));
#14521=CARTESIAN_POINT('Ctrl Pts',(-1.49090168313425,-2.85840013740546,
-34.5951340674383));
#14522=CARTESIAN_POINT('Ctrl Pts',(-1.56523120276755,-2.81838407721604,
-34.6000872000718));
#14523=CARTESIAN_POINT('Ctrl Pts',(-1.67934619186124,-2.75104159134923,
-34.6080182162998));
#14524=CARTESIAN_POINT('Ctrl Pts',(-1.72023668208287,-2.72565934404721,
-34.6109290538131));
#14525=CARTESIAN_POINT('Ctrl Pts',(-1.79783058004558,-2.67505227210551,
-34.6165960907502));
#14526=CARTESIAN_POINT('Ctrl Pts',(-1.83460971359678,-2.64996346130282,
-34.6193469144118));
#14527=CARTESIAN_POINT('Ctrl Pts',(-1.92165686580859,-2.58790358006154,
-34.6260206282659));
#14528=CARTESIAN_POINT('Ctrl Pts',(-1.97139231540311,-2.55021990303089,
-34.6299693779722));
#14529=CARTESIAN_POINT('Ctrl Pts',(-2.13530465371551,-2.41836512718779,
-34.643458630102));
#14530=CARTESIAN_POINT('Ctrl Pts',(-2.24407082621219,-2.31779057106791,
-34.6532315648553));
#14531=CARTESIAN_POINT('Ctrl Pts',(-2.43666998029154,-2.1133901351265,-34.6720491091999));
#14532=CARTESIAN_POINT('Ctrl Pts',(-2.52173594617269,-2.01112554606369,
-34.6810464597918));
#14533=CARTESIAN_POINT('Ctrl Pts',(-2.64139660869419,-1.84769956315272,
-34.6945927172459));
#14534=CARTESIAN_POINT('Ctrl Pts',(-2.68071723906216,-1.79017478774294,
-34.6992163509935));
#14535=CARTESIAN_POINT('Ctrl Pts',(-2.7452771635445,-1.6888225015762,-34.7070668152836));
#14536=CARTESIAN_POINT('Ctrl Pts',(-2.7714066487484,-1.64559227716962,-34.7103269275318));
#14537=CARTESIAN_POINT('Ctrl Pts',(-2.8101787528156,-1.57790025045115,-34.7152772125008));
#14538=CARTESIAN_POINT('Ctrl Pts',(-2.82354139393212,-1.55386226634818,
-34.717005819691));
#14539=CARTESIAN_POINT('Ctrl Pts',(-2.84768639832253,-1.50908772944498,
-34.7201677771165));
#14540=CARTESIAN_POINT('Ctrl Pts',(-2.85855379229225,-1.4883997667111,-34.7216061730157));
#14541=CARTESIAN_POINT('Ctrl Pts',(-2.888308160447,-1.43022901639573,-34.7255929003826));
#14542=CARTESIAN_POINT('Ctrl Pts',(-2.90669009308099,-1.39249134217169,
-34.7281130055937));
#14543=CARTESIAN_POINT('Ctrl Pts',(-2.9834843888935,-1.22668262085376,-34.7389454743223));
#14544=CARTESIAN_POINT('Ctrl Pts',(-3.03421295903237,-1.09521150202432,
-34.7469241659683));
#14545=CARTESIAN_POINT('Ctrl Pts',(-3.12276655164491,-0.811700281835316,
-34.7636518480597));
#14546=CARTESIAN_POINT('Ctrl Pts',(-3.15844057919212,-0.659378186072398,
-34.7723718958333));
#14547=CARTESIAN_POINT('Ctrl Pts',(-3.19871767776629,-0.405556570087333,
-34.7871099169284));
#14548=CARTESIAN_POINT('Ctrl Pts',(-3.20983238129255,-0.305359483045984,
-34.792976886234));
#14549=CARTESIAN_POINT('Ctrl Pts',(-3.21945636374139,-0.154230778247315,
-34.8020023677299));
#14550=CARTESIAN_POINT('Ctrl Pts',(-3.22148360358471,-0.103582721474755,
-34.8050561936212));
#14551=CARTESIAN_POINT('Ctrl Pts',(-3.22303646590291,-0.00901041361086034,
-34.8108234095914));
#14552=CARTESIAN_POINT('Ctrl Pts',(-3.22286008437264,0.0348974613347764,
-34.8135270896846));
#14553=CARTESIAN_POINT('Ctrl Pts',(-3.22041634235099,0.134828572752071,
-34.8197455264607));
#14554=CARTESIAN_POINT('Ctrl Pts',(-3.21758392805247,0.190822478239483,
-34.8232765832901));
#14555=CARTESIAN_POINT('Ctrl Pts',(-3.20105477719983,0.406106380548137,
-34.8370420230614));
#14556=CARTESIAN_POINT('Ctrl Pts',(-3.17697527065622,0.564349734224334,
-34.8475757196387));
#14557=CARTESIAN_POINT('Ctrl Pts',(-3.10587378834236,0.874497057878567,
-34.8688880136112));
#14558=CARTESIAN_POINT('Ctrl Pts',(-3.05915714949187,1.02603839900073,-34.8796332095907));
#14559=CARTESIAN_POINT('Ctrl Pts',(-2.97147372618767,1.25030245186017,-34.8956434110911));
#14560=CARTESIAN_POINT('Ctrl Pts',(-2.93852073077748,1.32589982133244,-34.9010572132222));
#14561=CARTESIAN_POINT('Ctrl Pts',(-2.88862319236059,1.42934383474286,-34.9084147909857));
#14562=CARTESIAN_POINT('Ctrl Pts',(-2.87410375741152,1.45831941836085,-34.9104699256199));
#14563=CARTESIAN_POINT('Ctrl Pts',(-2.84761106202955,1.5092561243403,-34.914066056812));
#14564=CARTESIAN_POINT('Ctrl Pts',(-2.83581575709415,1.53130397909653,-34.9156164591919));
#14565=CARTESIAN_POINT('Ctrl Pts',(-2.8070517461125,1.58359731731963,-34.9192804387879));
#14566=CARTESIAN_POINT('Ctrl Pts',(-2.78984961915996,1.61370979201426,-34.9213803325797));
#14567=CARTESIAN_POINT('Ctrl Pts',(-2.72087174896168,1.73005497251443,-34.9294774931738));
#14568=CARTESIAN_POINT('Ctrl Pts',(-2.66555301386505,1.81412895273838,-34.9352943191486));
#14569=CARTESIAN_POINT('Ctrl Pts',(-2.51775092655695,2.01736441106725,-34.949613897843));
#14570=CARTESIAN_POINT('Ctrl Pts',(-2.42067258631048,2.13287955687515,-34.9579993181559));
#14571=CARTESIAN_POINT('Ctrl Pts',(-2.24644231211711,2.31291595012444,-34.9721556750646));
#14572=CARTESIAN_POINT('Ctrl Pts',(-2.17372684684648,2.38138470599216,-34.9778435854657));
#14573=CARTESIAN_POINT('Ctrl Pts',(-2.03941000172662,2.49657216369485,-34.9881263006929));
#14574=CARTESIAN_POINT('Ctrl Pts',(-1.97908574658288,2.5446579390078,-34.9926716634702));
#14575=CARTESIAN_POINT('Ctrl Pts',(-1.87939851657902,2.61843052029085,-35.0001129422563));
#14576=CARTESIAN_POINT('Ctrl Pts',(-1.84109610222593,2.64550221572821,-35.0029561941834));
#14577=CARTESIAN_POINT('Ctrl Pts',(-1.7648061163322,2.69696374746712,-35.0085967852438));
#14578=CARTESIAN_POINT('Ctrl Pts',(-1.7268698184464,2.72141036864695,-35.0113911636954));
#14579=CARTESIAN_POINT('Ctrl Pts',(-1.63180585265499,2.77988258618225,-35.0183738222498));
#14580=CARTESIAN_POINT('Ctrl Pts',(-1.57411681069742,2.81295090543525,-35.0225944000651));
#14581=CARTESIAN_POINT('Ctrl Pts',(-1.44470459437286,2.88190421653859,-35.032031106279));
#14582=CARTESIAN_POINT('Ctrl Pts',(-1.3725824014475,2.91694348879139,-35.0372703484799));
#14583=CARTESIAN_POINT('Ctrl Pts',(-1.10965187998685,3.03277204486511,-35.0562726155883));
#14584=CARTESIAN_POINT('Ctrl Pts',(-0.912461961896676,3.09781191070751,
-35.0703807730241));
#14585=CARTESIAN_POINT('Ctrl Pts',(-0.625475374497176,3.16266997724789,
-35.0899860035357));
#14586=CARTESIAN_POINT('Ctrl Pts',(-0.539785471905421,3.1784170313087,-35.0957207452498));
#14587=CARTESIAN_POINT('Ctrl Pts',(-0.420552224945453,3.19536613024062,
-35.1034509951651));
#14588=CARTESIAN_POINT('Ctrl Pts',(-0.387475243087062,3.19954559569184,
-35.1055691057823));
#14589=CARTESIAN_POINT('Ctrl Pts',(-0.329509648010112,3.20595772580962,
-35.1092281946368));
#14590=CARTESIAN_POINT('Ctrl Pts',(-0.304650750548156,3.20841543033335,
-35.1107800447365));
#14591=CARTESIAN_POINT('Ctrl Pts',(-0.246841077342685,3.21345283830605,
-35.1143488701027));
#14592=CARTESIAN_POINT('Ctrl Pts',(-0.213875251475101,3.21581517404566,
-35.1163547588733));
#14593=CARTESIAN_POINT('Ctrl Pts',(-0.0930033442108636,3.22260984352113,
-35.123621325248));
#14594=CARTESIAN_POINT('Ctrl Pts',(-0.00495643619134498,3.22394816095712,
-35.128744378643));
#14595=CARTESIAN_POINT('Ctrl Pts',(0.265484150667288,3.21697734410398,-35.1442463003433));
#14596=CARTESIAN_POINT('Ctrl Pts',(0.447202374201056,3.19678583647782,-35.1543518866553));
#14597=CARTESIAN_POINT('Ctrl Pts',(0.75478555717288,3.13585536735573,-35.1721210086342));
#14598=CARTESIAN_POINT('Ctrl Pts',(0.881647955232236,3.1025767235475,-35.1796485045852));
#14599=CARTESIAN_POINT('Ctrl Pts',(1.05906921337028,3.04427261081192,-35.1907054745601));
#14600=CARTESIAN_POINT('Ctrl Pts',(1.11155041612107,3.02550466091211,-35.1940435891295));
#14601=CARTESIAN_POINT('Ctrl Pts',(1.20437532491047,2.98956807952176,-35.2000842424896));
#14602=CARTESIAN_POINT('Ctrl Pts',(1.24490572054345,2.97291888296745,-35.2027694218143));
#14603=CARTESIAN_POINT('Ctrl Pts',(1.33237515967555,2.93488559233414,-35.2086748778193));
#14604=CARTESIAN_POINT('Ctrl Pts',(1.37916498930865,2.91319076984041,-35.2119048792196));
#14605=CARTESIAN_POINT('Ctrl Pts',(1.52143860638185,2.84302757691006,-35.2219545429626));
#14606=CARTESIAN_POINT('Ctrl Pts',(1.61503634061994,2.79092009456253,-35.2288921709981));
#14607=CARTESIAN_POINT('Ctrl Pts',(1.85550250735081,2.6408969571709,-35.2475774212668));
#14608=CARTESIAN_POINT('Ctrl Pts',(1.99722069913298,2.53541483346839,-35.2595141716288));
#14609=CARTESIAN_POINT('Ctrl Pts',(2.22194170354755,2.33756994612819,-35.2796272495667));
#14610=CARTESIAN_POINT('Ctrl Pts',(2.30957218088143,2.25103079011394,-35.287827185852));
#14611=CARTESIAN_POINT('Ctrl Pts',(2.41634378832392,2.13277168207641,-35.2980900640551));
#14612=CARTESIAN_POINT('Ctrl Pts',(2.44018823150816,2.10544864589801,-35.3004010430417));
#14613=CARTESIAN_POINT('Ctrl Pts',(2.47976067797567,2.05852748541694,-35.3042608866362));
#14614=CARTESIAN_POINT('Ctrl Pts',(2.49572904666603,2.0391383222866,-35.3058251761443));
#14615=CARTESIAN_POINT('Ctrl Pts',(2.53104779020776,1.99521693535195,-35.309299240326));
#14616=CARTESIAN_POINT('Ctrl Pts',(2.5502707586273,1.97058690795218,-35.3112008888017));
#14617=CARTESIAN_POINT('Ctrl Pts',(2.61344449778358,1.88717044498049,-35.3175017999067));
#14618=CARTESIAN_POINT('Ctrl Pts',(2.65574726692722,1.8271596682661,-35.3218075352602));
#14619=CARTESIAN_POINT('Ctrl Pts',(2.76536485063017,1.65979456666491,-35.3333614219237));
#14620=CARTESIAN_POINT('Ctrl Pts',(2.82845962271793,1.54983226508888,-35.3404704309024));
#14621=CARTESIAN_POINT('Ctrl Pts',(2.96805273031486,1.26947536284365,-35.3580731674177));
#14622=CARTESIAN_POINT('Ctrl Pts',(3.03652744225533,1.09562680945297,-35.368562364152));
#14623=CARTESIAN_POINT('Ctrl Pts',(3.10771481836829,0.855738501234879,-35.3832566992314));
#14624=CARTESIAN_POINT('Ctrl Pts',(3.12402939344504,0.794115443589744,-35.3870472893939));
#14625=CARTESIAN_POINT('Ctrl Pts',(3.14866151122781,0.688510875674616,-35.393593406024));
#14626=CARTESIAN_POINT('Ctrl Pts',(3.1579098371248,0.644764838406605,-35.3963193841941));
#14627=CARTESIAN_POINT('Ctrl Pts',(3.17513239046499,0.554007524635492,-35.4020108906884));
#14628=CARTESIAN_POINT('Ctrl Pts',(3.18297931941968,0.506983539569178,-35.404979616173));
#14629=CARTESIAN_POINT('Ctrl Pts',(3.20143322228754,0.378964200486526,-35.4131216186116));
#14630=CARTESIAN_POINT('Ctrl Pts',(3.21000808518044,0.297716010688075,-35.4183543283446));
#14631=CARTESIAN_POINT('Ctrl Pts',(3.22280641341184,0.107400609165122,-35.4307647231612));
#14632=CARTESIAN_POINT('Ctrl Pts',(3.22459453473107,-0.00172737352979303,
-35.4379992562718));
#14633=CARTESIAN_POINT('Ctrl Pts',(3.21320166933526,-0.333119993313931,
-35.4602137468149));
#14634=CARTESIAN_POINT('Ctrl Pts',(3.18254381919031,-0.554126004956237,
-35.4754021874223));
#14635=CARTESIAN_POINT('Ctrl Pts',(3.11978679271869,-0.809105689326679,
-35.4923923928286));
#14636=CARTESIAN_POINT('Ctrl Pts',(3.10949022012298,-0.847816342486037,
-35.4949553300529));
#14637=CARTESIAN_POINT('Ctrl Pts',(3.09150279239003,-0.910697859025966,
-35.4990807293006));
#14638=CARTESIAN_POINT('Ctrl Pts',(3.08424378365282,-0.934986928939391,
-35.5006647696574));
#14639=CARTESIAN_POINT('Ctrl Pts',(3.06802235357057,-0.98701880831585,-35.5040348461883));
#14640=CARTESIAN_POINT('Ctrl Pts',(3.05896885323836,-1.01473000639363,-35.5058160261602));
#14641=CARTESIAN_POINT('Ctrl Pts',(3.03021604938352,-1.09885311185906,-35.5111920557482));
#14642=CARTESIAN_POINT('Ctrl Pts',(3.00932205699648,-1.15484594100018,-35.5147273853425));
#14643=CARTESIAN_POINT('Ctrl Pts',(2.95316984913018,-1.29343131086734,-35.5234435463508));
#14644=CARTESIAN_POINT('Ctrl Pts',(2.91599410384748,-1.37519336744652,-35.528555473604));
#14645=CARTESIAN_POINT('Ctrl Pts',(2.76456548512911,-1.67439319643931,-35.5475013444154));
#14646=CARTESIAN_POINT('Ctrl Pts',(2.629012717813,-1.88007998604159,-35.5610835686793));
#14647=CARTESIAN_POINT('Ctrl Pts',(2.43119495573586,-2.11644447820218,-35.5792010272464));
#14648=CARTESIAN_POINT('Ctrl Pts',(2.38957608063778,-2.16332418873763,-35.5829318836063));
#14649=CARTESIAN_POINT('Ctrl Pts',(2.32113404127666,-2.23603147064495,-35.588963307873));
#14650=CARTESIAN_POINT('Ctrl Pts',(2.29518395708476,-2.26266000989839,-35.5912278113247));
#14651=CARTESIAN_POINT('Ctrl Pts',(2.26878020052865,-2.28883244563449,-35.5935118781384));
#14652=CARTESIAN_POINT('Ctrl Pts',(2.26878031087686,-2.28883233625302,-35.8411988517434));
#14653=CARTESIAN_POINT('Ctrl Pts',(2.3352642194958,-2.2229308805301,-35.8358656336423));
#14654=CARTESIAN_POINT('Ctrl Pts',(2.39887845558188,-2.15413101434946,-35.8306078869139));
#14655=CARTESIAN_POINT('Ctrl Pts',(2.58543395974036,-1.93382159103378,-35.8143819814439));
#14656=CARTESIAN_POINT('Ctrl Pts',(2.69765956891768,-1.7739104211318,-35.8034030000764));
#14657=CARTESIAN_POINT('Ctrl Pts',(2.8239873749062,-1.55391820984128,-35.7884331224572));
#14658=CARTESIAN_POINT('Ctrl Pts',(2.85183321938616,-1.50220276761051,-35.7849255811006));
#14659=CARTESIAN_POINT('Ctrl Pts',(2.89807255958858,-1.41040235386445,-35.7787014572064));
#14660=CARTESIAN_POINT('Ctrl Pts',(2.91708557042082,-1.37064614107615,-35.7760067120446));
#14661=CARTESIAN_POINT('Ctrl Pts',(2.95579910417561,-1.28523934759973,-35.7702130346711));
#14662=CARTESIAN_POINT('Ctrl Pts',(2.97527020600965,-1.23949800263655,-35.7671073183813));
#14663=CARTESIAN_POINT('Ctrl Pts',(3.02857798210034,-1.10576583198921,-35.7580123216606));
#14664=CARTESIAN_POINT('Ctrl Pts',(3.05961980623481,-1.01672345909062,-35.751936752157));
#14665=CARTESIAN_POINT('Ctrl Pts',(3.14899064177308,-0.718962594587075,
-35.7315647453863));
#14666=CARTESIAN_POINT('Ctrl Pts',(3.19018363631925,-0.505729780936466,
-35.7168458592631));
#14667=CARTESIAN_POINT('Ctrl Pts',(3.21621819047205,-0.217589292394158,
-35.6974752454061));
#14668=CARTESIAN_POINT('Ctrl Pts',(3.22030896490971,-0.144968167778426,
-35.6926418127545));
#14669=CARTESIAN_POINT('Ctrl Pts',(3.22310572519618,-0.0202788587376412,
-35.6844844986759));
#14670=CARTESIAN_POINT('Ctrl Pts',(3.2230133999614,0.0317337139200843,-35.6811241054923));
#14671=CARTESIAN_POINT('Ctrl Pts',(3.22094058042385,0.111494639841122,-35.6760575422183));
#14672=CARTESIAN_POINT('Ctrl Pts',(3.21985981988505,0.139255677651452,-35.6743102376787));
#14673=CARTESIAN_POINT('Ctrl Pts',(3.21705282575042,0.193351881914526,-35.6709412599188));
#14674=CARTESIAN_POINT('Ctrl Pts',(3.21536186256889,0.219686113523178,-35.6693181418974));
#14675=CARTESIAN_POINT('Ctrl Pts',(3.20994116781044,0.290494126147055,-35.6649925930572));
#14676=CARTESIAN_POINT('Ctrl Pts',(3.20561064170182,0.334917873948849,-35.6623199245407));
#14677=CARTESIAN_POINT('Ctrl Pts',(3.17631952792257,0.582102106214547,-35.6476083543977));
#14678=CARTESIAN_POINT('Ctrl Pts',(3.13304428715088,0.78223958459152,-35.6362756330802));
#14679=CARTESIAN_POINT('Ctrl Pts',(3.03645169598095,1.0858853185833,-35.6183367593132));
#14680=CARTESIAN_POINT('Ctrl Pts',(2.99602741198798,1.19289709093965,-35.6118656414026));
#14681=CARTESIAN_POINT('Ctrl Pts',(2.91613410060458,1.37453884301584,-35.6003855665772));
#14682=CARTESIAN_POINT('Ctrl Pts',(2.8792625904275,1.4501863406919,-35.5954470807774));
#14683=CARTESIAN_POINT('Ctrl Pts',(2.81673491560534,1.5666632412962,-35.5875336598621));
#14684=CARTESIAN_POINT('Ctrl Pts',(2.79304954196039,1.60850961644331,-35.5846252292824));
#14685=CARTESIAN_POINT('Ctrl Pts',(2.74563904741926,1.68806610707185,-35.5789594460696));
#14686=CARTESIAN_POINT('Ctrl Pts',(2.72205062044186,1.72584503196518,-35.5762073889462));
#14687=CARTESIAN_POINT('Ctrl Pts',(2.66348857227354,1.81544867575635,-35.5695245400191));
#14688=CARTESIAN_POINT('Ctrl Pts',(2.62777608443872,1.8667665305759,-35.5655677015226));
#14689=CARTESIAN_POINT('Ctrl Pts',(2.50096445415971,2.03813628233367,-35.5518958649956));
#14690=CARTESIAN_POINT('Ctrl Pts',(2.40295868190494,2.1528128086686,-35.5419380612097));
#14691=CARTESIAN_POINT('Ctrl Pts',(2.15525510626092,2.40458226337193,-35.5182620034814));
#14692=CARTESIAN_POINT('Ctrl Pts',(1.99991099440145,2.535251686477,-35.5044681073185));
#14693=CARTESIAN_POINT('Ctrl Pts',(1.79318309875631,2.67824465028816,-35.4880690820898));
#14694=CARTESIAN_POINT('Ctrl Pts',(1.75241190949501,2.70509761173168,-35.4849221515694));
#14695=CARTESIAN_POINT('Ctrl Pts',(1.68801187211209,2.74544571972678,-35.4801035713358));
#14696=CARTESIAN_POINT('Ctrl Pts',(1.66479702851349,2.75958461610264,-35.4783964515819));
#14697=CARTESIAN_POINT('Ctrl Pts',(1.62113640513057,2.78542439108237,-35.4752451456248));
#14698=CARTESIAN_POINT('Ctrl Pts',(1.60073612904937,2.79719791857979,-35.473796445753));
#14699=CARTESIAN_POINT('Ctrl Pts',(1.5426176152966,2.82989553661957,-35.4697307664582));
#14700=CARTESIAN_POINT('Ctrl Pts',(1.50460446448734,2.8502883457805,-35.4671439672262));
#14701=CARTESIAN_POINT('Ctrl Pts',(1.28271142795066,2.96364985697702,-35.4523924461607));
#14702=CARTESIAN_POINT('Ctrl Pts',(1.09064610887298,3.03958511523094,-35.4409619193667));
#14703=CARTESIAN_POINT('Ctrl Pts',(0.782237031361676,3.12848551765377,-35.4228938048794));
#14704=CARTESIAN_POINT('Ctrl Pts',(0.670227667279095,3.15437936292708,-35.4163919616088));
#14705=CARTESIAN_POINT('Ctrl Pts',(0.47396063935328,3.18882431100243,-35.4048656161305));
#14706=CARTESIAN_POINT('Ctrl Pts',(0.390305945875559,3.20014043336239,-35.399912483523));
#14707=CARTESIAN_POINT('Ctrl Pts',(0.258402061867658,3.21273432512499,-35.3919814673502));
#14708=CARTESIAN_POINT('Ctrl Pts',(0.21040165012732,3.21623448270812,-35.3890706298528));
#14709=CARTESIAN_POINT('Ctrl Pts',(0.117880778127801,3.22090105019819,-35.3834035929523));
#14710=CARTESIAN_POINT('Ctrl Pts',(0.0733790013280007,3.22222200811857,
-35.3806527693102));
#14711=CARTESIAN_POINT('Ctrl Pts',(-0.0335215065450131,3.22317954172133,
-35.373979055508));
#14712=CARTESIAN_POINT('Ctrl Pts',(-0.0959082398382097,3.22192657032154,
-35.3700303058386));
#14713=CARTESIAN_POINT('Ctrl Pts',(-0.306018399468717,3.21159907082808,
-35.356541053828));
#14714=CARTESIAN_POINT('Ctrl Pts',(-0.453128322195566,3.1941636977453,-35.3467681191974));
#14715=CARTESIAN_POINT('Ctrl Pts',(-0.729087873775642,3.1420072133465,-35.3279505750423));
#14716=CARTESIAN_POINT('Ctrl Pts',(-0.858017304166652,3.10927394262781,
-35.3189532245111));
#14717=CARTESIAN_POINT('Ctrl Pts',(-1.05088419609975,3.04739431749685,-35.3054069672449));
#14718=CARTESIAN_POINT('Ctrl Pts',(-1.11650746773125,3.02396788356028,-35.3007833336355));
#14719=CARTESIAN_POINT('Ctrl Pts',(-1.22831092107886,2.97991953374572,-35.292932869543));
#14720=CARTESIAN_POINT('Ctrl Pts',(-1.27486020639078,2.96030407382419,-35.2896727573618));
#14721=CARTESIAN_POINT('Ctrl Pts',(-1.34601587167561,2.92832974515092,-35.2847224724694));
#14722=CARTESIAN_POINT('Ctrl Pts',(-1.37095564778479,2.91673697097014,-35.2829938652967));
#14723=CARTESIAN_POINT('Ctrl Pts',(-1.41680717881892,2.89470568735291,-35.2798319078943));
#14724=CARTESIAN_POINT('Ctrl Pts',(-1.43775916449653,2.88435646789259,-35.2783935120017));
#14725=CARTESIAN_POINT('Ctrl Pts',(-1.49602286287619,2.85478452125253,-35.2744067846416));
#14726=CARTESIAN_POINT('Ctrl Pts',(-1.53307580699154,2.83505873047486,-35.2718866794257));
#14727=CARTESIAN_POINT('Ctrl Pts',(-1.69266361320067,2.74605521466,-35.2610542109695));
#14728=CARTESIAN_POINT('Ctrl Pts',(-1.81098066855724,2.66951035423643,-35.2530755195169));
#14729=CARTESIAN_POINT('Ctrl Pts',(-2.04926574345631,2.49219545733055,-35.2363478372434));
#14730=CARTESIAN_POINT('Ctrl Pts',(-2.1676593229078,2.38993295839145,-35.2276277891041));
#14731=CARTESIAN_POINT('Ctrl Pts',(-2.34943678676138,2.20826123881373,-35.2128897675376));
#14732=CARTESIAN_POINT('Ctrl Pts',(-2.41732314180717,2.13373315065483,-35.2070227981109));
#14733=CARTESIAN_POINT('Ctrl Pts',(-2.51394033186439,2.01712429433846,-35.1979973165043));
#14734=CARTESIAN_POINT('Ctrl Pts',(-2.5453505841666,1.97734073746211,-35.1949434906091));
#14735=CARTESIAN_POINT('Ctrl Pts',(-2.60219508379396,1.90174288323518,-35.189176274664));
#14736=CARTESIAN_POINT('Ctrl Pts',(-2.62786078929637,1.86611699212361,-35.1864725945987));
#14737=CARTESIAN_POINT('Ctrl Pts',(-2.68462179330101,1.78383463048775,-35.18025415793));
#14738=CARTESIAN_POINT('Ctrl Pts',(-2.71524271338279,1.7368697589535,-35.176723101184));
#14739=CARTESIAN_POINT('Ctrl Pts',(-2.82841102645769,1.55298587523434,-35.162957664705));
#14740=CARTESIAN_POINT('Ctrl Pts',(-2.90194338697604,1.41081077965373,-35.1524239716011));
#14741=CARTESIAN_POINT('Ctrl Pts',(-3.02672111244333,1.11810393665668,-35.1311116787717));
#14742=CARTESIAN_POINT('Ctrl Pts',(-3.07800034025221,0.968045029552722,
-35.1203664802707));
#14743=CARTESIAN_POINT('Ctrl Pts',(-3.13888207863788,0.735072530136991,
-35.10435627566));
#14744=CARTESIAN_POINT('Ctrl Pts',(-3.15665756691841,0.654543679398243,
-35.0989424729181));
#14745=CARTESIAN_POINT('Ctrl Pts',(-3.17709247811663,0.541526666860606,
-35.091584894491));
#14746=CARTESIAN_POINT('Ctrl Pts',(-3.18237742946235,0.509550616572541,
-35.0895297597963));
#14747=CARTESIAN_POINT('Ctrl Pts',(-3.19088423345794,0.452769939489621,
-35.0859336285606));
#14748=CARTESIAN_POINT('Ctrl Pts',(-3.19430103518963,0.42799974433517,-35.0843832261971));
#14749=CARTESIAN_POINT('Ctrl Pts',(-3.2017677143166,0.368786485915752,-35.0807192467316));
#14750=CARTESIAN_POINT('Ctrl Pts',(-3.20555056969504,0.33431382764763,-35.0786193530487));
#14751=CARTESIAN_POINT('Ctrl Pts',(-3.21813227936215,0.199644456009511,
-35.0705221942678));
#14752=CARTESIAN_POINT('Ctrl Pts',(-3.22279592866093,0.0991116701523034,
-35.0647053698551));
#14753=CARTESIAN_POINT('Ctrl Pts',(-3.22268034131199,-0.152185129279559,
-35.0503857923619));
#14754=CARTESIAN_POINT('Ctrl Pts',(-3.21204041784068,-0.302700064493506,
-35.0420003717722));
#14755=CARTESIAN_POINT('Ctrl Pts',(-3.17690790664443,-0.550762571349196,
-35.0278440136735));
#14756=CARTESIAN_POINT('Ctrl Pts',(-3.15832478350957,-0.648896053149135,
-35.0221561023034));
#14757=CARTESIAN_POINT('Ctrl Pts',(-3.1173656588011,-0.821034149274176,
-35.0118733855988));
#14758=CARTESIAN_POINT('Ctrl Pts',(-3.09682641937535,-0.895394074366066,
-35.0073280223274));
#14759=CARTESIAN_POINT('Ctrl Pts',(-3.05954018946172,-1.01367203911393,
-34.9998867429761));
#14760=CARTESIAN_POINT('Ctrl Pts',(-3.04446522857545,-1.05808709620345,
-34.997043490985));
#14761=CARTESIAN_POINT('Ctrl Pts',(-3.0129936634984,-1.14456247841059,-34.9914028999584));
#14762=CARTESIAN_POINT('Ctrl Pts',(-2.99667191798091,-1.18663860559836,
-34.9886085216076));
#14763=CARTESIAN_POINT('Ctrl Pts',(-2.954132665167,-1.28982081289588,-34.9816258636257));
#14764=CARTESIAN_POINT('Ctrl Pts',(-2.92689832369941,-1.35048240710605,
-34.9774052862986));
#14765=CARTESIAN_POINT('Ctrl Pts',(-2.86273139085445,-1.48233338362255,
-34.9679685814317));
#14766=CARTESIAN_POINT('Ctrl Pts',(-2.82497888557456,-1.55307310185483,
-34.9627293401044));
#14767=CARTESIAN_POINT('Ctrl Pts',(-2.68034599700982,-1.80132697538337,
-34.9437270797267));
#14768=CARTESIAN_POINT('Ctrl Pts',(-2.55904553647452,-1.9698505967047,-34.9296189284839));
#14769=CARTESIAN_POINT('Ctrl Pts',(-2.36499114692388,-2.19100837949097,
-34.9100136975336));
#14770=CARTESIAN_POINT('Ctrl Pts',(-2.30492239037816,-2.25411534085376,
-34.9042789500282));
#14771=CARTESIAN_POINT('Ctrl Pts',(-2.21842303076359,-2.33791106277472,
-34.8965486938852));
#14772=CARTESIAN_POINT('Ctrl Pts',(-2.19411981155172,-2.36073449081934,
-34.8944305826072));
#14773=CARTESIAN_POINT('Ctrl Pts',(-2.15099360866885,-2.39999334233975,
-34.8907714930869));
#14774=CARTESIAN_POINT('Ctrl Pts',(-2.13232694087042,-2.41659336063151,
-34.8892196429684));
#14775=CARTESIAN_POINT('Ctrl Pts',(-2.08851885528587,-2.45464837643007,
-34.8856508181931));
#14776=CARTESIAN_POINT('Ctrl Pts',(-2.06323749636522,-2.47593636625069,
-34.8836449300139));
#14777=CARTESIAN_POINT('Ctrl Pts',(-1.96944395792036,-2.55248003043506,
-34.8763783696987));
#14778=CARTESIAN_POINT('Ctrl Pts',(-1.89899923460882,-2.60531537463542,
-34.8712553214422));
#14779=CARTESIAN_POINT('Ctrl Pts',(-1.67611131819944,-2.75863657529509,
-34.8557534295035));
#14780=CARTESIAN_POINT('Ctrl Pts',(-1.51723033107526,-2.84911242478676,
-34.8456478666228));
#14781=CARTESIAN_POINT('Ctrl Pts',(-1.2325763064649,-2.98061166511535,-34.8278787439843));
#14782=CARTESIAN_POINT('Ctrl Pts',(-1.1103813351518,-3.02825673617044,-34.8203512212046));
#14783=CARTESIAN_POINT('Ctrl Pts',(-0.932573740909747,-3.08537348604897,
-34.8092942211876));
#14784=CARTESIAN_POINT('Ctrl Pts',(-0.879084006879159,-3.10103758323379,
-34.8059561050844));
#14785=CARTESIAN_POINT('Ctrl Pts',(-0.782864059520709,-3.12652540206666,
-34.7999154501342));
#14786=CARTESIAN_POINT('Ctrl Pts',(-0.740288127713118,-3.13687909008653,
-34.7972302707906));
#14787=CARTESIAN_POINT('Ctrl Pts',(-0.647168477502677,-3.15752275776517,
-34.7913248161217));
#14788=CARTESIAN_POINT('Ctrl Pts',(-0.596562834274296,-3.16747364816955,
-34.7880948161093));
#14789=CARTESIAN_POINT('Ctrl Pts',(-0.440220340477743,-3.19433674738178,
-34.778045163548));
#14790=CARTESIAN_POINT('Ctrl Pts',(-0.333870324497253,-3.20719627244352,
-34.7711075457247));
#14791=CARTESIAN_POINT('Ctrl Pts',(-0.0511483941743684,-3.22716748116875,
-34.7524223410741));
#14792=CARTESIAN_POINT('Ctrl Pts',(0.125504346323852,-3.22513059804636,
-34.7404856274706));
#14793=CARTESIAN_POINT('Ctrl Pts',(0.423597963677889,-3.19715860171786,
-34.7203725358168));
#14794=CARTESIAN_POINT('Ctrl Pts',(0.545359649590148,-3.17865479436919,
-34.7121725513879));
#14795=CARTESIAN_POINT('Ctrl Pts',(0.701251356756557,-3.14573979964565,
-34.7019096268518));
#14796=CARTESIAN_POINT('Ctrl Pts',(0.736602010426943,-3.13765040836752,
-34.6995986467861));
#14797=CARTESIAN_POINT('Ctrl Pts',(0.796196375762298,-3.1229504894476,-34.6957388020278));
#14798=CARTESIAN_POINT('Ctrl Pts',(0.820511722950976,-3.11665029869525,
-34.6941745124122));
#14799=CARTESIAN_POINT('Ctrl Pts',(0.874901520807166,-3.10187699040634,
-34.6907004487907));
#14800=CARTESIAN_POINT('Ctrl Pts',(0.904930385116731,-3.09324986082381,
-34.6887988009628));
#14801=CARTESIAN_POINT('Ctrl Pts',(1.00506989321956,-3.06289714638004,-34.6824978952339));
#14802=CARTESIAN_POINT('Ctrl Pts',(1.07456692700322,-3.03921238262024,-34.6781921643721));
#14803=CARTESIAN_POINT('Ctrl Pts',(1.26162385029788,-2.96824290739178,-34.6666382961886));
#14804=CARTESIAN_POINT('Ctrl Pts',(1.37730259368907,-2.91636784184618,-34.6595293006397));
#14805=CARTESIAN_POINT('Ctrl Pts',(1.65502558558038,-2.77160515790573,-34.6419265578614));
#14806=CARTESIAN_POINT('Ctrl Pts',(1.81260872761203,-2.67120698321779,-34.6314373418852));
#14807=CARTESIAN_POINT('Ctrl Pts',(2.01120362071568,-2.51897593697931,-34.6167429855911));
#14808=CARTESIAN_POINT('Ctrl Pts',(2.06062351542123,-2.47871130162602,-34.6129523952937));
#14809=CARTESIAN_POINT('Ctrl Pts',(2.14262412661997,-2.40775380598445,-34.6064062785327));
#14810=CARTESIAN_POINT('Ctrl Pts',(2.17581945505171,-2.37779854808404,-34.6036803003651));
#14811=CARTESIAN_POINT('Ctrl Pts',(2.22876678606824,-2.32798190370282,-34.5992011997548));
#14812=CARTESIAN_POINT('Ctrl Pts',(2.24890195437326,-2.30853654037346,-34.597465658131));
#14813=CARTESIAN_POINT('Ctrl Pts',(2.26878020184338,-2.28883244433128,-34.5957191253299));
#14814=CARTESIAN_POINT('Origin',(0.,0.,-41.3107734492731));
#14815=CARTESIAN_POINT('',(2.26878017716708,-2.2888324687914,-33.0953665650246));
#14816=CARTESIAN_POINT('',(2.26878022243768,-2.28883242391741,-33.3405291647262));
#14817=CARTESIAN_POINT('',(2.26878020078428,-2.2888324453811,-41.3107734492731));
#14818=CARTESIAN_POINT('Ctrl Pts',(2.26878017716708,-2.2888324687914,-33.0953665650246));
#14819=CARTESIAN_POINT('Ctrl Pts',(2.25513518290648,-2.30235792026857,-33.0966503519412));
#14820=CARTESIAN_POINT('Ctrl Pts',(2.2413678000685,-2.31576278083686,-33.0979366661943));
#14821=CARTESIAN_POINT('Ctrl Pts',(2.08286720356223,-2.46735143037641,-33.1126403973839));
#14822=CARTESIAN_POINT('Ctrl Pts',(1.92568569537045,-2.59189080711268,-33.1262646258381));
#14823=CARTESIAN_POINT('Ctrl Pts',(1.71620807102168,-2.72822831962593,-33.1425841306978));
#14824=CARTESIAN_POINT('Ctrl Pts',(1.67382313920823,-2.75443580311782,-33.1457987636766));
#14825=CARTESIAN_POINT('Ctrl Pts',(1.60723780360399,-2.79350198703619,-33.1506960970612));
#14826=CARTESIAN_POINT('Ctrl Pts',(1.58345400366048,-2.80705187850117,-33.1524160342899));
#14827=CARTESIAN_POINT('Ctrl Pts',(1.53898885258495,-2.83163913499436,-33.1555734248723));
#14828=CARTESIAN_POINT('Ctrl Pts',(1.51835455793478,-2.84275682615637,-33.1570157123206));
#14829=CARTESIAN_POINT('Ctrl Pts',(1.46004330051404,-2.87335868486747,-33.1610326168507));
#14830=CARTESIAN_POINT('Ctrl Pts',(1.42209890099693,-2.89232634112015,-33.1635782642917));
#14831=CARTESIAN_POINT('Ctrl Pts',(1.19693712200369,-2.9993774020375,-33.1783503480835));
#14832=CARTESIAN_POINT('Ctrl Pts',(1.00194484908313,-3.07002406313783,-33.1898287210299));
#14833=CARTESIAN_POINT('Ctrl Pts',(0.689959120139942,-3.15013294156086,
-33.2079601832759));
#14834=CARTESIAN_POINT('Ctrl Pts',(0.576959686460083,-3.17277426477144,
-33.2144772147706));
#14835=CARTESIAN_POINT('Ctrl Pts',(0.379353359645486,-3.20146093324465,
-33.226026467992));
#14836=CARTESIAN_POINT('Ctrl Pts',(0.295271051875767,-3.21030752864928,
-33.2309868774288));
#14837=CARTESIAN_POINT('Ctrl Pts',(0.162899144393818,-3.2189904552102,-33.2389267232889));
#14838=CARTESIAN_POINT('Ctrl Pts',(0.114792996079793,-3.22106471252725,
-33.2418388482718));
#14839=CARTESIAN_POINT('Ctrl Pts',(0.0221571438913656,-3.22298122841051,
-33.2475067653327));
#14840=CARTESIAN_POINT('Ctrl Pts',(-0.0223584445544171,-3.22297979085081,
-33.2502571432136));
#14841=CARTESIAN_POINT('Ctrl Pts',(-0.129180639200564,-3.22076321688906,
-33.2569269144018));
#14842=CARTESIAN_POINT('Ctrl Pts',(-0.19144893514027,-3.21766216524124,
-33.260872081195));
#14843=CARTESIAN_POINT('Ctrl Pts',(-0.500463146355082,-3.19327147973357,
-33.280747707219));
#14844=CARTESIAN_POINT('Ctrl Pts',(-0.74424233835898,-3.14539570446211,
-33.2974621844789));
#14845=CARTESIAN_POINT('Ctrl Pts',(-1.06486340831942,-3.04304161805856,
-33.3200897644635));
#14846=CARTESIAN_POINT('Ctrl Pts',(-1.14848303963809,-3.01247814227129,
-33.326043727433));
#14847=CARTESIAN_POINT('Ctrl Pts',(-1.28564488330281,-2.95580189397782,
-33.3358000483637));
#14848=CARTESIAN_POINT('Ctrl Pts',(-1.33992168706782,-2.93159656184382,
-33.3396576959825));
#14849=CARTESIAN_POINT('Ctrl Pts',(-1.41973569084597,-2.89332242051299,
-33.3452948122007));
#14850=CARTESIAN_POINT('Ctrl Pts',(-1.44579942754109,-2.88038681751157,
-33.3471298171583));
#14851=CARTESIAN_POINT('Ctrl Pts',(-1.49425773645198,-2.85551311160995,
-33.3505256595042));
#14852=CARTESIAN_POINT('Ctrl Pts',(-1.51669230236408,-2.84366063445182,
-33.3520908203042));
#14853=CARTESIAN_POINT('Ctrl Pts',(-1.57430094990484,-2.81234950173778,
-33.3560966624343));
#14854=CARTESIAN_POINT('Ctrl Pts',(-1.6092563386829,-2.79249486374002,-33.3585146658838));
#14855=CARTESIAN_POINT('Ctrl Pts',(-1.82412891528854,-2.66507213151402,
-33.3733559610289));
#14856=CARTESIAN_POINT('Ctrl Pts',(-1.99358372486125,-2.54080677522296,
-33.3849861482271));
#14857=CARTESIAN_POINT('Ctrl Pts',(-2.23625067278748,-2.32352576272029,
-33.4033187248563));
#14858=CARTESIAN_POINT('Ctrl Pts',(-2.31847104350024,-2.2414903350086,-33.4098842228074));
#14859=CARTESIAN_POINT('Ctrl Pts',(-2.45287922393343,-2.09205970325972,
-33.4215062511335));
#14860=CARTESIAN_POINT('Ctrl Pts',(-2.50715246175046,-2.02670055657058,
-33.4264895332933));
#14861=CARTESIAN_POINT('Ctrl Pts',(-2.58808962786105,-1.92099821046018,
-33.4344567627992));
#14862=CARTESIAN_POINT('Ctrl Pts',(-2.61653682317474,-1.88206714287472,
-33.4373725435977));
#14863=CARTESIAN_POINT('Ctrl Pts',(-2.66953166546536,-1.80601692018826,
-33.4430422083021));
#14864=CARTESIAN_POINT('Ctrl Pts',(-2.69420492630011,-1.76899856958464,
-33.4457905525562));
#14865=CARTESIAN_POINT('Ctrl Pts',(-2.75149098626182,-1.67907020052297,
-33.4524458217324));
#14866=CARTESIAN_POINT('Ctrl Pts',(-2.78335387907905,-1.62570592191355,
-33.456378228878));
#14867=CARTESIAN_POINT('Ctrl Pts',(-2.91939440476421,-1.38212886629318,
-33.4742641091173));
#14868=CARTESIAN_POINT('Ctrl Pts',(-3.00574296928829,-1.18263609477538,
-33.4887959230864));
#14869=CARTESIAN_POINT('Ctrl Pts',(-3.10430948207055,-0.872460667001341,
-33.5107168227683));
#14870=CARTESIAN_POINT('Ctrl Pts',(-3.13196075265785,-0.767299589019079,
-33.5180289730792));
#14871=CARTESIAN_POINT('Ctrl Pts',(-3.16803231808227,-0.595152646469083,
-33.5296436145815));
#14872=CARTESIAN_POINT('Ctrl Pts',(-3.17975668556551,-0.528946243713139,
-33.534026750248));
#14873=CARTESIAN_POINT('Ctrl Pts',(-3.19375641491715,-0.432386762982047,
-33.5402554593491));
#14874=CARTESIAN_POINT('Ctrl Pts',(-3.19768623877609,-0.402294951309812,
-33.5421736250841));
#14875=CARTESIAN_POINT('Ctrl Pts',(-3.20411008306368,-0.347037924226917,
-33.5456485452067));
#14876=CARTESIAN_POINT('Ctrl Pts',(-3.20673379298496,-0.321893095036145,
-33.5472113168359));
#14877=CARTESIAN_POINT('Ctrl Pts',(-3.21253877950483,-0.259110989934605,
-33.5510708370597));
#14878=CARTESIAN_POINT('Ctrl Pts',(-3.21535482197858,-0.221444261801844,
-33.5533490151824));
#14879=CARTESIAN_POINT('Ctrl Pts',(-3.22945337670295,0.0254451694556208,
-33.5680870235743));
#14880=CARTESIAN_POINT('Ctrl Pts',(-3.22097239020679,0.235316330868668,
-33.5797260394388));
#14881=CARTESIAN_POINT('Ctrl Pts',(-3.17582410463868,0.560721496509795,
-33.5982081408355));
#14882=CARTESIAN_POINT('Ctrl Pts',(-3.15296643102383,0.677545446060423,
-33.6049291498048));
#14883=CARTESIAN_POINT('Ctrl Pts',(-3.10249245064262,0.876409154352357,
-33.6167840495007));
#14884=CARTESIAN_POINT('Ctrl Pts',(-3.07793584415687,0.959094160048735,
-33.6218400001516));
#14885=CARTESIAN_POINT('Ctrl Pts',(-3.03445719448557,1.08652300457852,-33.6298945094339));
#14886=CARTESIAN_POINT('Ctrl Pts',(-3.01778886182617,1.13199501612168,-33.6328221668055));
#14887=CARTESIAN_POINT('Ctrl Pts',(-2.98388351142591,1.21841241530387,-33.6384984716431));
#14888=CARTESIAN_POINT('Ctrl Pts',(-2.96681197181193,1.25941099101307,-33.6412411915081));
#14889=CARTESIAN_POINT('Ctrl Pts',(-2.92405979523054,1.35638620065473,-33.6478540497705));
#14890=CARTESIAN_POINT('Ctrl Pts',(-2.8976118914326,1.41200344714246,-33.6517488044581));
#14891=CARTESIAN_POINT('Ctrl Pts',(-2.76844559137495,1.66469468424587,-33.6699325423795));
#14892=CARTESIAN_POINT('Ctrl Pts',(-2.64712144118443,1.85154547174523,-33.6848360126741));
#14893=CARTESIAN_POINT('Ctrl Pts',(-2.44097011282467,2.10689897326052,-33.7069385796269));
#14894=CARTESIAN_POINT('Ctrl Pts',(-2.37033777372358,2.18606016015702,-33.7140683960266));
#14895=CARTESIAN_POINT('Ctrl Pts',(-2.24944774491906,2.30878529938712,-33.725438123356));
#14896=CARTESIAN_POINT('Ctrl Pts',(-2.20151919041601,2.3545316288309,-33.7297551558329));
#14897=CARTESIAN_POINT('Ctrl Pts',(-2.12973675486259,2.41893585094417,-33.7359100645792));
#14898=CARTESIAN_POINT('Ctrl Pts',(-2.10697867246153,2.43878460029075,-33.7378182854353));
#14899=CARTESIAN_POINT('Ctrl Pts',(-2.06463143179795,2.47468293264917,-33.7412853495083));
#14900=CARTESIAN_POINT('Ctrl Pts',(-2.0451278329901,2.49082531496769,-33.7428499550626));
#14901=CARTESIAN_POINT('Ctrl Pts',(-1.99583681753157,2.53065226290494,-33.7467281503791));
#14902=CARTESIAN_POINT('Ctrl Pts',(-1.96581671579061,2.55404197318377,-33.7490227186743));
#14903=CARTESIAN_POINT('Ctrl Pts',(-1.76990160376916,2.70118481668855,-33.7636196026392));
#14904=CARTESIAN_POINT('Ctrl Pts',(-1.59280807428144,2.80925847559134,-33.775124693466));
#14905=CARTESIAN_POINT('Ctrl Pts',(-1.29851769894735,2.95201420267694,-33.7935234837422));
#14906=CARTESIAN_POINT('Ctrl Pts',(-1.18764046013171,2.99834020625426,-33.8003050504581));
#14907=CARTESIAN_POINT('Ctrl Pts',(-0.992679404864649,3.06728320257979,
-33.8122502858677));
#14908=CARTESIAN_POINT('Ctrl Pts',(-0.90978865695149,3.09288238958538,-33.817334151159));
#14909=CARTESIAN_POINT('Ctrl Pts',(-0.779082383471197,3.12753917872972,
-33.8254222140341));
#14910=CARTESIAN_POINT('Ctrl Pts',(-0.731921029369964,3.13891094270284,
-33.8283544495412));
#14911=CARTESIAN_POINT('Ctrl Pts',(-0.641154254754654,3.15864028930871,
-33.8340334998117));
#14912=CARTESIAN_POINT('Ctrl Pts',(-0.597597393427313,3.16716976312302,
-33.8367742410062));
#14913=CARTESIAN_POINT('Ctrl Pts',(-0.493423269460232,3.18534414007337,
-33.8433717220453));
#14914=CARTESIAN_POINT('Ctrl Pts',(-0.432681166047868,3.19416186606653,
-33.8472527628742));
#14915=CARTESIAN_POINT('Ctrl Pts',(-0.149161112198021,3.22708416691309,
-33.8655376640036));
#14916=CARTESIAN_POINT('Ctrl Pts',(0.0754645436143387,3.2296437681523,-33.8805687433087));
#14917=CARTESIAN_POINT('Ctrl Pts',(0.403194128887664,3.19915728413175,-33.9027352765442));
#14918=CARTESIAN_POINT('Ctrl Pts',(0.507351232064744,3.18430045068996,-33.9098043918657));
#14919=CARTESIAN_POINT('Ctrl Pts',(0.675310769280718,3.15189092876012,-33.9210922977994));
#14920=CARTESIAN_POINT('Ctrl Pts',(0.739628699154956,3.13742117910994,-33.9253870426276));
#14921=CARTESIAN_POINT('Ctrl Pts',(0.832654173036695,3.11347286267701,-33.9315170452971));
#14922=CARTESIAN_POINT('Ctrl Pts',(0.861740983126144,3.10554807926666,-33.9334218953873));
#14923=CARTESIAN_POINT('Ctrl Pts',(0.915057744129675,3.09021496704233,-33.9368863356755));
#14924=CARTESIAN_POINT('Ctrl Pts',(0.939317027293624,3.0829276306688,-33.9384516013507));
#14925=CARTESIAN_POINT('Ctrl Pts',(0.999895941088634,3.06394862010903,-33.9423363319439));
#14926=CARTESIAN_POINT('Ctrl Pts',(1.03609819125512,3.05189676473568,-33.944636617782));
#14927=CARTESIAN_POINT('Ctrl Pts',(1.26640816662163,2.97065489779202,-33.9591839687126));
#14928=CARTESIAN_POINT('Ctrl Pts',(1.45373681265877,2.88361731984841,-33.9706419824356));
#14929=CARTESIAN_POINT('Ctrl Pts',(1.73538184648514,2.71828648359193,-33.989011692974));
#14930=CARTESIAN_POINT('Ctrl Pts',(1.83577203909949,2.65152227255239,-33.9958146326008));
#14931=CARTESIAN_POINT('Ctrl Pts',(2.00173381057107,2.52719820325288,-34.0077916897256));
#14932=CARTESIAN_POINT('Ctrl Pts',(2.06914227549585,2.47231014881584,-34.0128853398841));
#14933=CARTESIAN_POINT('Ctrl Pts',(2.17061542892803,2.38262504125599,-34.0209851389862));
#14934=CARTESIAN_POINT('Ctrl Pts',(2.20625146237104,2.34966540946579,-34.0239189510395));
#14935=CARTESIAN_POINT('Ctrl Pts',(2.27301420244556,2.28505860344945,-34.0295989072626));
#14936=CARTESIAN_POINT('Ctrl Pts',(2.30425819509295,2.25354836950868,-34.0323389266786));
#14937=CARTESIAN_POINT('Ctrl Pts',(2.37709179606774,2.17699551326187,-34.0389309594077));
#14938=CARTESIAN_POINT('Ctrl Pts',(2.41806503719888,2.13139286732515,-34.0428071635249));
#14939=CARTESIAN_POINT('Ctrl Pts',(2.62198078357479,1.89098536190384,-34.0630007882741));
#14940=CARTESIAN_POINT('Ctrl Pts',(2.76276276864001,1.67860432457326,-34.0801548260348));
#14941=CARTESIAN_POINT('Ctrl Pts',(2.91618824585569,1.37458166249732,-34.1030404633608));
#14942=CARTESIAN_POINT('Ctrl Pts',(2.95209928004865,1.29566195351805,-34.1088344401637));
#14943=CARTESIAN_POINT('Ctrl Pts',(3.00681584290379,1.16128727718757,-34.1183663352648));
#14944=CARTESIAN_POINT('Ctrl Pts',(3.02737156840673,1.10659474388166,-34.1221567268739));
#14945=CARTESIAN_POINT('Ctrl Pts',(3.05586610072001,1.02402953427941,-34.1277172174223));
#14946=CARTESIAN_POINT('Ctrl Pts',(3.0649337319084,0.996561825332186,-34.1295408102141));
#14947=CARTESIAN_POINT('Ctrl Pts',(3.08127937266239,0.944712724952865,-34.132929152254));
#14948=CARTESIAN_POINT('Ctrl Pts',(3.08864049603775,0.920361137104176,-34.1344979240421));
#14949=CARTESIAN_POINT('Ctrl Pts',(3.10700725064891,0.856897969454276,-34.1385329862793));
#14950=CARTESIAN_POINT('Ctrl Pts',(3.11756338058618,0.817659519530494,-34.1409758948028));
#14951=CARTESIAN_POINT('Ctrl Pts',(3.17137297685285,0.601421648596455,-34.1542071474229));
#14952=CARTESIAN_POINT('Ctrl Pts',(3.20030223372359,0.42118159973948,-34.1644049639806));
#14953=CARTESIAN_POINT('Ctrl Pts',(3.22833380326741,0.044943813274584,-34.1856104600273));
#14954=CARTESIAN_POINT('Ctrl Pts',(3.22513769176329,-0.150454589831461,
-34.1965927607226));
#14955=CARTESIAN_POINT('Ctrl Pts',(3.19802443635561,-0.402748389013214,
-34.2115663513047));
#14956=CARTESIAN_POINT('Ctrl Pts',(3.19015460947218,-0.460954984497453,
-34.2150739233834));
#14957=CARTESIAN_POINT('Ctrl Pts',(3.17360407226503,-0.562402487549828,
-34.2212980813588));
#14958=CARTESIAN_POINT('Ctrl Pts',(3.16561782684986,-0.605741569158405,
-34.2239928290579));
#14959=CARTESIAN_POINT('Ctrl Pts',(3.14673698999318,-0.697592153456303,
-34.2297864905141));
#14960=CARTESIAN_POINT('Ctrl Pts',(3.13560345814871,-0.746042239054158,
-34.2328921878864));
#14961=CARTESIAN_POINT('Ctrl Pts',(3.10012521323423,-0.885565348201471,
-34.2419870469939));
#14962=CARTESIAN_POINT('Ctrl Pts',(3.0729014764931,-0.975846361725071,-34.2480624936056));
#14963=CARTESIAN_POINT('Ctrl Pts',(2.97018489822096,-1.26927235750758,-34.2684345690076));
#14964=CARTESIAN_POINT('Ctrl Pts',(2.87817451151786,-1.46599696375291,-34.2831536722957));
#14965=CARTESIAN_POINT('Ctrl Pts',(2.72987057081456,-1.71441278346529,-34.3025244865525));
#14966=CARTESIAN_POINT('Ctrl Pts',(2.69049452599039,-1.77556886134533,-34.307357908211));
#14967=CARTESIAN_POINT('Ctrl Pts',(2.61946673923537,-1.87808832109708,-34.3155152062688));
#14968=CARTESIAN_POINT('Ctrl Pts',(2.58881986581317,-1.92011304333786,-34.3188755942587));
#14969=CARTESIAN_POINT('Ctrl Pts',(2.54026067673939,-1.98342253963959,-34.32394215152));
#14970=CARTESIAN_POINT('Ctrl Pts',(2.523068802453,-2.00524642394919,-34.3256894551054));
#14971=CARTESIAN_POINT('Ctrl Pts',(2.48900094624645,-2.04736125880574,-34.3290584325427));
#14972=CARTESIAN_POINT('Ctrl Pts',(2.4721540476785,-2.06767218408784,-34.3306815511669));
#14973=CARTESIAN_POINT('Ctrl Pts',(2.42614866163923,-2.12177091478953,-34.3350071039688));
#14974=CARTESIAN_POINT('Ctrl Pts',(2.39653352839163,-2.15516510292579,-34.3376797757416));
#14975=CARTESIAN_POINT('Ctrl Pts',(2.33447250556559,-2.22228355789538,-34.3430826064246));
#14976=CARTESIAN_POINT('Ctrl Pts',(2.30198005379905,-2.25592345578822,-34.3458075242752));
#14977=CARTESIAN_POINT('Ctrl Pts',(2.2687801086558,-2.28883253670245,-34.3485046109761));
#14978=CARTESIAN_POINT('Ctrl Pts',(2.26878020184338,-2.28883244433128,-34.5957191253299));
#14979=CARTESIAN_POINT('Ctrl Pts',(2.28275431418291,-2.2749807578556,-34.5944913387453));
#14980=CARTESIAN_POINT('Ctrl Pts',(2.29660145941807,-2.26100120851142,-34.5932581244753));
#14981=CARTESIAN_POINT('Ctrl Pts',(2.36726430182595,-2.18834372672855,-34.586878066658));
#14982=CARTESIAN_POINT('Ctrl Pts',(2.42195799566748,-2.12765274332109,-34.5816453573719));
#14983=CARTESIAN_POINT('Ctrl Pts',(2.54417663641725,-1.98120703338518,-34.5692349639376));
#14984=CARTESIAN_POINT('Ctrl Pts',(2.60976706956622,-1.89397168328745,-34.5620004317896));
#14985=CARTESIAN_POINT('Ctrl Pts',(2.79533776067639,-1.61917284960125,-34.5397859401555));
#14986=CARTESIAN_POINT('Ctrl Pts',(2.90043913069693,-1.4223549679812,-34.5245974973487));
#14987=CARTESIAN_POINT('Ctrl Pts',(2.99954093615506,-1.17918438778175,-34.5076072903031));
#14988=CARTESIAN_POINT('Ctrl Pts',(3.01396438259134,-1.14181464329064,-34.5050443534769));
#14989=CARTESIAN_POINT('Ctrl Pts',(3.03637307326663,-1.08036968935533,-34.5009189546891));
#14990=CARTESIAN_POINT('Ctrl Pts',(3.04477716846044,-1.05645268169334,-34.4993349144063));
#14991=CARTESIAN_POINT('Ctrl Pts',(3.06223732723952,-1.0048232888163,-34.4959648378351));
#14992=CARTESIAN_POINT('Ctrl Pts',(3.07120112559852,-0.977082942840127,
-34.4941836577518));
#14993=CARTESIAN_POINT('Ctrl Pts',(3.09738594297763,-0.8921254334767,-34.4888076273285));
#14994=CARTESIAN_POINT('Ctrl Pts',(3.11339410979983,-0.834545090850007,
-34.4852722970275));
#14995=CARTESIAN_POINT('Ctrl Pts',(3.14942446318477,-0.689421692088562,
-34.4765561336581));
#14996=CARTESIAN_POINT('Ctrl Pts',(3.16740718754507,-0.601423415670002,
-34.4714442047867));
#14997=CARTESIAN_POINT('Ctrl Pts',(3.22076408682028,-0.270358203708891,
-34.4524983364445));
#14998=CARTESIAN_POINT('Ctrl Pts',(3.23199925033774,-0.0242782529003616,
-34.4389161158309));
#14999=CARTESIAN_POINT('Ctrl Pts',(3.21089289386406,0.283218939623277,-34.420798660998));
#15000=CARTESIAN_POINT('Ctrl Pts',(3.204777719176,0.345608395335527,-34.4170678039333));
#15001=CARTESIAN_POINT('Ctrl Pts',(3.19120969630814,0.451977550233154,-34.4105907388083));
#15002=CARTESIAN_POINT('Ctrl Pts',(3.18465580620903,0.496054561874655,-34.4078724178608));
#15003=CARTESIAN_POINT('Ctrl Pts',(3.16914429757165,0.587322799796455,-34.402165523574));
#15004=CARTESIAN_POINT('Ctrl Pts',(3.16004132848768,0.634477790566203,-34.399173090636));
#15005=CARTESIAN_POINT('Ctrl Pts',(3.1321753072958,0.763291388460768,-34.3908712568216));
#15006=CARTESIAN_POINT('Ctrl Pts',(3.11127739106761,0.844444756922051,-34.3854982290444));
#15007=CARTESIAN_POINT('Ctrl Pts',(3.05466245178758,1.03346457621671,-34.3726437078281));
#15008=CARTESIAN_POINT('Ctrl Pts',(3.01635749649642,1.14043663225102,-34.3650989157743));
#15009=CARTESIAN_POINT('Ctrl Pts',(2.89105753980571,1.43955786079567,-34.3433455914678));
#15010=CARTESIAN_POINT('Ctrl Pts',(2.79074818166118,1.62550672723553,-34.3289864507506));
#15011=CARTESIAN_POINT('Ctrl Pts',(2.6495864078017,1.83509281791907,-34.3126045728813));
#15012=CARTESIAN_POINT('Ctrl Pts',(2.62549859376958,1.86939329465406,-34.3099181087708));
#15013=CARTESIAN_POINT('Ctrl Pts',(2.58695372173706,1.92206491913183,-34.3057959308746));
#15014=CARTESIAN_POINT('Ctrl Pts',(2.57295494921852,1.94076429396683,-34.3043331370721));
#15015=CARTESIAN_POINT('Ctrl Pts',(2.54202307249814,1.98115964575032,-34.3011774570349));
#15016=CARTESIAN_POINT('Ctrl Pts',(2.52501288363555,2.00279427357257,-34.2994899195145));
#15017=CARTESIAN_POINT('Ctrl Pts',(2.47594389590218,2.06358424694428,-34.2947471245486));
#15018=CARTESIAN_POINT('Ctrl Pts',(2.44323596504014,2.10220758666463,-34.291732436312));
#15019=CARTESIAN_POINT('Ctrl Pts',(2.36324269945501,2.19227766636083,-34.2846555737673));
#15020=CARTESIAN_POINT('Ctrl Pts',(2.31516683158788,2.24298929271774,-34.2806329062166));
#15021=CARTESIAN_POINT('Ctrl Pts',(2.17117198606978,2.38531167123716,-34.2690959575433));
#15022=CARTESIAN_POINT('Ctrl Pts',(2.07120086263719,2.47261566851285,-34.2616972355133));
#15023=CARTESIAN_POINT('Ctrl Pts',(1.84893457844744,2.64375441405337,-34.245889239122));
#15024=CARTESIAN_POINT('Ctrl Pts',(1.72567168717498,2.72581148782508,-34.2374775909167));
#15025=CARTESIAN_POINT('Ctrl Pts',(1.54303214809534,2.8300284839086,-34.2251136782484));
#15026=CARTESIAN_POINT('Ctrl Pts',(1.48796449225416,2.85936537673015,-34.2213994116818));
#15027=CARTESIAN_POINT('Ctrl Pts',(1.39220167180797,2.90686668046207,-34.214941439447));
#15028=CARTESIAN_POINT('Ctrl Pts',(1.35191665529052,2.92581962045885,-34.2122251630985));
#15029=CARTESIAN_POINT('Ctrl Pts',(1.26729144825611,2.96351244704122,-34.2065135033633));
#15030=CARTESIAN_POINT('Ctrl Pts',(1.22289832365684,2.98210545429801,-34.2035140689117));
#15031=CARTESIAN_POINT('Ctrl Pts',(1.09954829213986,3.03055020943928,-34.1951647056184));
#15032=CARTESIAN_POINT('Ctrl Pts',(1.01981364412113,3.0583033140502,-34.1897498793646));
#15033=CARTESIAN_POINT('Ctrl Pts',(0.829162615932968,3.1163779454646,-34.1767612468011));
#15034=CARTESIAN_POINT('Ctrl Pts',(0.717533976910228,3.14395667563413,-34.1691221166082));
#15035=CARTESIAN_POINT('Ctrl Pts',(0.40222596419993,3.20418703644321,-34.1475825410917));
#15036=CARTESIAN_POINT('Ctrl Pts',(0.196524080880937,3.22335002034519,-34.1335495640038));
#15037=CARTESIAN_POINT('Ctrl Pts',(-0.052682124323602,3.22260730248037,
-34.1173746297146));
#15038=CARTESIAN_POINT('Ctrl Pts',(-0.0957549019505773,3.22161522101677,
-34.1146102318553));
#15039=CARTESIAN_POINT('Ctrl Pts',(-0.16231880035045,3.21874579136757,-34.110399184628));
#15040=CARTESIAN_POINT('Ctrl Pts',(-0.185829663757392,3.2174740539212,-34.1089236108247));
#15041=CARTESIAN_POINT('Ctrl Pts',(-0.236461362457809,3.21417844340634,
-34.1057743210566));
#15042=CARTESIAN_POINT('Ctrl Pts',(-0.26357495516198,3.21206871083601,-34.1041053832965));
#15043=CARTESIAN_POINT('Ctrl Pts',(-0.339344344231211,3.20520710941833,
-34.099482596997));
#15044=CARTESIAN_POINT('Ctrl Pts',(-0.387925230829476,3.19969088509346,
-34.0965660987336));
#15045=CARTESIAN_POINT('Ctrl Pts',(-0.502188986630655,3.18407562230666,
-34.089779905838));
#15046=CARTESIAN_POINT('Ctrl Pts',(-0.56772303409955,3.17304629658005,-34.0859453745583));
#15047=CARTESIAN_POINT('Ctrl Pts',(-0.855798812563382,3.11535158528491,
-34.0691696744409));
#15048=CARTESIAN_POINT('Ctrl Pts',(-1.07337376811176,3.04724139140263,-34.0566663210387));
#15049=CARTESIAN_POINT('Ctrl Pts',(-1.36892210851935,2.91910105586133,-34.0381393677788));
#15050=CARTESIAN_POINT('Ctrl Pts',(-1.45415905513403,2.8775889106468,-34.0326061313529));
#15051=CARTESIAN_POINT('Ctrl Pts',(-1.58119510274997,2.80863283045792,-34.0239792737522));
#15052=CARTESIAN_POINT('Ctrl Pts',(-1.62439350654731,2.78387170367313,-34.0209756936361));
#15053=CARTESIAN_POINT('Ctrl Pts',(-1.70469883702285,2.73533542090594,-34.0152483054809));
#15054=CARTESIAN_POINT('Ctrl Pts',(-1.74192566316203,2.7117803522099,-34.0125327577926));
#15055=CARTESIAN_POINT('Ctrl Pts',(-1.82750560302044,2.65514072525237,-34.0061415400768));
#15056=CARTESIAN_POINT('Ctrl Pts',(-1.87546132461454,2.62148681582104,-34.0024457566313));
#15057=CARTESIAN_POINT('Ctrl Pts',(-2.080601206629,2.46901498075038,-33.9861170325249));
#15058=CARTESIAN_POINT('Ctrl Pts',(-2.22759875855569,2.33724623802432,-33.9730072397113));
#15059=CARTESIAN_POINT('Ctrl Pts',(-2.48438253152257,2.06070523692144,-33.9476082426829));
#15060=CARTESIAN_POINT('Ctrl Pts',(-2.59582690327688,1.91842473082648,-33.9353960022716));
#15061=CARTESIAN_POINT('Ctrl Pts',(-2.71712523652305,1.73349571666927,-33.9210757626383));
#15062=CARTESIAN_POINT('Ctrl Pts',(-2.73882054866971,1.69901127102594,-33.9184672845013));
#15063=CARTESIAN_POINT('Ctrl Pts',(-2.77300125182289,1.64232443867431,-33.914289962674));
#15064=CARTESIAN_POINT('Ctrl Pts',(-2.78588720453655,1.62036975938497,-33.9126984752009));
#15065=CARTESIAN_POINT('Ctrl Pts',(-2.8128363786728,1.57318252856204,-33.9093368337774));
#15066=CARTESIAN_POINT('Ctrl Pts',(-2.82682290460113,1.54790961139833,-33.9075710454565));
#15067=CARTESIAN_POINT('Ctrl Pts',(-2.86795106962706,1.47117594494492,-33.9023031580817));
#15068=CARTESIAN_POINT('Ctrl Pts',(-2.89404214267402,1.41916275888841,-33.8988571018703));
#15069=CARTESIAN_POINT('Ctrl Pts',(-2.95522847058906,1.28847165071172,-33.8904350533469));
#15070=CARTESIAN_POINT('Ctrl Pts',(-2.98860551890029,1.20903809799406,-33.8855220777578));
#15071=CARTESIAN_POINT('Ctrl Pts',(-3.10819065154371,0.889105337964295,
-33.8662019369981));
#15072=CARTESIAN_POINT('Ctrl Pts',(-3.16885482755945,0.640086550662371,
-33.8521041742066));
#15073=CARTESIAN_POINT('Ctrl Pts',(-3.20680935577038,0.325911580244707,
-33.8334735867785));
#15074=CARTESIAN_POINT('Ctrl Pts',(-3.21240728329331,0.265110069091308,
-33.8298347954596));
#15075=CARTESIAN_POINT('Ctrl Pts',(-3.21908421325108,0.15993865223235,-33.8234631443419));
#15076=CARTESIAN_POINT('Ctrl Pts',(-3.22097987681796,0.115636853831259,
-33.8207556495403));
#15077=CARTESIAN_POINT('Ctrl Pts',(-3.22303714865995,0.0226864077860033,
-33.8150192707975));
#15078=CARTESIAN_POINT('Ctrl Pts',(-3.22301242389749,-0.0259547603712082,
-33.8119854183815));
#15079=CARTESIAN_POINT('Ctrl Pts',(-3.21986202117663,-0.16206301649558,
-33.803399911913));
#15080=CARTESIAN_POINT('Ctrl Pts',(-3.2142745029355,-0.249425484656043,
-33.7977768863106));
#15081=CARTESIAN_POINT('Ctrl Pts',(-3.19241656248833,-0.457654033886757,
-33.7841069704923));
#15082=CARTESIAN_POINT('Ctrl Pts',(-3.17282901197651,-0.578033525436453,
-33.7759838996774));
#15083=CARTESIAN_POINT('Ctrl Pts',(-3.10258292516575,-0.895143215456569,
-33.7541575145555));
#15084=CARTESIAN_POINT('Ctrl Pts',(-3.04007265521266,-1.08870083126494,
-33.7403644121018));
#15085=CARTESIAN_POINT('Ctrl Pts',(-2.94453737792606,-1.31045766475141,
-33.7247686030642));
#15086=CARTESIAN_POINT('Ctrl Pts',(-2.92867229131383,-1.34554025187347,
-33.7223089290002));
#15087=CARTESIAN_POINT('Ctrl Pts',(-2.90131326193549,-1.4032614897725,-33.7182845471293));
#15088=CARTESIAN_POINT('Ctrl Pts',(-2.89017408583808,-1.42606289219463,
-33.7167009708395));
#15089=CARTESIAN_POINT('Ctrl Pts',(-2.86529347454357,-1.47550297645306,
-33.7132830934927));
#15090=CARTESIAN_POINT('Ctrl Pts',(-2.85144789365922,-1.50208548024471,
-33.7114547357917));
#15091=CARTESIAN_POINT('Ctrl Pts',(-2.80650730927186,-1.58550663512205,
-33.7057346359889));
#15092=CARTESIAN_POINT('Ctrl Pts',(-2.77406676565735,-1.64160570309285,
-33.7019141609664));
#15093=CARTESIAN_POINT('Ctrl Pts',(-2.68614632392249,-1.78358669658062,
-33.6922157819068));
#15094=CARTESIAN_POINT('Ctrl Pts',(-2.62823160448952,-1.8678769734824,-33.6864283693618));
#15095=CARTESIAN_POINT('Ctrl Pts',(-2.4270397116735,-2.13276511884671,-33.6676926112711));
#15096=CARTESIAN_POINT('Ctrl Pts',(-2.2684102164415,-2.30076402015599,-33.6548712654513));
#15097=CARTESIAN_POINT('Ctrl Pts',(-2.0471420065427,-2.48977932967462,-33.6377316381259));
#15098=CARTESIAN_POINT('Ctrl Pts',(-1.99995587692025,-2.52783846583439,
-33.6341175166604));
#15099=CARTESIAN_POINT('Ctrl Pts',(-1.91648719797233,-2.59136170038243,
-33.6277738680245));
#15100=CARTESIAN_POINT('Ctrl Pts',(-1.88069997615021,-2.61745027596987,
-33.6250690372428));
#15101=CARTESIAN_POINT('Ctrl Pts',(-1.80435382173455,-2.67073177051281,
-33.6193233923976));
#15102=CARTESIAN_POINT('Ctrl Pts',(-1.76369190480553,-2.6977567280764,-33.6162772918358));
#15103=CARTESIAN_POINT('Ctrl Pts',(-1.64751902048468,-2.77121904017934,
-33.607606639185));
#15104=CARTESIAN_POINT('Ctrl Pts',(-1.57068815370951,-2.81547692765836,
-33.6019083140625));
#15105=CARTESIAN_POINT('Ctrl Pts',(-1.38180571086802,-2.91414223076599,
-33.5879862187869));
#15106=CARTESIAN_POINT('Ctrl Pts',(-1.26823661294438,-2.96533027698748,
-33.5796820035108));
#15107=CARTESIAN_POINT('Ctrl Pts',(-0.967871025850895,-3.08029438539235,
-33.5580595436397));
#15108=CARTESIAN_POINT('Ctrl Pts',(-0.777653858128373,-3.13372799872132,
-33.5446731416994));
#15109=CARTESIAN_POINT('Ctrl Pts',(-0.545244104860971,-3.17653245338414,
-33.5293981784373));
#15110=CARTESIAN_POINT('Ctrl Pts',(-0.506622808517742,-3.182920546094,-33.5268957773784));
#15111=CARTESIAN_POINT('Ctrl Pts',(-0.442698106575825,-3.19230079895184,
-33.522823232662));
#15112=CARTESIAN_POINT('Ctrl Pts',(-0.417459350130495,-3.19569927649663,
-33.5212332291259));
#15113=CARTESIAN_POINT('Ctrl Pts',(-0.362735435088652,-3.20240856643265,
-33.517826954121));
#15114=CARTESIAN_POINT('Ctrl Pts',(-0.333240430192541,-3.20561204536868,
-33.5160160854558));
#15115=CARTESIAN_POINT('Ctrl Pts',(-0.241107852332009,-3.21433320843082,
-33.5104259638604));
#15116=CARTESIAN_POINT('Ctrl Pts',(-0.17834726898087,-3.21842574500099,
-33.5067134156217));
#15117=CARTESIAN_POINT('Ctrl Pts',(-0.0182121905898079,-3.22416866569615,
-33.497394937094));
#15118=CARTESIAN_POINT('Ctrl Pts',(0.0791922332697886,-3.2232477172368,
-33.4918707979789));
#15119=CARTESIAN_POINT('Ctrl Pts',(0.417629179523971,-3.20469421428213,
-33.4727600975917));
#15120=CARTESIAN_POINT('Ctrl Pts',(0.656576001985493,-3.16439225171484,
-33.4593506363506));
#15121=CARTESIAN_POINT('Ctrl Pts',(0.94565424611697,-3.08145381087424,-33.4416121788331));
#15122=CARTESIAN_POINT('Ctrl Pts',(1.00207374517393,-3.06357097315353,-33.4380792037024));
#15123=CARTESIAN_POINT('Ctrl Pts',(1.09963649348201,-3.02966388566108,-33.4318267754984));
#15124=CARTESIAN_POINT('Ctrl Pts',(1.14100304310047,-3.01432835661935,-33.4291298375298));
#15125=CARTESIAN_POINT('Ctrl Pts',(1.22807272407289,-2.98000055407047,-33.4233488529819));
#15126=CARTESIAN_POINT('Ctrl Pts',(1.27367895014745,-2.96079506688683,-33.4202583992583));
#15127=CARTESIAN_POINT('Ctrl Pts',(1.40349074996438,-2.90257503646365,-33.4112738339166));
#15128=CARTESIAN_POINT('Ctrl Pts',(1.48647173981525,-2.86096614691009,-33.4052967808635));
#15129=CARTESIAN_POINT('Ctrl Pts',(1.68509592767479,-2.75039495435885,-33.390411590174));
#15130=CARTESIAN_POINT('Ctrl Pts',(1.79843350213316,-2.67765806823329,-33.3814054518618));
#15131=CARTESIAN_POINT('Ctrl Pts',(2.03498792430055,-2.50403513889978,-33.3616524141691));
#15132=CARTESIAN_POINT('Ctrl Pts',(2.15594766665167,-2.40067646646913,-33.3509112477571));
#15133=CARTESIAN_POINT('Ctrl Pts',(2.26878022243767,-2.28883242391741,-33.3405291647262));
#15134=CARTESIAN_POINT('Origin',(0.,0.,-41.3107734492731));
#15135=CARTESIAN_POINT('',(2.26878017977789,-2.28883246620346,-31.8449383693487));
#15136=CARTESIAN_POINT('',(2.2687802230564,-2.28883242330411,-32.0941031001172));
#15137=CARTESIAN_POINT('',(2.26878020078428,-2.2888324453811,-41.3107734492731));
#15138=CARTESIAN_POINT('Ctrl Pts',(2.26878017977789,-2.28883246620346,-31.8449383693487));
#15139=CARTESIAN_POINT('Ctrl Pts',(2.25083588328518,-2.3066195540851,-31.846380501056));
#15140=CARTESIAN_POINT('Ctrl Pts',(2.23268039414462,-2.3241976195804,-31.8478279111245));
#15141=CARTESIAN_POINT('Ctrl Pts',(2.1462447988872,-2.40593611880222,-31.8546706275703));
#15142=CARTESIAN_POINT('Ctrl Pts',(2.07540247335777,-2.46730576859294,-31.8601415705246));
#15143=CARTESIAN_POINT('Ctrl Pts',(1.96325219349776,-2.55620855956848,-31.8686829425726));
#15144=CARTESIAN_POINT('Ctrl Pts',(1.92381287218028,-2.58602107719331,-31.871665215293));
#15145=CARTESIAN_POINT('Ctrl Pts',(1.84817462527405,-2.64050859320595,-31.8773549611355));
#15146=CARTESIAN_POINT('Ctrl Pts',(1.812127704753,-2.66537576456635,-31.8800543163724));
#15147=CARTESIAN_POINT('Ctrl Pts',(1.72782991028612,-2.72102850467852,-31.886344765084));
#15148=CARTESIAN_POINT('Ctrl Pts',(1.67924445321783,-2.7512778370562,-31.889954238958));
#15149=CARTESIAN_POINT('Ctrl Pts',(1.4128275107822,-2.90746285085639,-31.9096745557479));
#15150=CARTESIAN_POINT('Ctrl Pts',(1.18164818863494,-3.00883529266556,-31.9266293063323));
#15151=CARTESIAN_POINT('Ctrl Pts',(0.851284269751612,-3.10970237164751,
-31.9498862792296));
#15152=CARTESIAN_POINT('Ctrl Pts',(0.760322551787671,-3.13318447952589,
-31.9561826750656));
#15153=CARTESIAN_POINT('Ctrl Pts',(0.608364816766492,-3.16540420845404,
-31.9664119974058));
#15154=CARTESIAN_POINT('Ctrl Pts',(0.547911775597553,-3.17642649160067,
-31.9704069821587));
#15155=CARTESIAN_POINT('Ctrl Pts',(0.458194836643132,-3.19014649338539,
-31.9761923790283));
#15156=CARTESIAN_POINT('Ctrl Pts',(0.429152534537554,-3.19418305762291,
-31.9780431230572));
#15157=CARTESIAN_POINT('Ctrl Pts',(0.375078773353542,-3.20094786007096,
-31.9814431589607));
#15158=CARTESIAN_POINT('Ctrl Pts',(0.35006392680792,-3.20378004332276,-31.9829973620236));
#15159=CARTESIAN_POINT('Ctrl Pts',(0.286117003506866,-3.21026220754779,
-31.986927542094));
#15160=CARTESIAN_POINT('Ctrl Pts',(0.247145756334189,-3.21349741867446,
-31.989282537349));
#15161=CARTESIAN_POINT('Ctrl Pts',(0.0108207900656008,-3.22879107716611,
-32.003371646215));
#15162=CARTESIAN_POINT('Ctrl Pts',(-0.18726055140136,-3.22337705591122,
-32.0143908945148));
#15163=CARTESIAN_POINT('Ctrl Pts',(-0.507096719864957,-3.18503339747847,
-32.0325030121935));
#15164=CARTESIAN_POINT('Ctrl Pts',(-0.629614834490448,-3.16309464160002,
-32.0395157929653));
#15165=CARTESIAN_POINT('Ctrl Pts',(-0.836762037811956,-3.11348758835781,
-32.0518072842348));
#15166=CARTESIAN_POINT('Ctrl Pts',(-0.922076070187199,-3.08929595876016,
-32.0569990088072));
#15167=CARTESIAN_POINT('Ctrl Pts',(-1.05272490635079,-3.04635487102285,
-32.0652205457101));
#15168=CARTESIAN_POINT('Ctrl Pts',(-1.09881450676877,-3.03003531753112,
-32.0681744142687));
#15169=CARTESIAN_POINT('Ctrl Pts',(-1.18601302635277,-2.99690864860922,
-32.0738752365067));
#15170=CARTESIAN_POINT('Ctrl Pts',(-1.22718085794768,-2.9802877691009,-32.0766156151959));
#15171=CARTESIAN_POINT('Ctrl Pts',(-1.323948884494,-2.93887423123703,-32.0831797393906));
#15172=CARTESIAN_POINT('Ctrl Pts',(-1.37921417656479,-2.91334685140059,
-32.0870268690308));
#15173=CARTESIAN_POINT('Ctrl Pts',(-1.6626232612589,-2.7725667718116,-32.1072857019854));
#15174=CARTESIAN_POINT('Ctrl Pts',(-1.87715825308495,-2.63204874213256,
-32.1245463100748));
#15175=CARTESIAN_POINT('Ctrl Pts',(-2.13834646174866,-2.4126578648444,-32.1474542580902));
#15176=CARTESIAN_POINT('Ctrl Pts',(-2.20166970063346,-2.35501496362171,
-32.1531719569035));
#15177=CARTESIAN_POINT('Ctrl Pts',(-2.30389382249911,-2.25422922051474,
-32.1625973402715));
#15178=CARTESIAN_POINT('Ctrl Pts',(-2.3440599041077,-2.21243308489319,-32.1663559011371));
#15179=CARTESIAN_POINT('Ctrl Pts',(-2.40253355258328,-2.14820510720482,
-32.1718835959574));
#15180=CARTESIAN_POINT('Ctrl Pts',(-2.42170034524762,-2.12657476499325,
-32.1737050229972));
#15181=CARTESIAN_POINT('Ctrl Pts',(-2.4572556922702,-2.08534516621055,-32.1770973021609));
#15182=CARTESIAN_POINT('Ctrl Pts',(-2.47370644362626,-2.06580407155842,
-32.1786719965604));
#15183=CARTESIAN_POINT('Ctrl Pts',(-2.51600693232524,-2.01432732049326,
-32.1827399623243));
#15184=CARTESIAN_POINT('Ctrl Pts',(-2.54148230592145,-1.98208815951638,
-32.1852091812825));
#15185=CARTESIAN_POINT('Ctrl Pts',(-2.69704990466933,-1.77728412314121,
-32.2004726696924));
#15186=CARTESIAN_POINT('Ctrl Pts',(-2.81013855576133,-1.59246938591455,
-32.2124346304722));
#15187=CARTESIAN_POINT('Ctrl Pts',(-2.95219312378926,-1.29733639368063,
-32.230887026916));
#15188=CARTESIAN_POINT('Ctrl Pts',(-2.99526577543067,-1.19453206597594,
-32.2372009879123));
#15189=CARTESIAN_POINT('Ctrl Pts',(-3.06091380635784,-1.01181742644336,
-32.2484432786366));
#15190=CARTESIAN_POINT('Ctrl Pts',(-3.08588683134635,-0.932881949061886,
-32.2533057073726));
#15191=CARTESIAN_POINT('Ctrl Pts',(-3.1204625871208,-0.806921118863847,
-32.2611283657312));
#15192=CARTESIAN_POINT('Ctrl Pts',(-3.13210186047686,-0.760490646535977,
-32.2640249262468));
#15193=CARTESIAN_POINT('Ctrl Pts',(-3.15259132338029,-0.670282626630437,
-32.2696863776339));
#15194=CARTESIAN_POINT('Ctrl Pts',(-3.16157401945455,-0.626546297592554,
-32.2724464079597));
#15195=CARTESIAN_POINT('Ctrl Pts',(-3.1792506354493,-0.530382830994488,
-32.2785531588805));
#15196=CARTESIAN_POINT('Ctrl Pts',(-3.18756208361038,-0.477899567372165,
-32.2819107512426));
#15197=CARTESIAN_POINT('Ctrl Pts',(-3.22975530768901,-0.16092515098102,
-32.3023473661338));
#15198=CARTESIAN_POINT('Ctrl Pts',(-3.23199421620793,0.106698558096767,
-32.320385288323));
#15199=CARTESIAN_POINT('Ctrl Pts',(-3.19173000777098,0.453679046004111,
-32.3438423296109));
#15200=CARTESIAN_POINT('Ctrl Pts',(-3.17902872457724,0.535483718605843,
-32.3493667979328));
#15201=CARTESIAN_POINT('Ctrl Pts',(-3.15234404317121,0.672352681006745,
-32.358518118322));
#15202=CARTESIAN_POINT('Ctrl Pts',(-3.14002920181656,0.727700850441106,
-32.3621928105448));
#15203=CARTESIAN_POINT('Ctrl Pts',(-3.11930831632351,0.810464340586884,
-32.3676210694632));
#15204=CARTESIAN_POINT('Ctrl Pts',(-3.11198693902731,0.838137367822374,
-32.3694246973641));
#15205=CARTESIAN_POINT('Ctrl Pts',(-3.0974336889949,0.890322975649689,-32.3727996731793));
#15206=CARTESIAN_POINT('Ctrl Pts',(-3.09027734962206,0.914853209685398,
-32.374374525629));
#15207=CARTESIAN_POINT('Ctrl Pts',(-3.07076554150476,0.978892197073889,
-32.3784609029816));
#15208=CARTESIAN_POINT('Ctrl Pts',(-3.05793885156614,1.01825403401639,-32.3809477652685));
#15209=CARTESIAN_POINT('Ctrl Pts',(-2.97412251692548,1.25957853082372,-32.3961021176234));
#15210=CARTESIAN_POINT('Ctrl Pts',(-2.88390729941012,1.4543181869831,-32.4079553553971));
#15211=CARTESIAN_POINT('Ctrl Pts',(-2.71795552466129,1.73534922344312,-32.4263353282678));
#15212=CARTESIAN_POINT('Ctrl Pts',(-2.65586674929463,1.82895842259242,-32.4326949003001));
#15213=CARTESIAN_POINT('Ctrl Pts',(-2.53950015327866,1.98594378806094,-32.4440059698837));
#15214=CARTESIAN_POINT('Ctrl Pts',(-2.48741230417156,2.05080769402615,-32.4488901444259));
#15215=CARTESIAN_POINT('Ctrl Pts',(-2.40146485775406,2.14973910505034,-32.4567369407344));
#15216=CARTESIAN_POINT('Ctrl Pts',(-2.36925167340508,2.18519057020091,-32.4596349736365));
#15217=CARTESIAN_POINT('Ctrl Pts',(-2.30556673476992,2.25221342335293,-32.4652922884253));
#15218=CARTESIAN_POINT('Ctrl Pts',(-2.27420637256636,2.28387572801475,-32.4680465549153));
#15219=CARTESIAN_POINT('Ctrl Pts',(-2.19703467369579,2.35862461684478,-32.4747555442305));
#15220=CARTESIAN_POINT('Ctrl Pts',(-2.15060051292473,2.40103894595991,-32.4787369330605));
#15221=CARTESIAN_POINT('Ctrl Pts',(-1.91778021712075,2.60152956111959,-32.4984483604495));
#15222=CARTESIAN_POINT('Ctrl Pts',(-1.71508782504844,2.73939352585008,-32.5149364938315));
#15223=CARTESIAN_POINT('Ctrl Pts',(-1.41888633657627,2.89500083990007,-32.5374379689575));
#15224=CARTESIAN_POINT('Ctrl Pts',(-1.33722970849517,2.9336132194913,-32.5434815765863));
#15225=CARTESIAN_POINT('Ctrl Pts',(-1.19882303832718,2.99207886570611,-32.553362667385));
#15226=CARTESIAN_POINT('Ctrl Pts',(-1.14294581035873,3.01386602881807,-32.5572571042036));
#15227=CARTESIAN_POINT('Ctrl Pts',(-1.05902494929008,3.04391766645125,-32.5629351043087));
#15228=CARTESIAN_POINT('Ctrl Pts',(-1.03142672873532,3.05337970942992,-32.5647753963254));
#15229=CARTESIAN_POINT('Ctrl Pts',(-0.979633077398192,3.07035473088118,
-32.5681740253747));
#15230=CARTESIAN_POINT('Ctrl Pts',(-0.95547140880725,3.07795931697447,-32.5697368457888));
#15231=CARTESIAN_POINT('Ctrl Pts',(-0.892990635504107,3.09681773332658,
-32.5737249626882));
#15232=CARTESIAN_POINT('Ctrl Pts',(-0.854546221334146,3.10764596204018,
-32.5761279967936));
#15233=CARTESIAN_POINT('Ctrl Pts',(-0.632208441644363,3.16583115169922,
-32.5897863116035));
#15234=CARTESIAN_POINT('Ctrl Pts',(-0.444598695442307,3.19758061653721,
-32.6003916737218));
#15235=CARTESIAN_POINT('Ctrl Pts',(-0.0649455071326363,3.22774707530151,
-32.6218006860141));
#15236=CARTESIAN_POINT('Ctrl Pts',(0.126326062762748,3.22592644778593,-32.6325712379312));
#15237=CARTESIAN_POINT('Ctrl Pts',(0.373914219011914,3.20150856486668,-32.6472656260573));
#15238=CARTESIAN_POINT('Ctrl Pts',(0.431359353452693,3.19427572950281,-32.6507259395644));
#15239=CARTESIAN_POINT('Ctrl Pts',(0.532062040695091,3.17883045479747,-32.65689877275));
#15240=CARTESIAN_POINT('Ctrl Pts',(0.575405130293294,3.1712713099674,-32.6595907303629));
#15241=CARTESIAN_POINT('Ctrl Pts',(0.667839695784798,3.15319317610403,-32.6654132797304));
#15242=CARTESIAN_POINT('Ctrl Pts',(0.716866930620908,3.14240965325868,-32.6685514190392));
#15243=CARTESIAN_POINT('Ctrl Pts',(0.860223985671916,3.10734894106575,-32.6778817680555));
#15244=CARTESIAN_POINT('Ctrl Pts',(0.953721948456661,3.07993737187872,-32.6841675482006));
#15245=CARTESIAN_POINT('Ctrl Pts',(1.25753677142511,2.97570407620439,-32.7052479952225));
#15246=CARTESIAN_POINT('Ctrl Pts',(1.46109355801271,2.88121572739542,-32.7204858707239));
#15247=CARTESIAN_POINT('Ctrl Pts',(1.70991249643382,2.73252314307851,-32.7398416925248));
#15248=CARTESIAN_POINT('Ctrl Pts',(1.76557861967916,2.69689014960709,-32.7442192928158));
#15249=CARTESIAN_POINT('Ctrl Pts',(1.86030349849153,2.63206389133094,-32.7517068566758));
#15250=CARTESIAN_POINT('Ctrl Pts',(1.89986839864351,2.6036493726888,-32.7548464265614));
#15251=CARTESIAN_POINT('Ctrl Pts',(1.96047663790549,2.55800447872138,-32.759656904073));
#15252=CARTESIAN_POINT('Ctrl Pts',(1.98197043911462,2.54138719175909,-32.7613630679379));
#15253=CARTESIAN_POINT('Ctrl Pts',(2.02171898741522,2.5098457412055,-32.7645146925915));
#15254=CARTESIAN_POINT('Ctrl Pts',(2.04002481606516,2.49498940431175,-32.7659646274535));
#15255=CARTESIAN_POINT('Ctrl Pts',(2.09144683894697,2.45231281432277,-32.7700385020309));
#15256=CARTESIAN_POINT('Ctrl Pts',(2.1241695562899,2.42402395033417,-32.7726320685745));
#15257=CARTESIAN_POINT('Ctrl Pts',(2.3093308273636,2.25732164070832,-32.7873801495241));
#15258=CARTESIAN_POINT('Ctrl Pts',(2.44880886121207,2.10519891532581,-32.7988028289234));
#15259=CARTESIAN_POINT('Ctrl Pts',(2.64198066892902,1.84911926120305,-32.8168601661398));
#15260=CARTESIAN_POINT('Ctrl Pts',(2.70618217865005,1.75381863327001,-32.8233591362569));
#15261=CARTESIAN_POINT('Ctrl Pts',(2.80848998372138,1.58291464189368,-32.8348810773274));
#15262=CARTESIAN_POINT('Ctrl Pts',(2.84895971447847,1.50886104377346,-32.8398327684402));
#15263=CARTESIAN_POINT('Ctrl Pts',(2.9078768313499,1.39021055643107,-32.8477620609976));
#15264=CARTESIAN_POINT('Ctrl Pts',(2.92830902276181,1.34663987670954,-32.8506726733008));
#15265=CARTESIAN_POINT('Ctrl Pts',(2.96575238062977,1.26190825397263,-32.8563396253359));
#15266=CARTESIAN_POINT('Ctrl Pts',(2.98290094548011,1.22081991648424,-32.8590905975815));
#15267=CARTESIAN_POINT('Ctrl Pts',(3.02202884611609,1.12131763936864,-32.865765279464));
#15268=CARTESIAN_POINT('Ctrl Pts',(3.04317256965212,1.06259657036668,-32.8697148678552));
#15269=CARTESIAN_POINT('Ctrl Pts',(3.10872802721022,0.862487310983578,-32.8832177932101));
#15270=CARTESIAN_POINT('Ctrl Pts',(3.14508697658735,0.718674708985431,-32.8930043191624));
#15271=CARTESIAN_POINT('Ctrl Pts',(3.19518631999257,0.441331320160369,-32.9118889058492));
#15272=CARTESIAN_POINT('Ctrl Pts',(3.21074159277277,0.308426797108418,-32.9209404836845));
#15273=CARTESIAN_POINT('Ctrl Pts',(3.22175127287199,0.105906404441358,-32.9345021426273));
#15274=CARTESIAN_POINT('Ctrl Pts',(3.22328197619651,0.0367652693626423,
-32.9390900708907));
#15275=CARTESIAN_POINT('Ctrl Pts',(3.22208264448847,-0.0826164956901453,
-32.9468880662188));
#15276=CARTESIAN_POINT('Ctrl Pts',(3.22040299919485,-0.132842677331466,
-32.9501308794266));
#15277=CARTESIAN_POINT('Ctrl Pts',(3.21599056982555,-0.210418022095615,
-32.9550610040053));
#15278=CARTESIAN_POINT('Ctrl Pts',(3.21408157120335,-0.237804258152322,
-32.9567862952362));
#15279=CARTESIAN_POINT('Ctrl Pts',(3.20989823803415,-0.288475287034926,
-32.959946299043));
#15280=CARTESIAN_POINT('Ctrl Pts',(3.20771989716076,-0.31176562337916,-32.9613859789023));
#15281=CARTESIAN_POINT('Ctrl Pts',(3.20090857459537,-0.376930539533431,
-32.9653833164193));
#15282=CARTESIAN_POINT('Ctrl Pts',(3.19570764009236,-0.418742621981689,
-32.9679124801845));
#15283=CARTESIAN_POINT('Ctrl Pts',(3.15978957037525,-0.667562742506565,
-32.9828129972776));
#15284=CARTESIAN_POINT('Ctrl Pts',(3.1097853410238,-0.871300080003428,-32.9944154238782));
#15285=CARTESIAN_POINT('Ctrl Pts',(3.00251751658217,-1.17645011977741,-33.012625793801));
#15286=CARTESIAN_POINT('Ctrl Pts',(2.95897130873465,-1.28204251690308,-33.0190875279521));
#15287=CARTESIAN_POINT('Ctrl Pts',(2.87379517307445,-1.46098694633041,-33.030553400946));
#15288=CARTESIAN_POINT('Ctrl Pts',(2.83472010025197,-1.53542888959496,-33.0354873333003));
#15289=CARTESIAN_POINT('Ctrl Pts',(2.76879687369862,-1.64990654963131,-33.0433951230423));
#15290=CARTESIAN_POINT('Ctrl Pts',(2.74388342933559,-1.69101481674904,-33.0463026344805));
#15291=CARTESIAN_POINT('Ctrl Pts',(2.694132227438,-1.76911067071832,-33.0519675656619));
#15292=CARTESIAN_POINT('Ctrl Pts',(2.66942841901444,-1.80617071007457,-33.0547197124503));
#15293=CARTESIAN_POINT('Ctrl Pts',(2.60820717319357,-1.89401266655825,-33.0614044034138));
#15294=CARTESIAN_POINT('Ctrl Pts',(2.57096504606206,-1.94426503617086,-33.0653630417495));
#15295=CARTESIAN_POINT('Ctrl Pts',(2.45056934212156,-2.09720798546166,-33.0778461096972));
#15296=CARTESIAN_POINT('Ctrl Pts',(2.36256546156562,-2.19586883031866,-33.0865427928208));
#15297=CARTESIAN_POINT('Ctrl Pts',(2.26878017716708,-2.2888324687914,-33.0953665650246));
#15298=CARTESIAN_POINT('Ctrl Pts',(2.26878022243768,-2.28883242391741,-33.3405291647262));
#15299=CARTESIAN_POINT('Ctrl Pts',(2.2815974322282,-2.27612750424933,-33.3393498124077));
#15300=CARTESIAN_POINT('Ctrl Pts',(2.29430977757391,-2.26331308373006,-33.3381752501945));
#15301=CARTESIAN_POINT('Ctrl Pts',(2.33543620901607,-2.22115363659044,-33.334361238633));
#15302=CARTESIAN_POINT('Ctrl Pts',(2.36339974731244,-2.19137576576757,-33.3317455726527));
#15303=CARTESIAN_POINT('Ctrl Pts',(2.40787166087554,-2.1421765670001,-33.3275600333921));
#15304=CARTESIAN_POINT('Ctrl Pts',(2.424728572414,-2.12307745939442,-33.3259673477335));
#15305=CARTESIAN_POINT('Ctrl Pts',(2.46018622729106,-2.08193014870757,-33.3226069194139));
#15306=CARTESIAN_POINT('Ctrl Pts',(2.47872055074316,-2.05982863014307,-33.3208434672996));
#15307=CARTESIAN_POINT('Ctrl Pts',(2.5335875716952,-1.99258844351747,-33.31559178847));
#15308=CARTESIAN_POINT('Ctrl Pts',(2.56900379044949,-1.9467139146164,-33.3121590930041));
#15309=CARTESIAN_POINT('Ctrl Pts',(2.65362054990467,-1.83077586405287,-33.30378054767));
#15310=CARTESIAN_POINT('Ctrl Pts',(2.70130415338509,-1.75965897275495,-33.2988968671888));
#15311=CARTESIAN_POINT('Ctrl Pts',(2.88056244141489,-1.46781433037686,-33.2795193884745));
#15312=CARTESIAN_POINT('Ctrl Pts',(2.98835648675837,-1.23362830000713,-33.2653442274646));
#15313=CARTESIAN_POINT('Ctrl Pts',(3.08586548324229,-0.931261988041518,
-33.2466361085819));
#15314=CARTESIAN_POINT('Ctrl Pts',(3.10288507312785,-0.87287925949752,-33.2430112044922));
#15315=CARTESIAN_POINT('Ctrl Pts',(3.12943437333506,-0.771181718808912,
-33.2366553495684));
#15316=CARTESIAN_POINT('Ctrl Pts',(3.13974057372274,-0.728086241477337,
-33.2339493876052));
#15317=CARTESIAN_POINT('Ctrl Pts',(3.15951093839578,-0.637168421462377,
-33.2282079333869));
#15318=CARTESIAN_POINT('Ctrl Pts',(3.16878501068295,-0.589316655256495,
-33.2251672953158));
#15319=CARTESIAN_POINT('Ctrl Pts',(3.19177271721751,-0.454392146050003,
-33.2165346005326));
#15320=CARTESIAN_POINT('Ctrl Pts',(3.20300388944414,-0.366945685563639,
-33.2108698443246));
#15321=CARTESIAN_POINT('Ctrl Pts',(3.22131818113831,-0.156307985165885,
-33.1970605566852));
#15322=CARTESIAN_POINT('Ctrl Pts',(3.22493916864179,-0.0329582027652135,
-33.1888375032897));
#15323=CARTESIAN_POINT('Ctrl Pts',(3.2158892792051,0.289946190392386,-33.1671241262386));
#15324=CARTESIAN_POINT('Ctrl Pts',(3.19174408638474,0.488662767621672,-33.1535562716225));
#15325=CARTESIAN_POINT('Ctrl Pts',(3.14110992853273,0.721841778671662,-33.1381380285115));
#15326=CARTESIAN_POINT('Ctrl Pts',(3.13217883163252,0.759659929697509,-33.1356547407048));
#15327=CARTESIAN_POINT('Ctrl Pts',(3.11627577706345,0.8219423327106,-33.131603796716));
#15328=CARTESIAN_POINT('Ctrl Pts',(3.10969447453718,0.846501246732696,-33.1300167238944));
#15329=CARTESIAN_POINT('Ctrl Pts',(3.09476944567145,0.899670800413077,-33.1266055425404));
#15330=CARTESIAN_POINT('Ctrl Pts',(3.08631843840116,0.928247874742262,-33.124787073679));
#15331=CARTESIAN_POINT('Ctrl Pts',(3.0585616381,1.0175343225671,-33.1191407200418));
#15332=CARTESIAN_POINT('Ctrl Pts',(3.0378506618822,1.07779396780705,-33.1153814975561));
#15333=CARTESIAN_POINT('Ctrl Pts',(2.98027419515235,1.23043464517424,-33.1059000114187));
#15334=CARTESIAN_POINT('Ctrl Pts',(2.94089431022154,1.32179666326859,-33.1002632209355));
#15335=CARTESIAN_POINT('Ctrl Pts',(2.79369608742939,1.62401196210732,-33.0813185043216));
#15336=CARTESIAN_POINT('Ctrl Pts',(2.66691941525258,1.82474236356701,-33.0681649119777));
#15337=CARTESIAN_POINT('Ctrl Pts',(2.48200555414001,2.05653692367404,-33.0506870742025));
#15338=CARTESIAN_POINT('Ctrl Pts',(2.44340934727261,2.10224779426727,-33.047117928724));
#15339=CARTESIAN_POINT('Ctrl Pts',(2.37412946475749,2.17981177645596,-33.0408250318442));
#15340=CARTESIAN_POINT('Ctrl Pts',(2.3440201885715,2.21215712792206,-33.0381247651418));
#15341=CARTESIAN_POINT('Ctrl Pts',(2.27901920673361,2.27916805398083,-33.0323605564128));
#15342=CARTESIAN_POINT('Ctrl Pts',(2.24398012566538,2.31367420883668,-33.029290722216));
#15343=CARTESIAN_POINT('Ctrl Pts',(2.14199860597922,2.40960829487838,-33.020453173));
#15344=CARTESIAN_POINT('Ctrl Pts',(2.07323366333846,2.46902205143278,-33.0146068720087));
#15345=CARTESIAN_POINT('Ctrl Pts',(1.90039199017234,2.60604277202085,-33.0001794937773));
#15346=CARTESIAN_POINT('Ctrl Pts',(1.7939612724467,2.68041918950734,-32.9915090151857));
#15347=CARTESIAN_POINT('Ctrl Pts',(1.52481879398387,2.84527768743866,-32.9702734009079));
#15348=CARTESIAN_POINT('Ctrl Pts',(1.358177791081,2.92848748170027,-32.9576759668926));
#15349=CARTESIAN_POINT('Ctrl Pts',(1.14778115879816,3.01170091910822,-32.943032277101));
#15350=CARTESIAN_POINT('Ctrl Pts',(1.11000142506506,3.02582900842403,-32.9404508320781));
#15351=CARTESIAN_POINT('Ctrl Pts',(1.04801880832871,3.04769074400936,-32.9363043321251));
#15352=CARTESIAN_POINT('Ctrl Pts',(1.02397285787188,3.05585373487842,-32.9347172674222));
#15353=CARTESIAN_POINT('Ctrl Pts',(0.972222598731633,3.07274212763279,-32.9313506132433));
#15354=CARTESIAN_POINT('Ctrl Pts',(0.944492511835474,3.08137874970391,-32.9295756795287));
#15355=CARTESIAN_POINT('Ctrl Pts',(0.859989506013474,3.10644948513728,-32.9242441493829));
#15356=CARTESIAN_POINT('Ctrl Pts',(0.802875295836612,3.12169865785259,-32.9207456223695));
#15357=CARTESIAN_POINT('Ctrl Pts',(0.65950989410396,3.15578087598898,-32.912151462353));
#15358=CARTESIAN_POINT('Ctrl Pts',(0.572842375995145,3.17265811121929,-32.9071222517133));
#15359=CARTESIAN_POINT('Ctrl Pts',(0.238846222655787,3.22356409536986,-32.8880248769923));
#15360=CARTESIAN_POINT('Ctrl Pts',(-0.0114100151469539,3.23237942279218,
-32.8742312969334));
#15361=CARTESIAN_POINT('Ctrl Pts',(-0.321982003329754,3.20722473081007,
-32.855904270197));
#15362=CARTESIAN_POINT('Ctrl Pts',(-0.38362967329787,3.20043597470433,-32.8522111359217));
#15363=CARTESIAN_POINT('Ctrl Pts',(-0.489082500146419,3.18573277076142,
-32.8457773211945));
#15364=CARTESIAN_POINT('Ctrl Pts',(-0.532991024301267,3.17868136950936,
-32.8430634853532));
#15365=CARTESIAN_POINT('Ctrl Pts',(-0.624224832187557,3.16208642000774,
-32.837345072925));
#15366=CARTESIAN_POINT('Ctrl Pts',(-0.671509481383014,3.15238350993329,
-32.834336193556));
#15367=CARTESIAN_POINT('Ctrl Pts',(-0.801650372699304,3.12261749750859,
-32.8259229835529));
#15368=CARTESIAN_POINT('Ctrl Pts',(-0.883951024262481,3.10032448249165,
-32.8204520388855));
#15369=CARTESIAN_POINT('Ctrl Pts',(-1.07665938532853,3.03982787306527,-32.8072821242616));
#15370=CARTESIAN_POINT('Ctrl Pts',(-1.18606212424275,2.99883342109459,-32.7995150399525));
#15371=CARTESIAN_POINT('Ctrl Pts',(-1.4868604540302,2.86708196989205,-32.7774708454677));
#15372=CARTESIAN_POINT('Ctrl Pts',(-1.67189970196541,2.76327216693552,-32.7630597475327));
#15373=CARTESIAN_POINT('Ctrl Pts',(-1.87708164520897,2.61995660934746,-32.7468923892728));
#15374=CARTESIAN_POINT('Ctrl Pts',(-1.90833490544678,2.59728056373657,-32.7444254118261));
#15375=CARTESIAN_POINT('Ctrl Pts',(-1.95945363087026,2.55876995148225,-32.7403928379803));
#15376=CARTESIAN_POINT('Ctrl Pts',(-1.97955219478087,2.54325293108103,-32.738808203014));
#15377=CARTESIAN_POINT('Ctrl Pts',(-2.02292719340222,2.50893960604838,-32.7353926002089));
#15378=CARTESIAN_POINT('Ctrl Pts',(-2.04612879794041,2.49005410976413,-32.7335674784356));
#15379=CARTESIAN_POINT('Ctrl Pts',(-2.11846848759079,2.42947751712734,-32.7278710792597));
#15380=CARTESIAN_POINT('Ctrl Pts',(-2.16662347248104,2.3866322694978,-32.7240702372045));
#15381=CARTESIAN_POINT('Ctrl Pts',(-2.28710011035673,2.2727856743607,-32.7144416410786));
#15382=CARTESIAN_POINT('Ctrl Pts',(-2.3574176992672,2.19976488968956,-32.7087027598979));
#15383=CARTESIAN_POINT('Ctrl Pts',(-2.57733014835126,1.94871930176628,-32.6899013367315));
#15384=CARTESIAN_POINT('Ctrl Pts',(-2.71110468455041,1.75785100827698,-32.6769742390252));
#15385=CARTESIAN_POINT('Ctrl Pts',(-2.85229916113503,1.50138292843653,-32.6597270239733));
#15386=CARTESIAN_POINT('Ctrl Pts',(-2.87991784346774,1.44769946412563,-32.6561270870826));
#15387=CARTESIAN_POINT('Ctrl Pts',(-2.92514201908039,1.35337348664802,-32.6497996798029));
#15388=CARTESIAN_POINT('Ctrl Pts',(-2.94344780861348,1.31308428135173,-32.6470965288372));
#15389=CARTESIAN_POINT('Ctrl Pts',(-2.98023303065432,1.22748601163033,-32.6413459165926));
#15390=CARTESIAN_POINT('Ctrl Pts',(-2.99852161134579,1.1821076788523,-32.6382929867005));
#15391=CARTESIAN_POINT('Ctrl Pts',(-3.04725003618361,1.05278488299647,-32.6295736237474));
#15392=CARTESIAN_POINT('Ctrl Pts',(-3.07524255259424,0.967971953567275,
-32.6238320127503));
#15393=CARTESIAN_POINT('Ctrl Pts',(-3.13416365658659,0.760927611098515,
-32.6097633118767));
#15394=CARTESIAN_POINT('Ctrl Pts',(-3.16151179436378,0.637833457108885,
-32.6013532233444));
#15395=CARTESIAN_POINT('Ctrl Pts',(-3.212465236872,0.322109630769983,-32.57984681089));
#15396=CARTESIAN_POINT('Ctrl Pts',(-3.22602271593976,0.128349844134028,
-32.5666937389803));
#15397=CARTESIAN_POINT('Ctrl Pts',(-3.22128256542905,-0.104962294955333,
-32.5516036674606));
#15398=CARTESIAN_POINT('Ctrl Pts',(-3.21975372826244,-0.144446178298068,
-32.5490768268331));
#15399=CARTESIAN_POINT('Ctrl Pts',(-3.21605741476315,-0.209118714780682,
-32.5449924904373));
#15400=CARTESIAN_POINT('Ctrl Pts',(-3.21431905868137,-0.234326882862213,
-32.543414254866));
#15401=CARTESIAN_POINT('Ctrl Pts',(-3.20991898652324,-0.288791292684576,
-32.5400367778838));
#15402=CARTESIAN_POINT('Ctrl Pts',(-3.20715349735872,-0.318036002562597,
-32.5382427985214));
#15403=CARTESIAN_POINT('Ctrl Pts',(-3.19740645270749,-0.407972118388398,
-32.5327750166298));
#15404=CARTESIAN_POINT('Ctrl Pts',(-3.18909857162773,-0.468508859145859,
-32.5291637721633));
#15405=CARTESIAN_POINT('Ctrl Pts',(-3.16382118005518,-0.620479850239381,
-32.5201928028806));
#15406=CARTESIAN_POINT('Ctrl Pts',(-3.14460654418237,-0.711485210831207,
-32.5149073068681));
#15407=CARTESIAN_POINT('Ctrl Pts',(-3.05870670186714,-1.04601126980313,
-32.4954124982467));
#15408=CARTESIAN_POINT('Ctrl Pts',(-2.96743453887896,-1.28224413779704,
-32.4814360873824));
#15409=CARTESIAN_POINT('Ctrl Pts',(-2.82286436611143,-1.55589693967944,
-32.463153272247));
#15410=CARTESIAN_POINT('Ctrl Pts',(-2.79485369377115,-1.60566832335914,
-32.4597398967317));
#15411=CARTESIAN_POINT('Ctrl Pts',(-2.74294386451853,-1.69242809094574,
-32.4536151884451));
#15412=CARTESIAN_POINT('Ctrl Pts',(-2.71958079605436,-1.72972075503202,
-32.4509231221459));
#15413=CARTESIAN_POINT('Ctrl Pts',(-2.66803393858905,-1.80837395621602,
-32.4451105685868));
#15414=CARTESIAN_POINT('Ctrl Pts',(-2.63963577296326,-1.84957941516449,
-32.4419827600668));
#15415=CARTESIAN_POINT('Ctrl Pts',(-2.55374237163742,-1.9682007271315,-32.4327257345505));
#15416=CARTESIAN_POINT('Ctrl Pts',(-2.49372243359689,-2.04371224273494,
-32.4265052067696));
#15417=CARTESIAN_POINT('Ctrl Pts',(-2.33585429497226,-2.22500221416585,
-32.410735245973));
#15418=CARTESIAN_POINT('Ctrl Pts',(-2.2341311116399,-2.32712328416571,-32.4010698372943));
#15419=CARTESIAN_POINT('Ctrl Pts',(-2.00651131109712,-2.52691058902443,
-32.3806714397064));
#15420=CARTESIAN_POINT('Ctrl Pts',(-1.87949660575656,-2.62275886816318,
-32.369958240645));
#15421=CARTESIAN_POINT('Ctrl Pts',(-1.71032621107988,-2.73179340987916,
-32.3569046598221));
#15422=CARTESIAN_POINT('Ctrl Pts',(-1.6742796409564,-2.7540332332896,-32.3541888181361));
#15423=CARTESIAN_POINT('Ctrl Pts',(-1.61762499048443,-2.78746406087564,
-32.3500330044091));
#15424=CARTESIAN_POINT('Ctrl Pts',(-1.59731651132404,-2.79915104320127,
-32.3485652643575));
#15425=CARTESIAN_POINT('Ctrl Pts',(-1.55297764875523,-2.82402713061975,
-32.3454110684784));
#15426=CARTESIAN_POINT('Ctrl Pts',(-1.5289027696891,-2.83713328085056,-32.3437297535109));
#15427=CARTESIAN_POINT('Ctrl Pts',(-1.46046516621276,-2.87326590960952,
-32.3390298794213));
#15428=CARTESIAN_POINT('Ctrl Pts',(-1.41572823777866,-2.89557069069907,
-32.3360506831119));
#15429=CARTESIAN_POINT('Ctrl Pts',(-1.14203251646074,-3.02416820933234,
-32.3182744569069));
#15430=CARTESIAN_POINT('Ctrl Pts',(-0.9017390025095,-3.10430711995979,-32.3044831216224));
#15431=CARTESIAN_POINT('Ctrl Pts',(-0.537303710116642,-3.17989890461302,
-32.2833161060094));
#15432=CARTESIAN_POINT('Ctrl Pts',(-0.418816860247447,-3.19766179005776,
-32.2764081120268));
#15433=CARTESIAN_POINT('Ctrl Pts',(-0.245576636569195,-3.21383823689162,
-32.2660884180779));
#15434=CARTESIAN_POINT('Ctrl Pts',(-0.191413404359537,-3.21751837554626,
-32.2628319206372));
#15435=CARTESIAN_POINT('Ctrl Pts',(-0.093457474831853,-3.22169192450732,
-32.2568746313912));
#15436=CARTESIAN_POINT('Ctrl Pts',(-0.0496979836122681,-3.2226639569138,
-32.2541890225231));
#15437=CARTESIAN_POINT('Ctrl Pts',(0.0468487302272742,-3.22284172256959,
-32.2482042174224));
#15438=CARTESIAN_POINT('Ctrl Pts',(0.0996231243880949,-3.2216421735617,
-32.2448934835205));
#15439=CARTESIAN_POINT('Ctrl Pts',(0.268627209632442,-3.21364427555639,
-32.2341573191384));
#15440=CARTESIAN_POINT('Ctrl Pts',(0.384517066310479,-3.20184506847776,
-32.2265879972149));
#15441=CARTESIAN_POINT('Ctrl Pts',(0.710789779902625,-3.15065637098371,
-32.2047329711291));
#15442=CARTESIAN_POINT('Ctrl Pts',(0.918234945117026,-3.09656167630718,
-32.190151127381));
#15443=CARTESIAN_POINT('Ctrl Pts',(1.19447700207898,-2.99430400275913,-32.170571244194));
#15444=CARTESIAN_POINT('Ctrl Pts',(1.2690948516739,-2.96344934072554,-32.1652710526442));
#15445=CARTESIAN_POINT('Ctrl Pts',(1.37194288818179,-2.91632312282324,-32.1580197509992));
#15446=CARTESIAN_POINT('Ctrl Pts',(1.40120130314866,-2.90237884179815,-32.155963304045));
#15447=CARTESIAN_POINT('Ctrl Pts',(1.45262365682647,-2.8769125237363,-32.1523667801924));
#15448=CARTESIAN_POINT('Ctrl Pts',(1.47487137825699,-2.86557073950386,-32.1508172576355));
#15449=CARTESIAN_POINT('Ctrl Pts',(1.52708523768021,-2.83818310935327,-32.1471950767989));
#15450=CARTESIAN_POINT('Ctrl Pts',(1.55693294504448,-2.82192003791012,-32.1451350262465));
#15451=CARTESIAN_POINT('Ctrl Pts',(1.6713397190822,-2.75721542873139,-32.1372584150021));
#15452=CARTESIAN_POINT('Ctrl Pts',(1.75394834572748,-2.70541711894681,-32.1316123486419));
#15453=CARTESIAN_POINT('Ctrl Pts',(1.98935590321743,-2.54248639838375,-32.115275583791));
#15454=CARTESIAN_POINT('Ctrl Pts',(2.13480069364762,-2.42163817331102,-32.1048365903351));
#15455=CARTESIAN_POINT('Ctrl Pts',(2.26878022305635,-2.28883242330415,-32.0941031001172));
#15456=CARTESIAN_POINT('Origin',(0.,0.,-39.));
#15457=CARTESIAN_POINT('',(3.9333499476854,-0.00313792129108339,-38.595836477965));
#15458=CARTESIAN_POINT('',(-1.7510912850176,-3.52776001450859,-38.9999028013849));
#15459=CARTESIAN_POINT('Ctrl Pts',(3.93554779283278,-0.00313967467311022,
-38.595836477965));
#15460=CARTESIAN_POINT('Ctrl Pts',(3.93730083378416,-0.212909402327876,
-38.6064681800308));
#15461=CARTESIAN_POINT('Ctrl Pts',(3.82770051767509,-1.70709904727174,-38.6822941691407));
#15462=CARTESIAN_POINT('Ctrl Pts',(2.00357591915369,-4.09649302512289,-38.8169829436141));
#15463=CARTESIAN_POINT('Ctrl Pts',(-0.708776008939174,-4.0366411418627,
-38.9410400160216));
#15464=CARTESIAN_POINT('Ctrl Pts',(-1.7510912850176,-3.52776001450859,-38.9999028013849));
#15465=CARTESIAN_POINT('',(1.74869447533106,-3.52286199445091,-39.));
#15466=CARTESIAN_POINT('Origin',(0.,0.,-39.));
#15467=CARTESIAN_POINT('',(3.9346390333135,-0.00367440651247183,-38.779163522035));
#15468=CARTESIAN_POINT('Ctrl Pts',(1.74869447533105,-3.52286199445091,-39.));
#15469=CARTESIAN_POINT('Ctrl Pts',(2.9031442039855,-2.94981091674041,-38.9348057129559));
#15470=CARTESIAN_POINT('Ctrl Pts',(3.85357960338317,-1.6179858509449,-38.8611935536343));
#15471=CARTESIAN_POINT('Ctrl Pts',(3.9372815668327,-0.169521116836944,-38.7875813943125));
#15472=CARTESIAN_POINT('Ctrl Pts',(3.93601136498645,-0.00367568807969895,
-38.779163522035));
#15473=CARTESIAN_POINT('',(3.93299998071207,0.000389511058544483,-37.529163521997));
#15474=CARTESIAN_POINT('Ctrl Pts',(3.93299828502308,-0.00367287428139504,
-38.779163522035));
#15475=CARTESIAN_POINT('Ctrl Pts',(3.93310403942478,0.109571372226196,-38.7734110959793));
#15476=CARTESIAN_POINT('Ctrl Pts',(3.9283146543598,0.223023809436804,-38.7676586699237));
#15477=CARTESIAN_POINT('Ctrl Pts',(3.91860284299163,0.336215346017903,-38.761906243868));
#15478=CARTESIAN_POINT('Ctrl Pts',(3.90890215755498,0.449277209437349,-38.7561604078393));
#15479=CARTESIAN_POINT('Ctrl Pts',(3.89429028806077,0.5620783406858,-38.7504145718106));
#15480=CARTESIAN_POINT('Ctrl Pts',(3.87479196582847,0.674148515945203,-38.7446687357818));
#15481=CARTESIAN_POINT('Ctrl Pts',(3.85531062193827,0.786121105076323,-38.7389279029923));
#15482=CARTESIAN_POINT('Ctrl Pts',(3.83095135722373,0.897363581263983,-38.7331870702027));
#15483=CARTESIAN_POINT('Ctrl Pts',(3.80179073465061,1.00741064612441,-38.7274462374132));
#15484=CARTESIAN_POINT('Ctrl Pts',(3.77264376560108,1.11740618498629,-38.7217080925839));
#15485=CARTESIAN_POINT('Ctrl Pts',(3.73870001351969,1.22620700873158,-38.7159699477547));
#15486=CARTESIAN_POINT('Ctrl Pts',(3.70008701768355,1.33335856451655,-38.7102318029254));
#15487=CARTESIAN_POINT('Ctrl Pts',(3.66148195017559,1.44048811908973,-38.7044948362978));
#15488=CARTESIAN_POINT('Ctrl Pts',(3.61820968976194,1.54596867354476,-38.6987578696702));
#15489=CARTESIAN_POINT('Ctrl Pts',(3.57044717408169,1.64936229406763,-38.6930209030426));
#15490=CARTESIAN_POINT('Ctrl Pts',(3.52268190956214,1.75276186512397,-38.6872836062398));
#15491=CARTESIAN_POINT('Ctrl Pts',(3.47042605816341,1.85407387317384,-38.681546309437));
#15492=CARTESIAN_POINT('Ctrl Pts',(3.41390368481467,1.95288264645083,-38.6758090126341));
#15493=CARTESIAN_POINT('Ctrl Pts',(3.35732852695473,2.0517836942112,-38.6700663579458));
#15494=CARTESIAN_POINT('Ctrl Pts',(3.2964791044753,2.14817646423882,-38.6643237032574));
#15495=CARTESIAN_POINT('Ctrl Pts',(3.23162418551736,2.24167217129965,-38.658581048569));
#15496=CARTESIAN_POINT('Ctrl Pts',(3.16673908556028,2.33521138768714,-38.6528357214688));
#15497=CARTESIAN_POINT('Ctrl Pts',(3.09784504016324,2.42585051537552,-38.6470903943685));
#15498=CARTESIAN_POINT('Ctrl Pts',(3.02525145244781,2.51323350476282,-38.6413450672682));
#15499=CARTESIAN_POINT('Ctrl Pts',(2.95254227015903,2.60075563866267,-38.6355905915826));
#15500=CARTESIAN_POINT('Ctrl Pts',(2.87612206962711,2.68501096021976,-38.629836115897));
#15501=CARTESIAN_POINT('Ctrl Pts',(2.79633764742713,2.76567980098595,-38.6240816402113));
#15502=CARTESIAN_POINT('Ctrl Pts',(2.72587064216683,2.83692794028269,-38.6189991860526));
#15503=CARTESIAN_POINT('Ctrl Pts',(2.65277997360696,2.9053788043207,-38.6139167318939));
#15504=CARTESIAN_POINT('Ctrl Pts',(2.57732468195596,2.97083935677791,-38.6088342777352));
#15505=CARTESIAN_POINT('Ctrl Pts',(2.48987138838526,3.04670866675049,-38.6029436722406));
#15506=CARTESIAN_POINT('Ctrl Pts',(2.39892754289888,3.11883256847447,-38.5970530667459));
#15507=CARTESIAN_POINT('Ctrl Pts',(2.30484669155908,3.1868747588208,-38.5911624612512));
#15508=CARTESIAN_POINT('Ctrl Pts',(2.21088382408729,3.25483161957359,-38.5852792429816));
#15509=CARTESIAN_POINT('Ctrl Pts',(2.1137921052492,3.31871671175555,-38.579396024712));
#15510=CARTESIAN_POINT('Ctrl Pts',(2.01395958894456,3.37823264061228,-38.5735128064424));
#15511=CARTESIAN_POINT('Ctrl Pts',(1.91422606988959,3.43768955149085,-38.5676354221681));
#15512=CARTESIAN_POINT('Ctrl Pts',(1.81175751084977,3.49278570946986,-38.5617580378937));
#15513=CARTESIAN_POINT('Ctrl Pts',(1.70697198469082,3.54326623942947,-38.5558806536194));
#15514=CARTESIAN_POINT('Ctrl Pts',(1.60101867459009,3.59430935044794,-38.5499377687437));
#15515=CARTESIAN_POINT('Ctrl Pts',(1.49269678112721,3.64063307271995,-38.543994883868));
#15516=CARTESIAN_POINT('Ctrl Pts',(1.38246565758099,3.68202087251134,-38.5380519989923));
#15517=CARTESIAN_POINT('Ctrl Pts',(1.2735689627828,3.72290764257462,-38.5321810571049));
#15518=CARTESIAN_POINT('Ctrl Pts',(1.16280940652878,3.75897720033455,-38.5263101152174));
#15519=CARTESIAN_POINT('Ctrl Pts',(1.05065053183007,3.79006892549004,-38.5204391733299));
#15520=CARTESIAN_POINT('Ctrl Pts',(0.938507535572435,3.82115624895972,-38.5145690625975));
#15521=CARTESIAN_POINT('Ctrl Pts',(0.824966010151,3.84726703192967,-38.508698951865));
#15522=CARTESIAN_POINT('Ctrl Pts',(0.710504059987592,3.86829070530398,-38.5028288411325));
#15523=CARTESIAN_POINT('Ctrl Pts',(0.5960311126015,3.88931639858113,-38.4969581664142));
#15524=CARTESIAN_POINT('Ctrl Pts',(0.480637968203892,3.90525393657037,-38.4910874916959));
#15525=CARTESIAN_POINT('Ctrl Pts',(0.364811642391675,3.91604410924794,-38.4852168169776));
#15526=CARTESIAN_POINT('Ctrl Pts',(0.246490661258306,3.92706667953889,-38.4792197002797));
#15527=CARTESIAN_POINT('Ctrl Pts',(0.127718069625044,3.93271755714998,-38.4732225835818));
#15528=CARTESIAN_POINT('Ctrl Pts',(0.00901585574032525,3.93298966618847,
-38.4672254668839));
#15529=CARTESIAN_POINT('Ctrl Pts',(-0.107349584636595,3.93325641848447,
-38.4613464095125));
#15530=CARTESIAN_POINT('Ctrl Pts',(-0.223646980528024,3.92835430643586,
-38.4554673521411));
#15531=CARTESIAN_POINT('Ctrl Pts',(-0.339388193689483,3.91832931923597,
-38.4495882947697));
#15532=CARTESIAN_POINT('Ctrl Pts',(-0.458615764137953,3.90800235933144,
-38.4435321484085));
#15533=CARTESIAN_POINT('Ctrl Pts',(-0.577252643695642,3.8922390778494,-38.4374760020474));
#15534=CARTESIAN_POINT('Ctrl Pts',(-0.69477607476468,3.87114649760695,-38.4314198556863));
#15535=CARTESIAN_POINT('Ctrl Pts',(-0.812299505833717,3.85005391736451,
-38.4253637093252));
#15536=CARTESIAN_POINT('Ctrl Pts',(-0.92870904423043,3.8236322024653,-38.419307562964));
#15537=CARTESIAN_POINT('Ctrl Pts',(-1.0434996866262,3.79204396124452,-38.4132514166029));
#15538=CARTESIAN_POINT('Ctrl Pts',(-1.15520854495649,3.76130376945023,-38.4073578595867));
#15539=CARTESIAN_POINT('Ctrl Pts',(-1.26572912502489,3.7255761015192,-38.4014643025705));
#15540=CARTESIAN_POINT('Ctrl Pts',(-1.37458525047183,3.68497006625363,-38.3955707455544));
#15541=CARTESIAN_POINT('Ctrl Pts',(-1.48330825929835,3.6444136867898,-38.3896843955777));
#15542=CARTESIAN_POINT('Ctrl Pts',(-1.59037048124739,3.59899094817998,-38.383798045601));
#15543=CARTESIAN_POINT('Ctrl Pts',(-1.69530914157331,3.54886121375547,-38.3779116956242));
#15544=CARTESIAN_POINT('Ctrl Pts',(-1.80014692174289,3.49877967029729,-38.3720310043429));
#15545=CARTESIAN_POINT('Ctrl Pts',(-1.90286483388534,3.44400030914931,-38.3661503130615));
#15546=CARTESIAN_POINT('Ctrl Pts',(-2.00301898693927,3.38473099934999,-38.3602696217801));
#15547=CARTESIAN_POINT('Ctrl Pts',(-2.10421236949566,3.32484669343263,-38.3543279106838));
#15548=CARTESIAN_POINT('Ctrl Pts',(-2.20278808548508,3.26037887490091,-38.3483861995876));
#15549=CARTESIAN_POINT('Ctrl Pts',(-2.29831241675886,3.19159036139853,-38.3424444884914));
#15550=CARTESIAN_POINT('Ctrl Pts',(-2.3927587841673,3.12357810595437,-38.33656982785));
#15551=CARTESIAN_POINT('Ctrl Pts',(-2.48422194944399,3.05134242750369,-38.3306951672086));
#15552=CARTESIAN_POINT('Ctrl Pts',(-2.57231145605353,2.97518113281456,-38.3248205065672));
#15553=CARTESIAN_POINT('Ctrl Pts',(-2.66039072498379,2.89902868951919,-38.3189465286733));
#15554=CARTESIAN_POINT('Ctrl Pts',(-2.74509680518825,2.81895180536477,-38.3130725507795));
#15555=CARTESIAN_POINT('Ctrl Pts',(-2.82607291940948,2.73528807517241,-38.3071985728856));
#15556=CARTESIAN_POINT('Ctrl Pts',(-2.90705880239056,2.65161425199279,-38.3013238863694));
#15557=CARTESIAN_POINT('Ctrl Pts',(-2.98431353973336,2.56435301685264,-38.2954491998533));
#15558=CARTESIAN_POINT('Ctrl Pts',(-3.05751823924298,2.47387776915039,-38.2895745133371));
#15559=CARTESIAN_POINT('Ctrl Pts',(-3.13218681977183,2.38159327970945,-38.2835823501815));
#15560=CARTESIAN_POINT('Ctrl Pts',(-3.20264136328559,2.2859651996263,-38.277590187026));
#15561=CARTESIAN_POINT('Ctrl Pts',(-3.26858839065875,2.1874228974871,-38.2715980238705));
#15562=CARTESIAN_POINT('Ctrl Pts',(-3.33333834646129,2.09066933690446,-38.2657146305632));
#15563=CARTESIAN_POINT('Ctrl Pts',(-3.39374288383936,1.99110684518476,-38.2598312372559));
#15564=CARTESIAN_POINT('Ctrl Pts',(-3.44957008258935,1.88916787112859,-38.2539478439486));
#15565=CARTESIAN_POINT('Ctrl Pts',(-3.50694544809086,1.78440198592781,-38.2479012958689));
#15566=CARTESIAN_POINT('Ctrl Pts',(-3.55948568566393,1.67712630679095,-38.2418547477893));
#15567=CARTESIAN_POINT('Ctrl Pts',(-3.60699189470479,1.56783241181383,-38.2358081997096));
#15568=CARTESIAN_POINT('Ctrl Pts',(-3.65449810374564,1.45853851683671,-38.2297616516299));
#15569=CARTESIAN_POINT('Ctrl Pts',(-3.69697017722673,1.34722686104502,-38.2237151035502));
#15570=CARTESIAN_POINT('Ctrl Pts',(-3.7342648234265,1.23440480739482,-38.2176685554706));
#15571=CARTESIAN_POINT('Ctrl Pts',(-3.77052159073377,1.12472249738144,-38.2117902777799));
#15572=CARTESIAN_POINT('Ctrl Pts',(-3.80200079442422,1.0132633042238,-38.2059120000893));
#15573=CARTESIAN_POINT('Ctrl Pts',(-3.82852756824506,0.900480793347386,
-38.2000337223986));
#15574=CARTESIAN_POINT('Ctrl Pts',(-3.85502069485874,0.787841338559683,
-38.1941629008588));
#15575=CARTESIAN_POINT('Ctrl Pts',(-3.87657379121321,0.67388230218471,-38.188292079319));
#15576=CARTESIAN_POINT('Ctrl Pts',(-3.89306112942339,0.559074272858875,
-38.1824212577792));
#15577=CARTESIAN_POINT('Ctrl Pts',(-3.90953193684349,0.444381354135343,
-38.1765563225334));
#15578=CARTESIAN_POINT('Ctrl Pts',(-3.92094703126756,0.328841541576567,
-38.1706913872875));
#15579=CARTESIAN_POINT('Ctrl Pts',(-3.92723145224885,0.212936893157096,
-38.1648264520416));
#15580=CARTESIAN_POINT('Ctrl Pts',(-3.93360437720446,0.0953999508386366,
-38.1588789204706));
#15581=CARTESIAN_POINT('Ctrl Pts',(-3.93470090624358,-0.0225117637689814,
-38.1529313888996));
#15582=CARTESIAN_POINT('Ctrl Pts',(-3.93049719147084,-0.140288373858487,
-38.1469838573286));
#15583=CARTESIAN_POINT('Ctrl Pts',(-3.92635644108237,-0.25630089381883,
-38.1411254095047));
#15584=CARTESIAN_POINT('Ctrl Pts',(-3.91707315609044,-0.372181903431668,
-38.1352669616807));
#15585=CARTESIAN_POINT('Ctrl Pts',(-3.90267701153491,-0.487443477376551,
-38.1294085138568));
#15586=CARTESIAN_POINT('Ctrl Pts',(-3.88828289391023,-0.602688822862551,
-38.1235508908834));
#15587=CARTESIAN_POINT('Ctrl Pts',(-3.86877739943271,-0.717314497090862,
-38.1176932679101));
#15588=CARTESIAN_POINT('Ctrl Pts',(-3.84424200732712,-0.830838365208051,
-38.1118356449367));
#15589=CARTESIAN_POINT('Ctrl Pts',(-3.81970416507145,-0.944373570030658,
-38.1059774370102));
#15590=CARTESIAN_POINT('Ctrl Pts',(-3.79013551385952,-1.05680634701712,
-38.1001192290837));
#15591=CARTESIAN_POINT('Ctrl Pts',(-3.75566836719429,-1.16766609767356,
-38.0942610211572));
#15592=CARTESIAN_POINT('Ctrl Pts',(-3.72028101543238,-1.28148558586095,
-38.0882464105889));
#15593=CARTESIAN_POINT('Ctrl Pts',(-3.67973004258524,-1.39364642639785,
-38.0822318000207));
#15594=CARTESIAN_POINT('Ctrl Pts',(-3.63421238298233,-1.50365865653675,
-38.0762171894524));
#15595=CARTESIAN_POINT('Ctrl Pts',(-3.58981364157883,-1.61096655856358,
-38.0703504304496));
#15596=CARTESIAN_POINT('Ctrl Pts',(-3.54068979591582,-1.71622990698234,
-38.0644836714468));
#15597=CARTESIAN_POINT('Ctrl Pts',(-3.48707090017794,-1.81901773964198,
-38.058616912444));
#15598=CARTESIAN_POINT('Ctrl Pts',(-3.43142508352822,-1.92569119517083,
-38.052528376093));
#15599=CARTESIAN_POINT('Ctrl Pts',(-3.37093791991247,-2.02969785558404,
-38.046439839742));
#15600=CARTESIAN_POINT('Ctrl Pts',(-3.30591594764488,-2.1305888263828,-38.0403513033911));
#15601=CARTESIAN_POINT('Ctrl Pts',(-3.24089397537729,-2.23147979718156,
-38.0342627670401));
#15602=CARTESIAN_POINT('Ctrl Pts',(-3.17133753228712,-2.32925471819556,
-38.0281742306891));
#15603=CARTESIAN_POINT('Ctrl Pts',(-3.09759881119903,-2.4235037868463,-38.0220856943382));
#15604=CARTESIAN_POINT('Ctrl Pts',(-3.02631412947532,-2.5146162276696,-38.0161997856929));
#15605=CARTESIAN_POINT('Ctrl Pts',(-2.95089313000904,-2.60272526257842,
-38.0103138770477));
#15606=CARTESIAN_POINT('Ctrl Pts',(-2.87161794774054,-2.68743360145221,
-38.0044279684024));
#15607=CARTESIAN_POINT('Ctrl Pts',(-2.79244200045035,-2.77203590423842,
-37.9985494276118));
#15608=CARTESIAN_POINT('Ctrl Pts',(-2.70942174467608,-2.85324568012192,
-37.9926708868211));
#15609=CARTESIAN_POINT('Ctrl Pts',(-2.62288064297686,-2.9306972093168,-37.9867923460305));
#15610=CARTESIAN_POINT('Ctrl Pts',(-2.53642504872363,-3.00807221207143,
-37.9809196135667));
#15611=CARTESIAN_POINT('Ctrl Pts',(-2.44645583372397,-3.08169608266493,
-37.975046881103));
#15612=CARTESIAN_POINT('Ctrl Pts',(-2.35333406803029,-3.15123908395539,
-37.9691741486393));
#15613=CARTESIAN_POINT('Ctrl Pts',(-2.25907212034071,-3.22163356907911,
-37.9632295104962));
#15614=CARTESIAN_POINT('Ctrl Pts',(-2.16158019445166,-3.28784626766858,
-37.9572848723531));
#15615=CARTESIAN_POINT('Ctrl Pts',(-2.06126854352396,-3.34957624058307,
-37.9513402342101));
#15616=CARTESIAN_POINT('Ctrl Pts',(-1.96227733703284,-3.4104936359101,-37.9454738478383));
#15617=CARTESIAN_POINT('Ctrl Pts',(-1.86054055956049,-3.46704540009716,
-37.9396074614665));
#15618=CARTESIAN_POINT('Ctrl Pts',(-1.75648197291948,-3.51898566050061,
-37.9337410750947));
#15619=CARTESIAN_POINT('Ctrl Pts',(-1.65243732970433,-3.57091896112118,
-37.9278754747947));
#15620=CARTESIAN_POINT('Ctrl Pts',(-1.54607186377699,-3.61824180339004,
-37.9220098744947));
#15621=CARTESIAN_POINT('Ctrl Pts',(-1.43783318258035,-3.66075466797092,
-37.9161442741948));
#15622=CARTESIAN_POINT('Ctrl Pts',(-1.32958315663315,-3.70327198842505,
-37.9102780591075));
#15623=CARTESIAN_POINT('Ctrl Pts',(-1.21945990771322,-3.74097817870569,
-37.9044118440201));
#15624=CARTESIAN_POINT('Ctrl Pts',(-1.10792958207428,-3.77372243827825,
-37.8985456289328));
#15625=CARTESIAN_POINT('Ctrl Pts',(-0.993787891794018,-3.80723337006452,
-37.8925420626222));
#15626=CARTESIAN_POINT('Ctrl Pts',(-0.878172845458401,-3.83554698500218,
-37.8865384963116));
#15627=CARTESIAN_POINT('Ctrl Pts',(-0.761597616398928,-3.85855647499106,
-37.8805349300011));
#15628=CARTESIAN_POINT('Ctrl Pts',(-0.647523367456019,-3.88107232428614,
-37.8746601629225));
#15629=CARTESIAN_POINT('Ctrl Pts',(-0.532530140825998,-3.89850934457288,
-37.8687853958439));
#15630=CARTESIAN_POINT('Ctrl Pts',(-0.417105225738954,-3.91081989238334,
-37.8629106287653));
#15631=CARTESIAN_POINT('Ctrl Pts',(-0.297884422181058,-3.92353528750487,
-37.8568426628387));
#15632=CARTESIAN_POINT('Ctrl Pts',(-0.178203529785833,-3.93078119112377,
-37.8507746969121));
#15633=CARTESIAN_POINT('Ctrl Pts',(-0.0585996244716005,-3.93256342402914,
-37.8447067309855));
#15634=CARTESIAN_POINT('Ctrl Pts',(0.0610042808426331,-3.93434565693451,
-37.8386387650589));
#15635=CARTESIAN_POINT('Ctrl Pts',(0.180530724763209,-3.93066429775285,
-37.8325707991324));
#15636=CARTESIAN_POINT('Ctrl Pts',(0.299449635869794,-3.92158372543255,
-37.8265028332058));
#15637=CARTESIAN_POINT('Ctrl Pts',(0.41479306394575,-3.91277617471948,-37.820617310164));
#15638=CARTESIAN_POINT('Ctrl Pts',(0.529930234432639,-3.89886158014946,
-37.8147317871223));
#15639=CARTESIAN_POINT('Ctrl Pts',(0.644374131683919,-3.87985450479997,
-37.8088462640805));
#15640=CARTESIAN_POINT('Ctrl Pts',(0.758675010952778,-3.86087118216803,
-37.8029680960454));
#15641=CARTESIAN_POINT('Ctrl Pts',(0.872283937964804,-3.83680810304319,
-37.7970899280104));
#15642=CARTESIAN_POINT('Ctrl Pts',(0.984717262339541,-3.80773172810934,
-37.7912117599753));
#15643=CARTESIAN_POINT('Ctrl Pts',(1.09703974336824,-3.77868401836622,-37.785339386982));
#15644=CARTESIAN_POINT('Ctrl Pts',(1.20818853149974,-3.74463294734043,-37.7794670139888));
#15645=CARTESIAN_POINT('Ctrl Pts',(1.31768907691635,-3.70569622292159,-37.7735946409955));
#15646=CARTESIAN_POINT('Ctrl Pts',(1.42853973645088,-3.66627941850731,-37.7676498631237));
#15647=CARTESIAN_POINT('Ctrl Pts',(1.53770081122438,-3.62185573636504,-37.761705085252));
#15648=CARTESIAN_POINT('Ctrl Pts',(1.64469434049997,-3.57259982734246,-37.7557603073802));
#15649=CARTESIAN_POINT('Ctrl Pts',(1.75027115444445,-3.52399612226092,-37.7498942450907));
#15650=CARTESIAN_POINT('Ctrl Pts',(1.85373709783592,-3.47068757164734,-37.7440281828012));
#15651=CARTESIAN_POINT('Ctrl Pts',(1.95465267010927,-3.41289055482808,-37.7381621205116));
#15652=CARTESIAN_POINT('Ctrl Pts',(2.05555495924655,-3.35510114561209,-37.7322968303498));
#15653=CARTESIAN_POINT('Ctrl Pts',(2.15390718824994,-3.29282464947338,-37.7264315401879));
#15654=CARTESIAN_POINT('Ctrl Pts',(2.24929521998674,-3.22632298651961,-37.720566250026));
#15655=CARTESIAN_POINT('Ctrl Pts',(2.34469348397095,-3.1598141899511,-37.7147003306961));
#15656=CARTESIAN_POINT('Ctrl Pts',(2.4371265813273,-3.08907956066971,-37.7088344113662));
#15657=CARTESIAN_POINT('Ctrl Pts',(2.52621064934735,-3.01442345318704,-37.7029684920363));
#15658=CARTESIAN_POINT('Ctrl Pts',(2.61739236773523,-2.93800942855034,-37.696964448706));
#15659=CARTESIAN_POINT('Ctrl Pts',(2.70506501123355,-2.85748722065425,-37.6909604053758));
#15660=CARTESIAN_POINT('Ctrl Pts',(2.78885512983911,-2.77322484929911,-37.6849563620456));
#15661=CARTESIAN_POINT('Ctrl Pts',(2.87083753200744,-2.6907803829222,-37.6790818519825));
#15662=CARTESIAN_POINT('Ctrl Pts',(2.9491030055128,-2.60475585219117,-37.6732073419194));
#15663=CARTESIAN_POINT('Ctrl Pts',(3.02334183484842,-2.51553039132016,-37.6673328318563));
#15664=CARTESIAN_POINT('Ctrl Pts',(3.10003611953523,-2.4233537910344,-37.6612640218925));
#15665=CARTESIAN_POINT('Ctrl Pts',(3.1724324905158,-2.32776123575489,-37.6551952119287));
#15666=CARTESIAN_POINT('Ctrl Pts',(3.24023798824153,-2.22920317143962,-37.6491264019649));
#15667=CARTESIAN_POINT('Ctrl Pts',(3.30804348596726,-2.13064510712436,-37.6430575920011));
#15668=CARTESIAN_POINT('Ctrl Pts',(3.37125791289597,-2.02912197265364,-37.6369887820373));
#15669=CARTESIAN_POINT('Ctrl Pts',(3.42964097392287,-1.925110851351,-37.6309199720735));
#15670=CARTESIAN_POINT('Ctrl Pts',(3.48856666349948,-1.82013302150459,-37.6247947568871));
#15671=CARTESIAN_POINT('Ctrl Pts',(3.54274534667089,-1.71231104743553,-37.6186695417008));
#15672=CARTESIAN_POINT('Ctrl Pts',(3.59190567969494,-1.6020931896039,-37.6125443265145));
#15673=CARTESIAN_POINT('Ctrl Pts',(3.64098595593051,-1.4920548197291,-37.6064290861396));
#15674=CARTESIAN_POINT('Ctrl Pts',(3.68506401051628,-1.37962866589796,-37.6003138457648));
#15675=CARTESIAN_POINT('Ctrl Pts',(3.72391385284358,-1.26528835314314,-37.59419860539));
#15676=CARTESIAN_POINT('Ctrl Pts',(3.76268577704808,-1.15117736390669,-37.5880956298797));
#15677=CARTESIAN_POINT('Ctrl Pts',(3.79625027498637,-1.03516021058229,-37.5819926543693));
#15678=CARTESIAN_POINT('Ctrl Pts',(3.82442934891155,-0.917730437102317,
-37.575889678859));
#15679=CARTESIAN_POINT('Ctrl Pts',(3.85257463465805,-0.80044146804261,-37.5697940211344));
#15680=CARTESIAN_POINT('Ctrl Pts',(3.87534726934537,-0.681743602605054,
-37.5636983634099));
#15681=CARTESIAN_POINT('Ctrl Pts',(3.89261871291701,-0.562146382936252,
-37.5576027056853));
#15682=CARTESIAN_POINT('Ctrl Pts',(3.90986570691575,-0.442718465904437,
-37.5515156770153));
#15683=CARTESIAN_POINT('Ctrl Pts',(3.92162697995051,-0.322394090351545,
-37.5454286483452));
#15684=CARTESIAN_POINT('Ctrl Pts',(3.92782495184999,-0.201693201731384,
-37.5393416196752));
#15685=CARTESIAN_POINT('Ctrl Pts',(3.93127948698162,-0.134418701794884,
-37.5359489204618));
#15686=CARTESIAN_POINT('Ctrl Pts',(3.93300665744572,-0.0670274303798492,
-37.5325562212484));
#15687=CARTESIAN_POINT('Ctrl Pts',(3.93299998071214,0.000389510303426849,
-37.529163522035));
#15688=CARTESIAN_POINT('',(3.93299955983151,0.00186074317507175,-36.2791635220746));
#15689=CARTESIAN_POINT('Ctrl Pts',(3.93299998071207,0.000389511058542827,
-37.529163521997));
#15690=CARTESIAN_POINT('Ctrl Pts',(3.93298780586095,0.12332232175523,-37.5229770346553));
#15691=CARTESIAN_POINT('Ctrl Pts',(3.92720762809877,0.246130529403216,-37.5167905473136));
#15692=CARTESIAN_POINT('Ctrl Pts',(3.91572001853827,0.368273996392117,-37.5106040599719));
#15693=CARTESIAN_POINT('Ctrl Pts',(3.9040731652767,0.492110642248457,-37.5043318142194));
#15694=CARTESIAN_POINT('Ctrl Pts',(3.88655953275626,0.615263622070913,-37.4980595684668));
#15695=CARTESIAN_POINT('Ctrl Pts',(3.86329543211516,0.737182069910901,-37.4917873227142));
#15696=CARTESIAN_POINT('Ctrl Pts',(3.8402520103762,0.857944022185726,-37.4855745743103));
#15697=CARTESIAN_POINT('Ctrl Pts',(3.81156691509454,0.977494457883954,-37.4793618259063));
#15698=CARTESIAN_POINT('Ctrl Pts',(3.77740317841339,1.09531467063689,-37.4731490775024));
#15699=CARTESIAN_POINT('Ctrl Pts',(3.74274868024797,1.21482736870041,-37.4668470830755));
#15700=CARTESIAN_POINT('Ctrl Pts',(3.70245706381593,1.33255941114986,-37.4605450886486));
#15701=CARTESIAN_POINT('Ctrl Pts',(3.6567484231738,1.44799170219167,-37.4542430942217));
#15702=CARTESIAN_POINT('Ctrl Pts',(3.61103978253167,1.56342399323349,-37.4479410997948));
#15703=CARTESIAN_POINT('Ctrl Pts',(3.55991432357928,1.67655623474915,-37.441639105368));
#15704=CARTESIAN_POINT('Ctrl Pts',(3.50363957301195,1.78689639946602,-37.4353371109411));
#15705=CARTESIAN_POINT('Ctrl Pts',(3.4510897069913,1.88993303337576,-37.4294522521108));
#15706=CARTESIAN_POINT('Ctrl Pts',(3.39390730272993,1.99081327251063,-37.4235673932806));
#15707=CARTESIAN_POINT('Ctrl Pts',(3.33229321363909,2.08909332925431,-37.4176825344503));
#15708=CARTESIAN_POINT('Ctrl Pts',(3.27075630360959,2.18725027839971,-37.411805047114));
#15709=CARTESIAN_POINT('Ctrl Pts',(3.20479896627598,2.28281317765645,-37.4059275597776));
#15710=CARTESIAN_POINT('Ctrl Pts',(3.1346686596137,2.37536131871251,-37.4000500724412));
#15711=CARTESIAN_POINT('Ctrl Pts',(3.06460768476465,2.46781796536715,-37.394178395672));
#15712=CARTESIAN_POINT('Ctrl Pts',(2.99038219450984,2.55726545692151,-37.3883067189027));
#15713=CARTESIAN_POINT('Ctrl Pts',(2.91228344309494,2.64331120889597,-37.3824350421335));
#15714=CARTESIAN_POINT('Ctrl Pts',(2.83320898553806,2.73043195076685,-37.37649000912));
#15715=CARTESIAN_POINT('Ctrl Pts',(2.75016405047795,2.81406500967108,-37.3705449761064));
#15716=CARTESIAN_POINT('Ctrl Pts',(2.66349393190528,2.89383639390753,-37.3645999430929));
#15717=CARTESIAN_POINT('Ctrl Pts',(2.57798573639555,2.97253834138038,-37.3587346108007));
#15718=CARTESIAN_POINT('Ctrl Pts',(2.4889492809948,3.04748124265705,-37.3528692785085));
#15719=CARTESIAN_POINT('Ctrl Pts',(2.39675340126518,3.11834285054158,-37.3470039462163));
#15720=CARTESIAN_POINT('Ctrl Pts',(2.30456983732484,3.18919499252988,-37.341139397432));
#15721=CARTESIAN_POINT('Ctrl Pts',(2.20922801440525,3.25596667488358,-37.3352748486476));
#15722=CARTESIAN_POINT('Ctrl Pts',(2.11112903414671,3.3183765912239,-37.3294102998633));
#15723=CARTESIAN_POINT('Ctrl Pts',(2.01301970639734,3.38079309056882,-37.3235451324857));
#15724=CARTESIAN_POINT('Ctrl Pts',(1.91215299013068,3.43884668855458,-37.3176799651081));
#15725=CARTESIAN_POINT('Ctrl Pts',(1.80895749424776,3.49230035707195,-37.3118147977306));
#15726=CARTESIAN_POINT('Ctrl Pts',(1.70330089064088,3.54702884127131,-37.3058097520704));
#15727=CARTESIAN_POINT('Ctrl Pts',(1.59520342017676,3.59693499162826,-37.2998047064102));
#15728=CARTESIAN_POINT('Ctrl Pts',(1.48514886698982,3.64181573433896,-37.2937996607501));
#15729=CARTESIAN_POINT('Ctrl Pts',(1.37750077943175,3.68571510952235,-37.2879259221151));
#15730=CARTESIAN_POINT('Ctrl Pts',(1.26798073092691,3.72480651193384,-37.28205218348));
#15731=CARTESIAN_POINT('Ctrl Pts',(1.15705779767805,3.75895015301246,-37.276178444845));
#15732=CARTESIAN_POINT('Ctrl Pts',(1.042415352559,3.79423871222987,-37.2701077456723));
#15733=CARTESIAN_POINT('Ctrl Pts',(0.926274756106329,3.82424174301004,-37.2640370464995));
#15734=CARTESIAN_POINT('Ctrl Pts',(0.809165139064767,3.84886227055766,-37.2579663473268));
#15735=CARTESIAN_POINT('Ctrl Pts',(0.692055522023205,3.87348279810528,-37.2518956481541));
#15736=CARTESIAN_POINT('Ctrl Pts',(0.573977366695297,3.89272080910603,-37.2458249489814));
#15737=CARTESIAN_POINT('Ctrl Pts',(0.455464109096355,3.90653829436306,-37.2397542498086));
#15738=CARTESIAN_POINT('Ctrl Pts',(0.340581901548086,3.91993243474241,-37.2338695468104));
#15739=CARTESIAN_POINT('Ctrl Pts',(0.224925811904918,3.92827595135078,-37.2279848438122));
#15740=CARTESIAN_POINT('Ctrl Pts',(0.108976507804059,3.93148993649314,-37.2221001408139));
#15741=CARTESIAN_POINT('Ctrl Pts',(-0.00682755354633928,3.93469989566876,
-37.2162228092308));
#15742=CARTESIAN_POINT('Ctrl Pts',(-0.122923691200477,3.93279309178156,
-37.2103454776476));
#15743=CARTESIAN_POINT('Ctrl Pts',(-0.238824603734641,3.9257421984449,-37.2044681460644));
#15744=CARTESIAN_POINT('Ctrl Pts',(-0.354610937519859,3.91869827556706,
-37.198596624766));
#15745=CARTESIAN_POINT('Ctrl Pts',(-0.470202021859575,3.90652040463552,
-37.1927251034675));
#15746=CARTESIAN_POINT('Ctrl Pts',(-0.58510967706775,3.88923330051074,-37.1868535821691));
#15747=CARTESIAN_POINT('Ctrl Pts',(-0.701457123927851,3.87172958916202,
-37.1809084907736));
#15748=CARTESIAN_POINT('Ctrl Pts',(-0.817103469411767,3.8489877140398,-37.174963399378));
#15749=CARTESIAN_POINT('Ctrl Pts',(-0.931545990870102,3.82108768113136,
-37.1690183079825));
#15750=CARTESIAN_POINT('Ctrl Pts',(-1.04445019708959,3.79356267531286,-37.1631531294076));
#15751=CARTESIAN_POINT('Ctrl Pts',(-1.15618233507013,3.76101744065471,-37.1572879508327));
#15752=CARTESIAN_POINT('Ctrl Pts',(-1.26626974629447,3.72358025690589,-37.1514227722578));
#15753=CARTESIAN_POINT('Ctrl Pts',(-1.37634246908157,3.68614806822161,-37.1455583762456));
#15754=CARTESIAN_POINT('Ctrl Pts',(-1.48477051229725,3.64382536095392,-37.1396939802335));
#15755=CARTESIAN_POINT('Ctrl Pts',(-1.59109739978839,3.59678996667676,-37.1338295842213));
#15756=CARTESIAN_POINT('Ctrl Pts',(-1.69743552339359,3.54974960192537,-37.127964568488));
#15757=CARTESIAN_POINT('Ctrl Pts',(-1.80167167377429,3.49799572651596,-37.1220995527547));
#15758=CARTESIAN_POINT('Ctrl Pts',(-1.90337097343573,3.44175361370949,-37.1162345370214));
#15759=CARTESIAN_POINT('Ctrl Pts',(-2.00750214789092,3.38416661675006,-37.1102292746593));
#15760=CARTESIAN_POINT('Ctrl Pts',(-2.10897320448926,3.32187421780444,-37.1042240122972));
#15761=CARTESIAN_POINT('Ctrl Pts',(-2.20734685422763,3.25516648808189,-37.0982187499351));
#15762=CARTESIAN_POINT('Ctrl Pts',(-2.30356356729778,3.18992138934512,-37.0923451587129));
#15763=CARTESIAN_POINT('Ctrl Pts',(-2.39681700584095,3.12045288570387,-37.0864715674906));
#15764=CARTESIAN_POINT('Ctrl Pts',(-2.48673078417477,3.04707384338442,-37.0805979762683));
#15765=CARTESIAN_POINT('Ctrl Pts',(-2.57966802359885,2.97122734075573,-37.0745268783363));
#15766=CARTESIAN_POINT('Ctrl Pts',(-2.66903668757966,2.89120300019649,-37.0684557804043));
#15767=CARTESIAN_POINT('Ctrl Pts',(-2.75446262885671,2.80738750909663,-37.0623846824723));
#15768=CARTESIAN_POINT('Ctrl Pts',(-2.83988857013377,2.72357201799677,-37.0563135845403));
#15769=CARTESIAN_POINT('Ctrl Pts',(-2.92137151010482,2.63596577058062,-37.0502424866083));
#15770=CARTESIAN_POINT('Ctrl Pts',(-2.9985840061201,2.54499174030894,-37.0441713886763));
#15771=CARTESIAN_POINT('Ctrl Pts',(-3.07342358424983,2.45681355157449,-37.0382868695704));
#15772=CARTESIAN_POINT('Ctrl Pts',(-3.14448935456177,2.36519118784049,-37.0324023504645));
#15773=CARTESIAN_POINT('Ctrl Pts',(-3.21144914123017,2.27048087710335,-37.0265178313586));
#15774=CARTESIAN_POINT('Ctrl Pts',(-3.27832500925433,2.17588926389002,-37.0206406871397));
#15775=CARTESIAN_POINT('Ctrl Pts',(-3.34110489296003,2.0782177338312,-37.0147635429209));
#15776=CARTESIAN_POINT('Ctrl Pts',(-3.39949586273868,1.97785663768197,-37.0088863987021));
#15777=CARTESIAN_POINT('Ctrl Pts',(-3.45782907389752,1.87759481575984,-37.0030150679804));
#15778=CARTESIAN_POINT('Ctrl Pts',(-3.51178180185997,1.77464907379141,-36.9971437372588));
#15779=CARTESIAN_POINT('Ctrl Pts',(-3.56110393773355,1.66943935039839,-36.9912724065372));
#15780=CARTESIAN_POINT('Ctrl Pts',(-3.61104629038695,1.56290663409979,-36.9853272449124));
#15781=CARTESIAN_POINT('Ctrl Pts',(-3.6562405417712,1.45405295409796,-36.9793820832877));
#15782=CARTESIAN_POINT('Ctrl Pts',(-3.69647450474803,1.34334107200957,-36.973436921663));
#15783=CARTESIAN_POINT('Ctrl Pts',(-3.73616584641738,1.23412232213505,-36.9675719403421));
#15784=CARTESIAN_POINT('Ctrl Pts',(-3.77102973583569,1.12309558453723,-36.9617069590211));
#15785=CARTESIAN_POINT('Ctrl Pts',(-3.80091085821922,1.01072530782168,-36.9558419777002));
#15786=CARTESIAN_POINT('Ctrl Pts',(-3.83078798260546,0.898370065884793,
-36.9499777810948));
#15787=CARTESIAN_POINT('Ctrl Pts',(-3.85568356019966,0.78467203972006,-36.9441135844893));
#15788=CARTESIAN_POINT('Ctrl Pts',(-3.87549248587364,0.670109686496867,
-36.9382493878839));
#15789=CARTESIAN_POINT('Ctrl Pts',(-3.89530349840427,0.555535264208808,
-36.9323845734893));
#15790=CARTESIAN_POINT('Ctrl Pts',(-3.91002672365672,0.440096739119747,
-36.9265197590948));
#15791=CARTESIAN_POINT('Ctrl Pts',(-3.9196085134202,0.324280899104241,-36.9206549447003));
#15792=CARTESIAN_POINT('Ctrl Pts',(-3.92942020866677,0.205686173587696,
-36.9146494099373));
#15793=CARTESIAN_POINT('Ctrl Pts',(-3.93384054987489,0.0866962472526169,
-36.9086438751742));
#15794=CARTESIAN_POINT('Ctrl Pts',(-3.93286847923819,-0.0321640329351796,
-36.9026383404112));
#15795=CARTESIAN_POINT('Ctrl Pts',(-3.93191779837726,-0.148408870742695,
-36.8967649534953));
#15796=CARTESIAN_POINT('Ctrl Pts',(-3.9258096503033,-0.26452929666638,-36.8908915665794));
#15797=CARTESIAN_POINT('Ctrl Pts',(-3.91459571819556,-0.380038633674274,
-36.8850181796635));
#15798=CARTESIAN_POINT('Ctrl Pts',(-3.9030033254976,-0.499446311731457,
-36.8789465709769));
#15799=CARTESIAN_POINT('Ctrl Pts',(-3.88595449812792,-0.618200444421965,
-36.8728749622903));
#15800=CARTESIAN_POINT('Ctrl Pts',(-3.86356363957789,-0.735775103500807,
-36.8668033536037));
#15801=CARTESIAN_POINT('Ctrl Pts',(-3.84117278102787,-0.853349762579648,
-36.8607317449171));
#15802=CARTESIAN_POINT('Ctrl Pts',(-3.81344006503029,-0.969744497313235,
-36.8546601362305));
#15803=CARTESIAN_POINT('Ctrl Pts',(-3.78053601460536,-1.08445213922598,
-36.8485885275439));
#15804=CARTESIAN_POINT('Ctrl Pts',(-3.74864509202635,-1.19562789054591,
-36.8427038659276));
#15805=CARTESIAN_POINT('Ctrl Pts',(-3.71179525530777,-1.30557241359153,
-36.8368192043114));
#15806=CARTESIAN_POINT('Ctrl Pts',(-3.67009882187724,-1.41381174052817,
-36.8309345426952));
#15807=CARTESIAN_POINT('Ctrl Pts',(-3.62845463042516,-1.52191545306999,
-36.8250572540444));
#15808=CARTESIAN_POINT('Ctrl Pts',(-3.58197606627379,-1.62831783820295,
-36.8191799653937));
#15809=CARTESIAN_POINT('Ctrl Pts',(-3.53082560359532,-1.73255867346411,
-36.813302676743));
#15810=CARTESIAN_POINT('Ctrl Pts',(-3.47972572118794,-1.83669642989805,
-36.8074311998648));
#15811=CARTESIAN_POINT('Ctrl Pts',(-3.42396331078167,-1.93867652136449,
-36.8015597229865));
#15812=CARTESIAN_POINT('Ctrl Pts',(-3.36374921089127,-2.038057959487,-36.7956882461083));
#15813=CARTESIAN_POINT('Ctrl Pts',(-3.30278000271274,-2.13868567958914,
-36.789743138621));
#15814=CARTESIAN_POINT('Ctrl Pts',(-3.23724683771426,-2.23664872183403,
-36.7837980311336));
#15815=CARTESIAN_POINT('Ctrl Pts',(-3.16741718972646,-2.33151396011805,
-36.7778529236462));
#15816=CARTESIAN_POINT('Ctrl Pts',(-3.09852692699529,-2.42510302117965,
-36.7719877928806));
#15817=CARTESIAN_POINT('Ctrl Pts',(-3.02545532729194,-2.5156767780483,-36.7661226621149));
#15818=CARTESIAN_POINT('Ctrl Pts',(-2.94850282556456,-2.60284845652562,
-36.7602575313492));
#15819=CARTESIAN_POINT('Ctrl Pts',(-2.87156060692803,-2.69000848633306,
-36.7543931843355));
#15820=CARTESIAN_POINT('Ctrl Pts',(-2.79073878978542,-2.77376703366651,
-36.7485288373217));
#15821=CARTESIAN_POINT('Ctrl Pts',(-2.70637730467253,-2.85377134416082,
-36.742664490308));
#15822=CARTESIAN_POINT('Ctrl Pts',(-2.6220069209459,-2.9337840936656,-36.7367995247115));
#15823=CARTESIAN_POINT('Ctrl Pts',(-2.53409642542111,-3.01004153610371,
-36.7309345591151));
#15824=CARTESIAN_POINT('Ctrl Pts',(-2.44302121061884,-3.08222912264265,
-36.7250695935186));
#15825=CARTESIAN_POINT('Ctrl Pts',(-2.34976636349886,-3.15614431857455,
-36.7190642662597));
#15826=CARTESIAN_POINT('Ctrl Pts',(-2.25319374342195,-3.22579209143481,
-36.7130589390007));
#15827=CARTESIAN_POINT('Ctrl Pts',(-2.15373949565974,-3.29088060932561,
-36.7070536117418));
#15828=CARTESIAN_POINT('Ctrl Pts',(-2.05646779870621,-3.35454074179745,
-36.7011800730406));
#15829=CARTESIAN_POINT('Ctrl Pts',(-1.95644003669387,-3.41383950676763,
-36.6953065343393));
#15830=CARTESIAN_POINT('Ctrl Pts',(-1.8540899073174,-3.46855007396228,-36.6894329956381));
#15831=CARTESIAN_POINT('Ctrl Pts',(-1.74829502939687,-3.52510200811794,
-36.6833617741003));
#15832=CARTESIAN_POINT('Ctrl Pts',(-1.640019142131,-3.57675124888194,-36.6772905525626));
#15833=CARTESIAN_POINT('Ctrl Pts',(-1.52976325021857,-3.62330145009778,
-36.6712193310248));
#15834=CARTESIAN_POINT('Ctrl Pts',(-1.41950735830614,-3.66985165131363,
-36.6651481094871));
#15835=CARTESIAN_POINT('Ctrl Pts',(-1.30727193294276,-3.71130270770446,
-36.6590768879493));
#15836=CARTESIAN_POINT('Ctrl Pts',(-1.19357347707007,-3.74751535751821,
-36.6530056664116));
#15837=CARTESIAN_POINT('Ctrl Pts',(-1.08336942808624,-3.78261504821566,
-36.6471210377189));
#15838=CARTESIAN_POINT('Ctrl Pts',(-0.971440620823848,-3.81290523254181,
-36.6412364090263));
#15839=CARTESIAN_POINT('Ctrl Pts',(-0.85824376992436,-3.83821659516318,
-36.6353517803337));
#15840=CARTESIAN_POINT('Ctrl Pts',(-0.745188749241536,-3.86349624386304,
-36.6294745247981));
#15841=CARTESIAN_POINT('Ctrl Pts',(-0.630869242885877,-3.88380938917106,
-36.6235972692625));
#15842=CARTESIAN_POINT('Ctrl Pts',(-0.515758335612414,-3.89903607821809,
-36.617720013727));
#15843=CARTESIAN_POINT('Ctrl Pts',(-0.400761259595107,-3.91424770984631,
-36.6118485701114));
#15844=CARTESIAN_POINT('Ctrl Pts',(-0.284974745011976,-3.92438283772759,
-36.6059771264958));
#15845=CARTESIAN_POINT('Ctrl Pts',(-0.168882685058675,-3.92937242300693,
-36.6001056828802));
#15846=CARTESIAN_POINT('Ctrl Pts',(-0.0513338740589549,-3.93442461880055,
-36.5941605629802));
#15847=CARTESIAN_POINT('Ctrl Pts',(0.0665277857892527,-3.9342011533646,
-36.5882154430801));
#15848=CARTESIAN_POINT('Ctrl Pts',(0.184193531576616,-3.9286844799405,-36.5822703231801));
#15849=CARTESIAN_POINT('Ctrl Pts',(0.300275472207089,-3.92324206207615,
-36.5764052258175));
#15850=CARTESIAN_POINT('Ctrl Pts',(0.41616631817684,-3.91264808560998,-36.570540128455));
#15851=CARTESIAN_POINT('Ctrl Pts',(0.531377618227846,-3.89693813484978,
-36.5646750310925));
#15852=CARTESIAN_POINT('Ctrl Pts',(0.646573522784248,-3.8812302833842,-36.5588107174732));
#15853=CARTESIAN_POINT('Ctrl Pts',(0.761089654624889,-3.86040787282167,
-36.5529464038538));
#15854=CARTESIAN_POINT('Ctrl Pts',(0.874443976543163,-3.83455821860712,
-36.5470820902345));
#15855=CARTESIAN_POINT('Ctrl Pts',(0.987810256284547,-3.80870583749528,
-36.5412171579848));
#15856=CARTESIAN_POINT('Ctrl Pts',(1.10001408148965,-3.77782524991446,-36.5353522257352));
#15857=CARTESIAN_POINT('Ctrl Pts',(1.21058554890604,-3.74205446630322,-36.5294872934855));
#15858=CARTESIAN_POINT('Ctrl Pts',(1.32380476256398,-3.70542711489852,-36.5234819194683));
#15859=CARTESIAN_POINT('Ctrl Pts',(1.43531201249615,-3.66367251754737,-36.5174765454511));
#15860=CARTESIAN_POINT('Ctrl Pts',(1.54462259819798,-3.61699184808815,-36.5114711714339));
#15861=CARTESIAN_POINT('Ctrl Pts',(1.65153290144412,-3.57133621011333,-36.5055976656507));
#15862=CARTESIAN_POINT('Ctrl Pts',(1.75634166794661,-3.52096884273536,-36.4997241598675));
#15863=CARTESIAN_POINT('Ctrl Pts',(1.85861966962177,-3.46612491461215,-36.4938506540843));
#15864=CARTESIAN_POINT('Ctrl Pts',(1.96434209272642,-3.40943400475082,-36.4877793459501));
#15865=CARTESIAN_POINT('Ctrl Pts',(2.06735987213064,-3.34795995271331,-36.4817080378159));
#15866=CARTESIAN_POINT('Ctrl Pts',(2.16723180649855,-3.28201086178901,-36.4756367296817));
#15867=CARTESIAN_POINT('Ctrl Pts',(2.26710374086646,-3.2160617708647,-36.4695654215475));
#15868=CARTESIAN_POINT('Ctrl Pts',(2.36382948129902,-3.14563797486531,-36.4634941134134));
#15869=CARTESIAN_POINT('Ctrl Pts',(2.45700674411374,-3.07109212811657,-36.4574228052792));
#15870=CARTESIAN_POINT('Ctrl Pts',(2.54629870464434,-2.99965469150884,-36.4516046583417));
#15871=CARTESIAN_POINT('Ctrl Pts',(2.63263057261756,-2.92419311716659,-36.4457865114042));
#15872=CARTESIAN_POINT('Ctrl Pts',(2.71561293937094,-2.84498424662091,-36.4399683644668));
#15873=CARTESIAN_POINT('Ctrl Pts',(2.79849071779156,-2.76587520841352,-36.4341575505364));
#15874=CARTESIAN_POINT('Ctrl Pts',(2.8780270851052,-2.68302855163472,-36.4283467366061));
#15875=CARTESIAN_POINT('Ctrl Pts',(2.95386421551895,-2.59676244509902,-36.4225359226758));
#15876=CARTESIAN_POINT('Ctrl Pts',(3.03182913555492,-2.50807593941009,-36.4165620726507));
#15877=CARTESIAN_POINT('Ctrl Pts',(3.10588379397672,-2.4157755201198,-36.4105882226257));
#15878=CARTESIAN_POINT('Ctrl Pts',(3.17567818472388,-2.32024935450241,-36.4046143726006));
#15879=CARTESIAN_POINT('Ctrl Pts',(3.24345393473171,-2.22748606148154,-36.3988133023205));
#15880=CARTESIAN_POINT('Ctrl Pts',(3.30721219521597,-2.13168141618424,-36.3930122320404));
#15881=CARTESIAN_POINT('Ctrl Pts',(3.36667258369661,-2.03322520006654,-36.3872111617603));
#15882=CARTESIAN_POINT('Ctrl Pts',(3.42611307370171,-1.93480193241516,-36.3814120328139));
#15883=CARTESIAN_POINT('Ctrl Pts',(3.48125833276999,-1.83372921829553,-36.3756129038674));
#15884=CARTESIAN_POINT('Ctrl Pts',(3.53187167650335,-1.73042522540368,-36.369813774921));
#15885=CARTESIAN_POINT('Ctrl Pts',(3.58248089321154,-1.6271296559462,-36.3640151188371));
#15886=CARTESIAN_POINT('Ctrl Pts',(3.62855874456104,-1.52160354849334,-36.3582164627531));
#15887=CARTESIAN_POINT('Ctrl Pts',(3.66991520746485,-1.41428829098534,-36.3524178066691));
#15888=CARTESIAN_POINT('Ctrl Pts',(3.7134531419379,-1.30131236603235,-36.3463132829529));
#15889=CARTESIAN_POINT('Ctrl Pts',(3.7517578077341,-1.18635386797593,-36.3402087592367));
#15890=CARTESIAN_POINT('Ctrl Pts',(3.78466629066775,-1.06994862880571,-36.3341042355205));
#15891=CARTESIAN_POINT('Ctrl Pts',(3.81596056636101,-0.959253229869264,
-36.3282991472539));
#15892=CARTESIAN_POINT('Ctrl Pts',(3.84237541622021,-0.847250085037127,
-36.3224940589872));
#15893=CARTESIAN_POINT('Ctrl Pts',(3.86382307213103,-0.734411510849277,
-36.3166889707206));
#15894=CARTESIAN_POINT('Ctrl Pts',(3.88528287947158,-0.62150900659791,-36.3108805935107));
#15895=CARTESIAN_POINT('Ctrl Pts',(3.90176983066044,-0.507770547286545,
-36.3050722163009));
#15896=CARTESIAN_POINT('Ctrl Pts',(3.9132479705996,-0.39367412995792,-36.299263839091));
#15897=CARTESIAN_POINT('Ctrl Pts',(3.92474076857546,-0.279432007011314,
-36.2934480443547));
#15898=CARTESIAN_POINT('Ctrl Pts',(3.93121197153682,-0.164831433445106,
-36.2876322496185));
#15899=CARTESIAN_POINT('Ctrl Pts',(3.93267768806338,-0.0503507875654495,
-36.2818164548822));
#15900=CARTESIAN_POINT('Ctrl Pts',(3.93290055513694,-0.032943624540109,
-36.2809321439463));
#15901=CARTESIAN_POINT('Ctrl Pts',(3.93300779193799,-0.0155392245317547,
-36.2800478330105));
#15902=CARTESIAN_POINT('Ctrl Pts',(3.93299955983151,0.00186074317507913,
-36.2791635220746));
#15903=CARTESIAN_POINT('',(3.93270531513622,-0.00309687980344829,-35.0291635502465));
#15904=CARTESIAN_POINT('Ctrl Pts',(3.93299955983114,0.0018607439544177,
-36.279163522035));
#15905=CARTESIAN_POINT('Ctrl Pts',(3.93294580438091,0.1154820520235,-36.2733889960723));
#15906=CARTESIAN_POINT('Ctrl Pts',(3.92796871631761,0.22897989575827,-36.2676144701095));
#15907=CARTESIAN_POINT('Ctrl Pts',(3.91809833470597,0.34204449940656,-36.2618399441467));
#15908=CARTESIAN_POINT('Ctrl Pts',(3.90803975391883,0.457264912832259,-36.2559553149409));
#15909=CARTESIAN_POINT('Ctrl Pts',(3.89287842309005,0.572224409020614,-36.2500706857351));
#15910=CARTESIAN_POINT('Ctrl Pts',(3.87263401463472,0.686436296166057,-36.2441860565294));
#15911=CARTESIAN_POINT('Ctrl Pts',(3.85241497185978,0.800505078995474,-36.2383088006002));
#15912=CARTESIAN_POINT('Ctrl Pts',(3.82712558994851,0.913827714317787,-36.2324315446711));
#15913=CARTESIAN_POINT('Ctrl Pts',(3.79683740043307,1.02592141739639,-36.226554288742));
#15914=CARTESIAN_POINT('Ctrl Pts',(3.76657916301714,1.13790427060902,-36.2206828448524));
#15915=CARTESIAN_POINT('Ctrl Pts',(3.73133205862219,1.24866021433365,-36.2148114009628));
#15916=CARTESIAN_POINT('Ctrl Pts',(3.6912187674152,1.35771610106155,-36.2089399570732));
#15917=CARTESIAN_POINT('Ctrl Pts',(3.65060212790096,1.46814043935075,-36.2029948373208));
#15918=CARTESIAN_POINT('Ctrl Pts',(3.60499641086151,1.57682134006441,-36.1970497175683));
#15919=CARTESIAN_POINT('Ctrl Pts',(3.55458139483645,1.68328253941,-36.1911045978158));
#15920=CARTESIAN_POINT('Ctrl Pts',(3.50484497427593,1.78831075127046,-36.1852395004777));
#15921=CARTESIAN_POINT('Ctrl Pts',(3.45042811731104,1.89117827149154,-36.1793744031396));
#15922=CARTESIAN_POINT('Ctrl Pts',(3.39155180991,1.99144804619558,-36.1735093058015));
#15923=CARTESIAN_POINT('Ctrl Pts',(3.3326833711807,2.09170442009413,-36.167644992319));
#15924=CARTESIAN_POINT('Ctrl Pts',(3.26935687554114,2.18936338440196,-36.1617806788365));
#15925=CARTESIAN_POINT('Ctrl Pts',(3.20183857770775,2.28401373076048,-36.155916365354));
#15926=CARTESIAN_POINT('Ctrl Pts',(3.13431315862322,2.37867406002599,-36.150051433354));
#15927=CARTESIAN_POINT('Ctrl Pts',(3.06259529728359,2.4703248057144,-36.1441865013541));
#15928=CARTESIAN_POINT('Ctrl Pts',(2.98699335770534,2.55858548440817,-36.1383215693541));
#15929=CARTESIAN_POINT('Ctrl Pts',(2.90958105150426,2.64895965632323,-36.1323161954925));
#15930=CARTESIAN_POINT('Ctrl Pts',(2.82809657227961,2.73577898797125,-36.1263108216309));
#15931=CARTESIAN_POINT('Ctrl Pts',(2.74291227337743,2.81867367046195,-36.1203054477693));
#15932=CARTESIAN_POINT('Ctrl Pts',(2.65959848831895,2.89974811550085,-36.1144319425159));
#15933=CARTESIAN_POINT('Ctrl Pts',(2.57274604487698,2.97706826223606,-36.1085584372626));
#15934=CARTESIAN_POINT('Ctrl Pts',(2.48273730049492,3.05032858832146,-36.1026849320093));
#15935=CARTESIAN_POINT('Ctrl Pts',(2.38969731820365,3.1260561133351,-36.0966136238435));
#15936=CARTESIAN_POINT('Ctrl Pts',(2.29328508670429,3.19744526217168,-36.0905423156778));
#15937=CARTESIAN_POINT('Ctrl Pts',(2.19395488236274,3.26420755684388,-36.084471007512));
#15938=CARTESIAN_POINT('Ctrl Pts',(2.0946246780212,3.33096985151608,-36.0783996993462));
#15939=CARTESIAN_POINT('Ctrl Pts',(1.99237694328402,3.39310509862785,-36.0723283911805));
#15940=CARTESIAN_POINT('Ctrl Pts',(1.88769207713821,3.45037789552241,-36.0662570830147));
#15941=CARTESIAN_POINT('Ctrl Pts',(1.78622613205874,3.50588962972243,-36.0603724595386));
#15942=CARTESIAN_POINT('Ctrl Pts',(1.68214816344238,3.55701008158881,-36.0544878360626));
#15943=CARTESIAN_POINT('Ctrl Pts',(1.57587411384908,3.6034857814761,-36.0486032125865));
#15944=CARTESIAN_POINT('Ctrl Pts',(1.46973322370741,3.64990324815655,-36.0427259624367));
#15945=CARTESIAN_POINT('Ctrl Pts',(1.36140209902872,3.69168737452847,-36.0368487122868));
#15946=CARTESIAN_POINT('Ctrl Pts',(1.25132218365477,3.72863001552761,-36.0309714621369));
#15947=CARTESIAN_POINT('Ctrl Pts',(1.1413511275954,3.7655361235174,-36.0251000240684));
#15948=CARTESIAN_POINT('Ctrl Pts',(1.02963510896131,3.79761014051247,-36.0192285859999));
#15949=CARTESIAN_POINT('Ctrl Pts',(0.916635910175047,3.82469183179215,-36.0133571479314));
#15950=CARTESIAN_POINT('Ctrl Pts',(0.802218623360296,3.85211338585499,-36.0074120260127));
#15951=CARTESIAN_POINT('Ctrl Pts',(0.686486119662203,3.87441627606722,-36.0014669040939));
#15952=CARTESIAN_POINT('Ctrl Pts',(0.569934434622809,3.89148605808002,-35.9955217821752));
#15953=CARTESIAN_POINT('Ctrl Pts',(0.454951714153902,3.9083260546273,-35.9896566907224));
#15954=CARTESIAN_POINT('Ctrl Pts',(0.339172151849051,3.92007291688466,-35.9837915992696));
#15955=CARTESIAN_POINT('Ctrl Pts',(0.223081996925893,3.92666823434926,-35.9779265078168));
#15956=CARTESIAN_POINT('Ctrl Pts',(0.107007357442921,3.9332626703502,-35.972062200233));
#15957=CARTESIAN_POINT('Ctrl Pts',(-0.00937738159519706,3.93470690755665,
-35.9661978926492));
#15958=CARTESIAN_POINT('Ctrl Pts',(-0.125582381397877,3.93099453897896,
-35.9603335850654));
#15959=CARTESIAN_POINT('Ctrl Pts',(-0.241799637389512,3.92728177885624,
-35.9544686589707));
#15960=CARTESIAN_POINT('Ctrl Pts',(-0.357836705402596,3.91841134490497,
-35.948603732876));
#15961=CARTESIAN_POINT('Ctrl Pts',(-0.473205969581352,3.90442890962975,
-35.9427388067813));
#15962=CARTESIAN_POINT('Ctrl Pts',(-0.591338150602947,3.89011161648575,
-35.9367334247064));
#15963=CARTESIAN_POINT('Ctrl Pts',(-0.708769683599898,3.87043440316512,
-35.9307280426314));
#15964=CARTESIAN_POINT('Ctrl Pts',(-0.824986354483205,3.84550211479808,
-35.9247226605565));
#15965=CARTESIAN_POINT('Ctrl Pts',(-0.938650820224721,3.82111735815849,
-35.9188491611701));
#15966=CARTESIAN_POINT('Ctrl Pts',(-1.0511528452843,3.79170612251139,-35.9129756617836));
#15967=CARTESIAN_POINT('Ctrl Pts',(-1.16202617332701,3.75741722097813,-35.9071021623973));
#15968=CARTESIAN_POINT('Ctrl Pts',(-1.27663380139134,3.72197344254167,-35.901030838978));
#15969=CARTESIAN_POINT('Ctrl Pts',(-1.38950063021121,3.6813178026479,-35.8949595155588));
#15970=CARTESIAN_POINT('Ctrl Pts',(-1.50013470844846,3.63566841949431,-35.8888881921396));
#15971=CARTESIAN_POINT('Ctrl Pts',(-1.61076878668571,3.59001903634072,-35.8828168687204));
#15972=CARTESIAN_POINT('Ctrl Pts',(-1.71916970807392,3.53937617092121,-35.8767455453012));
#15973=CARTESIAN_POINT('Ctrl Pts',(-1.8248752088951,3.48400910905239,-35.870674221882));
#15974=CARTESIAN_POINT('Ctrl Pts',(-1.92733012257181,3.43034465923442,-35.8647895998709));
#15975=CARTESIAN_POINT('Ctrl Pts',(-2.02757871867464,3.37207172169912,-35.8589049778599));
#15976=CARTESIAN_POINT('Ctrl Pts',(-2.1251794386981,3.30939591970118,-35.8530203558489));
#15977=CARTESIAN_POINT('Ctrl Pts',(-2.22265786611653,3.24679864977858,-35.8471431072031));
#15978=CARTESIAN_POINT('Ctrl Pts',(-2.31749467305084,3.17980970808052,-35.8412658585573));
#15979=CARTESIAN_POINT('Ctrl Pts',(-2.40927188222961,3.10868107040555,-35.8353886099115));
#15980=CARTESIAN_POINT('Ctrl Pts',(-2.50095833125454,3.03762277313595,-35.829517173384));
#15981=CARTESIAN_POINT('Ctrl Pts',(-2.58959087832125,2.9624331744105,-35.8236457368564));
#15982=CARTESIAN_POINT('Ctrl Pts',(-2.67478014173756,2.88340773970079,-35.8177743003289));
#15983=CARTESIAN_POINT('Ctrl Pts',(-2.76103852208886,2.8033905435043,-35.8118291778464));
#15984=CARTESIAN_POINT('Ctrl Pts',(-2.84376623716277,2.71944079991931,-35.8058840553639));
#15985=CARTESIAN_POINT('Ctrl Pts',(-2.92259302138893,2.63190786908066,-35.7999389328815));
#15986=CARTESIAN_POINT('Ctrl Pts',(-3.00035864723054,2.54555329791248,-35.7940738430508));
#15987=CARTESIAN_POINT('Ctrl Pts',(-3.07432744876471,2.45571174070017,-35.78820875322));
#15988=CARTESIAN_POINT('Ctrl Pts',(-3.1441812194431,2.36275548021824,-35.7823436633893));
#15989=CARTESIAN_POINT('Ctrl Pts',(-3.21402565383958,2.26981164377361,-35.7764793574551));
#15990=CARTESIAN_POINT('Ctrl Pts',(-3.2797559042162,2.17375426070261,-35.770615051521));
#15991=CARTESIAN_POINT('Ctrl Pts',(-3.34109505236939,2.07498743394576,-35.7647507455869));
#15992=CARTESIAN_POINT('Ctrl Pts',(-3.40244066971976,1.97621019064259,-35.7588858211676));
#15993=CARTESIAN_POINT('Ctrl Pts',(-3.4593940472322,1.87472328496582,-35.7530208967483));
#15994=CARTESIAN_POINT('Ctrl Pts',(-3.51172284097113,1.77095784484036,-35.747155972329));
#15995=CARTESIAN_POINT('Ctrl Pts',(-3.56530486416553,1.66470731196324,-35.7411505880307));
#15996=CARTESIAN_POINT('Ctrl Pts',(-3.61403776324045,1.55606811915416,-35.7351452037325));
#15997=CARTESIAN_POINT('Ctrl Pts',(-3.6577236916246,1.44552633864904,-35.7291398194342));
#15998=CARTESIAN_POINT('Ctrl Pts',(-3.7004502159369,1.33741221021058,-35.7232663217722));
#15999=CARTESIAN_POINT('Ctrl Pts',(-3.73834908375054,1.2274786129651,-35.7173928241103));
#16000=CARTESIAN_POINT('Ctrl Pts',(-3.77128562979908,1.11619608423921,-35.7115193264483));
#16001=CARTESIAN_POINT('Ctrl Pts',(-3.80533153789732,1.00116535999881,-35.7054479988319));
#16002=CARTESIAN_POINT('Ctrl Pts',(-3.83407483448959,0.884693704268451,
-35.6993766712155));
#16003=CARTESIAN_POINT('Ctrl Pts',(-3.85742428506768,0.767311465423337,
-35.693305343599));
#16004=CARTESIAN_POINT('Ctrl Pts',(-3.88077373564577,0.649929226578227,
-35.6872340159826));
#16005=CARTESIAN_POINT('Ctrl Pts',(-3.89872933216462,0.53163688743102,-35.6811626883662));
#16006=CARTESIAN_POINT('Ctrl Pts',(-3.91125888325936,0.412968458995048,
-35.6750913607497));
#16007=CARTESIAN_POINT('Ctrl Pts',(-3.92340313000817,0.297949280309227,
-35.6692067364636));
#16008=CARTESIAN_POINT('Ctrl Pts',(-3.93048880854725,0.18221112392774,-35.6633221121774));
#16009=CARTESIAN_POINT('Ctrl Pts',(-3.93244222618923,0.0662354714927022,
-35.6574374878913));
#16010=CARTESIAN_POINT('Ctrl Pts',(-3.93439319623325,-0.0495948654887856,
-35.6515602369359));
#16011=CARTESIAN_POINT('Ctrl Pts',(-3.93122468849843,-0.165661698915492,
-35.6456829859805));
#16012=CARTESIAN_POINT('Ctrl Pts',(-3.92291466037067,-0.28147747236472,
-35.6398057350251));
#16013=CARTESIAN_POINT('Ctrl Pts',(-3.91461285013363,-0.397178714147654,
-35.6339342961567));
#16014=CARTESIAN_POINT('Ctrl Pts',(-3.90117966355049,-0.512628981876277,
-35.6280628572882));
#16015=CARTESIAN_POINT('Ctrl Pts',(-3.88264510567778,-0.627340404689822,
-35.6221914184198));
#16016=CARTESIAN_POINT('Ctrl Pts',(-3.86387795112926,-0.743491381433198,
-35.616246296803));
#16017=CARTESIAN_POINT('Ctrl Pts',(-3.83988049751041,-0.858884413607845,
-35.6103011751863));
#16018=CARTESIAN_POINT('Ctrl Pts',(-3.81073820089442,-0.973017658752366,
-35.6043560535695));
#16019=CARTESIAN_POINT('Ctrl Pts',(-3.78198819903342,-1.08561451594403,
-35.5984909613361));
#16020=CARTESIAN_POINT('Ctrl Pts',(-3.74823113030102,-1.19698488693604,
-35.5926258691027));
#16021=CARTESIAN_POINT('Ctrl Pts',(-3.70960039123802,-1.30665754401324,
-35.5867607768693));
#16022=CARTESIAN_POINT('Ctrl Pts',(-3.67097481522704,-1.41631554318725,
-35.5808964685136));
#16023=CARTESIAN_POINT('Ctrl Pts',(-3.62747700096022,-1.5242758919045,-35.5750321601579));
#16024=CARTESIAN_POINT('Ctrl Pts',(-3.57928971837202,-1.63008408125358,
-35.5691678518023));
#16025=CARTESIAN_POINT('Ctrl Pts',(-3.53109735353148,-1.73590343005989,
-35.5633029249453));
#16026=CARTESIAN_POINT('Ctrl Pts',(-3.47821470760771,-1.83956979398554,
-35.5574379980884));
#16027=CARTESIAN_POINT('Ctrl Pts',(-3.42087175511027,-1.94065077618019,
-35.5515730712315));
#16028=CARTESIAN_POINT('Ctrl Pts',(-3.36215554534861,-2.04415246025761,
-35.5455676902637));
#16029=CARTESIAN_POINT('Ctrl Pts',(-3.29876289481269,-2.14494295784491,
-35.5395623092958));
#16030=CARTESIAN_POINT('Ctrl Pts',(-3.23098862981859,-2.24258811955806,
-35.533556928328));
#16031=CARTESIAN_POINT('Ctrl Pts',(-3.16470271797934,-2.33808894987192,
-35.5276834282106));
#16032=CARTESIAN_POINT('Ctrl Pts',(-3.09422595330723,-2.43058087239799,
-35.5218099280933));
#16033=CARTESIAN_POINT('Ctrl Pts',(-3.01987526464141,-2.51969093065141,
-35.5159364279759));
#16034=CARTESIAN_POINT('Ctrl Pts',(-2.94302042209953,-2.61180224285117,
-35.5098651065828));
#16035=CARTESIAN_POINT('Ctrl Pts',(-2.86202643257968,-2.70029951224006,
-35.5037937851897));
#16036=CARTESIAN_POINT('Ctrl Pts',(-2.77728407914598,-2.78481276636729,
-35.4977224637966));
#16037=CARTESIAN_POINT('Ctrl Pts',(-2.69254172571229,-2.86932602049453,
-35.4916511424035));
#16038=CARTESIAN_POINT('Ctrl Pts',(-2.60405140570917,-2.9498549849764,-35.4855798210104));
#16039=CARTESIAN_POINT('Ctrl Pts',(-2.51223968600886,-3.02607679348064,
-35.4795084996174));
#16040=CARTESIAN_POINT('Ctrl Pts',(-2.4232512504495,-3.09995472013793,-35.4736238762347));
#16041=CARTESIAN_POINT('Ctrl Pts',(-2.3308597938181,-3.17002141713106,-35.4677392528521));
#16042=CARTESIAN_POINT('Ctrl Pts',(-2.23542515827695,-3.23594860307491,
-35.4618546294694));
#16043=CARTESIAN_POINT('Ctrl Pts',(-2.14011010082685,-3.30179318329602,
-35.4559773794269));
#16044=CARTESIAN_POINT('Ctrl Pts',(-2.04175978384362,-3.36350833667166,
-35.4501001293844));
#16045=CARTESIAN_POINT('Ctrl Pts',(-1.9407677419334,-3.42080539812933,-35.4442228793419));
#16046=CARTESIAN_POINT('Ctrl Pts',(-1.83987557247139,-3.47804579771845,
-35.4383514413945));
#16047=CARTESIAN_POINT('Ctrl Pts',(-1.73634723084554,-3.53087659515673,
-35.4324800034471));
#16048=CARTESIAN_POINT('Ctrl Pts',(-1.6306053706547,-3.5790522663398,-35.4266085654997));
#16049=CARTESIAN_POINT('Ctrl Pts',(-1.52353649576712,-3.62783252139882,
-35.4206634435408));
#16050=CARTESIAN_POINT('Ctrl Pts',(-1.4141985138439,-3.67183976181265,-35.4147183215818));
#16051=CARTESIAN_POINT('Ctrl Pts',(-1.30305645053974,-3.71086686458929,
-35.4087731996229));
#16052=CARTESIAN_POINT('Ctrl Pts',(-1.19341053362311,-3.74936860138749,
-35.4029081083245));
#16053=CARTESIAN_POINT('Ctrl Pts',(-1.08200921092332,-3.78302332655099,
-35.3970430170261));
#16054=CARTESIAN_POINT('Ctrl Pts',(-0.96931860959011,-3.81168078845833,
-35.3911779257277));
#16055=CARTESIAN_POINT('Ctrl Pts',(-0.856643069582972,-3.8403344202381,
-35.3853136183106));
#16056=CARTESIAN_POINT('Ctrl Pts',(-0.742678992132058,-3.86399201575787,
-35.3794493108935));
#16057=CARTESIAN_POINT('Ctrl Pts',(-0.627905965179305,-3.88255368268003,
-35.3735850034764));
#16058=CARTESIAN_POINT('Ctrl Pts',(-0.513120833305429,-3.90111730727047,
-35.3677200775605));
#16059=CARTESIAN_POINT('Ctrl Pts',(-0.397526988314185,-3.9145838691709,
-35.3618551516446));
#16060=CARTESIAN_POINT('Ctrl Pts',(-0.281611788061173,-3.92290502062247,
-35.3559902257287));
#16061=CARTESIAN_POINT('Ctrl Pts',(-0.162920589154323,-3.93142545141944,
-35.3499848434584));
#16062=CARTESIAN_POINT('Ctrl Pts',(-0.0438928990445518,-3.93455084456753,
-35.3439794611881));
#16063=CARTESIAN_POINT('Ctrl Pts',(0.0749465089043309,-3.93228585186823,
-35.3379740789177));
#16064=CARTESIAN_POINT('Ctrl Pts',(0.191176106553475,-3.93007060025548,
-35.3321005797389));
#16065=CARTESIAN_POINT('Ctrl Pts',(0.307225195050442,-3.92269936432258,
-35.32622708056));
#16066=CARTESIAN_POINT('Ctrl Pts',(0.422607673289962,-3.91022911790044,
-35.3203535813811));
#16067=CARTESIAN_POINT('Ctrl Pts',(0.541876335249591,-3.89733886257079,
-35.3142822575651));
#16068=CARTESIAN_POINT('Ctrl Pts',(0.660432211828677,-3.87900013685128,
-35.308210933749));
#16069=CARTESIAN_POINT('Ctrl Pts',(0.77775073672986,-3.85533303250396,-35.302139609933));
#16070=CARTESIAN_POINT('Ctrl Pts',(0.895069261631039,-3.83166592815663,
-35.296068286117));
#16071=CARTESIAN_POINT('Ctrl Pts',(1.01114998620073,-3.80267062373241,-35.289996962301));
#16072=CARTESIAN_POINT('Ctrl Pts',(1.12548770706434,-3.76852310875853,-35.283925638485));
#16073=CARTESIAN_POINT('Ctrl Pts',(1.23630940586834,-3.73542567082854,-35.2780410151586));
#16074=CARTESIAN_POINT('Ctrl Pts',(1.345846078771,-3.69738306041137,-35.2721563918322));
#16075=CARTESIAN_POINT('Ctrl Pts',(1.4536250113728,-3.65451273445742,-35.2662717685058));
#16076=CARTESIAN_POINT('Ctrl Pts',(1.56126889860917,-3.61169612437071,-35.2603945185231));
#16077=CARTESIAN_POINT('Ctrl Pts',(1.66715904704408,-3.56406398053053,-35.2545172685403));
#16078=CARTESIAN_POINT('Ctrl Pts',(1.77083703148471,-3.5117837644027,-35.2486400185576));
#16079=CARTESIAN_POINT('Ctrl Pts',(1.87441248724979,-3.45955524894543,-35.2427685806733));
#16080=CARTESIAN_POINT('Ctrl Pts',(1.9757797657369,-3.40268798941228,-35.236897142789));
#16081=CARTESIAN_POINT('Ctrl Pts',(2.07450019996574,-3.34139759985879,-35.2310257049048));
#16082=CARTESIAN_POINT('Ctrl Pts',(2.17445953447812,-3.27933804147426,-35.2250805829234));
#16083=CARTESIAN_POINT('Ctrl Pts',(2.27170473558523,-3.21274372887598,-35.2191354609421));
#16084=CARTESIAN_POINT('Ctrl Pts',(2.36580560185385,-3.14188683027205,-35.2131903389607));
#16085=CARTESIAN_POINT('Ctrl Pts',(2.45863972148375,-3.07198377770266,-35.2073252477335));
#16086=CARTESIAN_POINT('Ctrl Pts',(2.5484133093192,-2.99793245860549,-35.2014601565062));
#16087=CARTESIAN_POINT('Ctrl Pts',(2.63474288294348,-2.9200374896187,-35.1955950652789));
#16088=CARTESIAN_POINT('Ctrl Pts',(2.72106091840379,-2.84215293148982,-35.1897307579358));
#16089=CARTESIAN_POINT('Ctrl Pts',(2.8039355498467,-2.76042602060623,-35.1838664505927));
#16090=CARTESIAN_POINT('Ctrl Pts',(2.88301774185246,-2.67520049718968,-35.1780021432496));
#16091=CARTESIAN_POINT('Ctrl Pts',(2.96210827448838,-2.58996598521892,-35.1721372174105));
#16092=CARTESIAN_POINT('Ctrl Pts',(3.03740529281105,-2.50123242865741,-35.1662722915714));
#16093=CARTESIAN_POINT('Ctrl Pts',(3.108598350078,-2.40937861240037,-35.1604073657323));
#16094=CARTESIAN_POINT('Ctrl Pts',(3.18149637851831,-2.31532502955241,-35.1544019833673));
#16095=CARTESIAN_POINT('Ctrl Pts',(3.25009109191741,-2.21800018708156,-35.1483966010023));
#16096=CARTESIAN_POINT('Ctrl Pts',(3.31409540635905,-2.11784339306518,-35.1423912186373));
#16097=CARTESIAN_POINT('Ctrl Pts',(3.37669413199414,-2.01988612684309,-35.1365177195416));
#16098=CARTESIAN_POINT('Ctrl Pts',(3.43490184314894,-1.91922040189029,-35.1306442204458));
#16099=CARTESIAN_POINT('Ctrl Pts',(3.48849644101194,-1.81628235168628,-35.12477072135));
#16100=CARTESIAN_POINT('Ctrl Pts',(3.54389615469999,-1.70987725236104,-35.1186993973504));
#16101=CARTESIAN_POINT('Ctrl Pts',(3.59436632447562,-1.60104450114051,-35.1126280733509));
#16102=CARTESIAN_POINT('Ctrl Pts',(3.63971605311705,-1.49028723831416,-35.1065567493513));
#16103=CARTESIAN_POINT('Ctrl Pts',(3.68506578175848,-1.37952997548781,-35.1004854253517));
#16104=CARTESIAN_POINT('Ctrl Pts',(3.72529496910861,-1.26684867343169,-35.0944141013522));
#16105=CARTESIAN_POINT('Ctrl Pts',(3.76026997298341,-1.15276135009782,-35.0883427773526));
#16106=CARTESIAN_POINT('Ctrl Pts',(3.80113461351723,-1.01946222383631,-35.0812490691233));
#16107=CARTESIAN_POINT('Ctrl Pts',(3.83493313330237,-0.88390402157618,-35.074155360894));
#16108=CARTESIAN_POINT('Ctrl Pts',(3.86145381695015,-0.746768651967352,
-35.0670616526647));
#16109=CARTESIAN_POINT('Ctrl Pts',(3.8876819604404,-0.611145973477642,-35.0600461925888));
#16110=CARTESIAN_POINT('Ctrl Pts',(3.9067919115526,-0.473980755150574,-35.0530307325129));
#16111=CARTESIAN_POINT('Ctrl Pts',(3.91862537579101,-0.33595262196737,-35.046015272437));
#16112=CARTESIAN_POINT('Ctrl Pts',(3.92810036406333,-0.225434271904183,
-35.0403980330044));
#16113=CARTESIAN_POINT('Ctrl Pts',(3.93291115998635,-0.114363079279912,
-35.0347807935718));
#16114=CARTESIAN_POINT('Ctrl Pts',(3.93299878050155,-0.00309718796439099,
-35.0291635541393));
#16115=CARTESIAN_POINT('',(3.93264515487443,0.00306832688220754,-33.7791634933578));
#16116=CARTESIAN_POINT('Ctrl Pts',(3.93057853514731,-0.0030946465227831,
-35.029163522035));
#16117=CARTESIAN_POINT('Ctrl Pts',(3.92365169001617,0.896981560524963,-34.9836956534301));
#16118=CARTESIAN_POINT('Ctrl Pts',(3.17394638211024,3.09807182351393,-34.8730334977809));
#16119=CARTESIAN_POINT('Ctrl Pts',(-0.452408180865259,4.60400171736557,
-34.697177055088));
#16120=CARTESIAN_POINT('Ctrl Pts',(-4.08239314255048,2.17613677140805,-34.5015941939554));
#16121=CARTESIAN_POINT('Ctrl Pts',(-4.07447403678864,-2.19092822357172,
-34.3060113328231));
#16122=CARTESIAN_POINT('Ctrl Pts',(-0.435707702205553,-4.60561216169713,
-34.1104284716908));
#16123=CARTESIAN_POINT('Ctrl Pts',(3.18020937176261,-3.08861798879681,-33.9348125347613));
#16124=CARTESIAN_POINT('Ctrl Pts',(3.92364775283068,-0.892318847406521,
-33.8243908848761));
#16125=CARTESIAN_POINT('Ctrl Pts',(3.93045809296359,0.00306605271246902,
-33.779163522035));
#16126=CARTESIAN_POINT('',(3.93299959220032,-0.00179101985566553,-32.5291635219964));
#16127=CARTESIAN_POINT('Ctrl Pts',(3.9329988028365,0.00306869461550739,
-33.7791634887208));
#16128=CARTESIAN_POINT('Ctrl Pts',(3.93289100539829,0.141227504320743,-33.7721893226934));
#16129=CARTESIAN_POINT('Ctrl Pts',(3.92549945843856,0.279086805530256,-33.7652151566661));
#16130=CARTESIAN_POINT('Ctrl Pts',(3.91094177047953,0.415960897102635,-33.7582409906387));
#16131=CARTESIAN_POINT('Ctrl Pts',(3.89621992300834,0.554378446960705,-33.7511881805508));
#16132=CARTESIAN_POINT('Ctrl Pts',(3.87416947544637,0.691788396585036,-33.744135370463));
#16133=CARTESIAN_POINT('Ctrl Pts',(3.84496154579419,0.827502091455922,-33.7370825603751));
#16134=CARTESIAN_POINT('Ctrl Pts',(3.82036237760766,0.941801326119291,-33.7311426233921));
#16135=CARTESIAN_POINT('Ctrl Pts',(3.79068718235984,1.0548977358952,-33.725202686409));
#16136=CARTESIAN_POINT('Ctrl Pts',(3.75606447311104,1.16639130390838,-33.719262749426));
#16137=CARTESIAN_POINT('Ctrl Pts',(3.72176417441482,1.2768466313086,-33.7133781258025));
#16138=CARTESIAN_POINT('Ctrl Pts',(3.68253296561105,1.38596324660863,-33.707493502179));
#16139=CARTESIAN_POINT('Ctrl Pts',(3.63849343586062,1.49326974026771,-33.7016088785555));
#16140=CARTESIAN_POINT('Ctrl Pts',(3.59450908705311,1.60044178032259,-33.6957316282869));
#16141=CARTESIAN_POINT('Ctrl Pts',(3.54572855487768,1.70580783244215,-33.6898543780182));
#16142=CARTESIAN_POINT('Ctrl Pts',(3.49232427470953,1.80891131907415,-33.6839771277496));
#16143=CARTESIAN_POINT('Ctrl Pts',(3.43897280691607,1.91191284496533,-33.6781056895908));
#16144=CARTESIAN_POINT('Ctrl Pts',(3.38100687546608,2.01265589327127,-33.672234251432));
#16145=CARTESIAN_POINT('Ctrl Pts',(3.31864685067646,2.11070416697727,-33.6663628132732));
#16146=CARTESIAN_POINT('Ctrl Pts',(3.25550423767038,2.20998289920066,-33.6604176913991));
#16147=CARTESIAN_POINT('Ctrl Pts',(3.18785664584906,2.30649835847185,-33.6544725695249));
#16148=CARTESIAN_POINT('Ctrl Pts',(3.11598090425347,2.39982332773222,-33.6485274476508));
#16149=CARTESIAN_POINT('Ctrl Pts',(3.04507271968931,2.49189200066491,-33.6426623561783));
#16150=CARTESIAN_POINT('Ctrl Pts',(2.97004978649661,2.58085522413837,-33.6367972647059));
#16151=CARTESIAN_POINT('Ctrl Pts',(2.89122087237093,2.6663328500333,-33.6309321732334));
#16152=CARTESIAN_POINT('Ctrl Pts',(2.81240249407926,2.7517990514644,-33.6250678656565));
#16153=CARTESIAN_POINT('Ctrl Pts',(2.72977942529371,2.8337802795901,-33.6192035580795));
#16154=CARTESIAN_POINT('Ctrl Pts',(2.64369918049048,2.91193125658453,-33.6133392505025));
#16155=CARTESIAN_POINT('Ctrl Pts',(2.55760985715705,2.99009047584183,-33.6074743244411));
#16156=CARTESIAN_POINT('Ctrl Pts',(2.46806293747283,3.06441836447313,-33.6016093983797));
#16157=CARTESIAN_POINT('Ctrl Pts',(2.37544055899965,3.13460861203746,-33.5957444723183));
#16158=CARTESIAN_POINT('Ctrl Pts',(2.28060001730402,3.20647980785954,-33.5897390903162));
#16159=CARTESIAN_POINT('Ctrl Pts',(2.18253519374144,3.27401237963774,-33.5837337083142));
#16160=CARTESIAN_POINT('Ctrl Pts',(2.08168849136363,3.33692403643299,-33.5777283263121));
#16161=CARTESIAN_POINT('Ctrl Pts',(1.98305645856488,3.39845410583679,-33.5718548270243));
#16162=CARTESIAN_POINT('Ctrl Pts',(1.88176386432633,3.45556397466868,-33.5659813277365));
#16163=CARTESIAN_POINT('Ctrl Pts',(1.77824923092822,3.50803629865815,-33.5601078284487));
#16164=CARTESIAN_POINT('Ctrl Pts',(1.67124814333661,3.56227593175176,-33.5540365050895));
#16165=CARTESIAN_POINT('Ctrl Pts',(1.56187313987604,3.6115599207793,-33.5479651817303));
#16166=CARTESIAN_POINT('Ctrl Pts',(1.45062940626627,3.65570284975072,-33.5418938583712));
#16167=CARTESIAN_POINT('Ctrl Pts',(1.33938567265651,3.69984577872215,-33.535822535012));
#16168=CARTESIAN_POINT('Ctrl Pts',(1.22627368233417,3.73884755262167,-33.5297512116529));
#16169=CARTESIAN_POINT('Ctrl Pts',(1.11181287535345,3.77258016882323,-33.5236798882937));
#16170=CARTESIAN_POINT('Ctrl Pts',(1.00087175247158,3.80527550286691,-33.5177952588855));
#16171=CARTESIAN_POINT('Ctrl Pts',(0.888310844573323,3.83312496977567,-33.5119106294773));
#16172=CARTESIAN_POINT('Ctrl Pts',(0.774590439266641,3.85596922334667,-33.5060260000691));
#16173=CARTESIAN_POINT('Ctrl Pts',(0.661012523218186,3.87878485355199,-33.5001487439768));
#16174=CARTESIAN_POINT('Ctrl Pts',(0.546278399129095,3.89660766344188,-33.4942714878846));
#16175=CARTESIAN_POINT('Ctrl Pts',(0.4308636477164,3.90932801349241,-33.4883942317924));
#16176=CARTESIAN_POINT('Ctrl Pts',(0.315563031132705,3.92203578425857,-33.4825227877788));
#16177=CARTESIAN_POINT('Ctrl Pts',(0.199583532768558,3.92965108828396,-33.4766513437653));
#16178=CARTESIAN_POINT('Ctrl Pts',(0.0834104323618352,3.9321154229973,-33.4707798997518));
#16179=CARTESIAN_POINT('Ctrl Pts',(-0.0342204239031183,3.93461068051766,
-33.4648347800605));
#16180=CARTESIAN_POINT('Ctrl Pts',(-0.152049354966056,3.93182472315353,
-33.4588896603692));
#16181=CARTESIAN_POINT('Ctrl Pts',(-0.269567336800497,3.92375106893012,
-33.4529445406779));
#16182=CARTESIAN_POINT('Ctrl Pts',(-0.385503506534395,3.91578608747106,
-33.4470794433128));
#16183=CARTESIAN_POINT('Ctrl Pts',(-0.501136624927632,3.90267491989501,
-33.4412143459476));
#16184=CARTESIAN_POINT('Ctrl Pts',(-0.615979129770265,3.88446376114998,
-33.4353492485825));
#16185=CARTESIAN_POINT('Ctrl Pts',(-0.730806285486452,3.86625503639382,
-33.4294849351093));
#16186=CARTESIAN_POINT('Ctrl Pts',(-0.844842631716971,3.84294774051984,
-33.4236206216362));
#16187=CARTESIAN_POINT('Ctrl Pts',(-0.957608143411652,3.8146396479447,-33.417756308163));
#16188=CARTESIAN_POINT('Ctrl Pts',(-1.07038554794669,3.78632856985014,-33.4118913762087));
#16189=CARTESIAN_POINT('Ctrl Pts',(-1.18189145261582,3.75301574673305,-33.4060264442544));
#16190=CARTESIAN_POINT('Ctrl Pts',(-1.29165906555342,3.71484937223216,-33.4001615123001));
#16191=CARTESIAN_POINT('Ctrl Pts',(-1.40405517649577,3.67576906477291,-33.3941561385385));
#16192=CARTESIAN_POINT('Ctrl Pts',(-1.5146282547568,3.63159994266073,-33.388150764777));
#16193=CARTESIAN_POINT('Ctrl Pts',(-1.62289808782706,3.58255366973438,-33.3821453910154));
#16194=CARTESIAN_POINT('Ctrl Pts',(-1.72879048418896,3.53458437648332,-33.3762718858974));
#16195=CARTESIAN_POINT('Ctrl Pts',(-1.83247940080365,3.4819501569843,-33.3703983807794));
#16196=CARTESIAN_POINT('Ctrl Pts',(-1.93354082357389,3.4248954558604,-33.3645248756614));
#16197=CARTESIAN_POINT('Ctrl Pts',(-2.0380057079412,3.36591931449862,-33.3584535675781));
#16198=CARTESIAN_POINT('Ctrl Pts',(-2.13966259455587,3.30221996183034,-33.3523822594947));
#16199=CARTESIAN_POINT('Ctrl Pts',(-2.23807708431421,3.23411502032127,-33.3463109514113));
#16200=CARTESIAN_POINT('Ctrl Pts',(-2.33649157407254,3.16601007881219,-33.340239643328));
#16201=CARTESIAN_POINT('Ctrl Pts',(-2.43166332541418,3.09349988977969,-33.3341683352446));
#16202=CARTESIAN_POINT('Ctrl Pts',(-2.52319781621016,3.01694577019082,-33.3280970271613));
#16203=CARTESIAN_POINT('Ctrl Pts',(-2.61191753789585,2.94274575962916,-33.3222124173411));
#16204=CARTESIAN_POINT('Ctrl Pts',(-2.69750251298505,2.86451100509295,-33.3163278075209));
#16205=CARTESIAN_POINT('Ctrl Pts',(-2.77956492914437,2.78253621803395,-33.3104431977007));
#16206=CARTESIAN_POINT('Ctrl Pts',(-2.86152452215785,2.70066414432266,-33.3045659612205));
#16207=CARTESIAN_POINT('Ctrl Pts',(-2.93997004623968,2.61506164677989,-33.2986887247403));
#16208=CARTESIAN_POINT('Ctrl Pts',(-3.01454657687363,2.52606372363396,-33.2928114882601));
#16209=CARTESIAN_POINT('Ctrl Pts',(-3.08904935777308,2.43715381173162,-33.2869400638581));
#16210=CARTESIAN_POINT('Ctrl Pts',(-3.15969049388662,2.34485546747271,-33.2810686394561));
#16211=CARTESIAN_POINT('Ctrl Pts',(-3.22615224045201,2.24954011331794,-33.2751972150541));
#16212=CARTESIAN_POINT('Ctrl Pts',(-3.29344826604316,2.15302828743447,-33.2692520880114));
#16213=CARTESIAN_POINT('Ctrl Pts',(-3.35645894996537,2.05342348798032,-33.2633069609687));
#16214=CARTESIAN_POINT('Ctrl Pts',(-3.41489667157031,1.9511457460933,-33.257361833926));
#16215=CARTESIAN_POINT('Ctrl Pts',(-3.4725475486578,1.85024514003999,-33.2514967560448));
#16216=CARTESIAN_POINT('Ctrl Pts',(-3.525747651882,1.74674350200199,-33.2456316781637));
#16217=CARTESIAN_POINT('Ctrl Pts',(-3.57426510284596,1.64107220273135,-33.2397666002825));
#16218=CARTESIAN_POINT('Ctrl Pts',(-3.62277606993461,1.53541502538006,-33.2339023062108));
#16219=CARTESIAN_POINT('Ctrl Pts',(-3.6666054577924,1.42758913713199,-33.2280380121391));
#16220=CARTESIAN_POINT('Ctrl Pts',(-3.70556849258319,1.31804823385746,-33.2221737180673));
#16221=CARTESIAN_POINT('Ctrl Pts',(-3.74453563732704,1.20849577583688,-33.2163088054099));
#16222=CARTESIAN_POINT('Ctrl Pts',(-3.7786352707319,1.09722833064852,-33.2104438927526));
#16223=CARTESIAN_POINT('Ctrl Pts',(-3.80773191605457,0.984716535587463,
-33.2045789800952));
#16224=CARTESIAN_POINT('Ctrl Pts',(-3.83752554438897,0.869509625371121,
-33.198573578923));
#16225=CARTESIAN_POINT('Ctrl Pts',(-3.86207332821644,0.752998429117083,
-33.1925681777508));
#16226=CARTESIAN_POINT('Ctrl Pts',(-3.88128516945974,0.635699955428583,
-33.1865627765786));
#16227=CARTESIAN_POINT('Ctrl Pts',(-3.90007500252231,0.520978065361393,
-33.1806892903224));
#16228=CARTESIAN_POINT('Ctrl Pts',(-3.91376090692278,0.40550354843166,-33.1748158040662));
#16229=CARTESIAN_POINT('Ctrl Pts',(-3.92231122642181,0.289764806499083,
-33.1689423178099));
#16230=CARTESIAN_POINT('Ctrl Pts',(-3.93114959835571,0.17012693232627,-33.1628709591798));
#16231=CARTESIAN_POINT('Ctrl Pts',(-3.934500243471,0.0502072011357646,-33.1567996005496));
#16232=CARTESIAN_POINT('Ctrl Pts',(-3.93238664930414,-0.0694567518281636,
-33.1507282419194));
#16233=CARTESIAN_POINT('Ctrl Pts',(-3.93027305513729,-0.189120704792092,
-33.1446568832892));
#16234=CARTESIAN_POINT('Ctrl Pts',(-3.92269531637615,-0.308528406004927,
-33.1385855246591));
#16235=CARTESIAN_POINT('Ctrl Pts',(-3.9097353961647,-0.427151181640451,
-33.1325141660289));
#16236=CARTESIAN_POINT('Ctrl Pts',(-3.89717406651062,-0.542125638653213,
-33.1266295358801));
#16237=CARTESIAN_POINT('Ctrl Pts',(-3.87951686780026,-0.656728299452036,
-33.1207449057314));
#16238=CARTESIAN_POINT('Ctrl Pts',(-3.85679404856287,-0.770473015082302,
-33.1148602755826));
#16239=CARTESIAN_POINT('Ctrl Pts',(-3.83409970101184,-0.884075208614637,
-33.1089830188739));
#16240=CARTESIAN_POINT('Ctrl Pts',(-3.80635243691103,-0.996821195167531,
-33.1031057621651));
#16241=CARTESIAN_POINT('Ctrl Pts',(-3.77363426670775,-1.10822985933832,
-33.0972285054563));
#16242=CARTESIAN_POINT('Ctrl Pts',(-3.74094845251934,-1.21952834802034,
-33.0913570609493));
#16243=CARTESIAN_POINT('Ctrl Pts',(-3.70330162679568,-1.32949175279322,
-33.0854856164422));
#16244=CARTESIAN_POINT('Ctrl Pts',(-3.66082672701619,-1.43764970516601,
-33.0796141719352));
#16245=CARTESIAN_POINT('Ctrl Pts',(-3.61781885170795,-1.54716482476353,
-33.0736690524752));
#16246=CARTESIAN_POINT('Ctrl Pts',(-3.56986098538416,-1.6548284504036,-33.0677239330153));
#16247=CARTESIAN_POINT('Ctrl Pts',(-3.51714321807872,-1.76016833954109,
-33.0617788135554));
#16248=CARTESIAN_POINT('Ctrl Pts',(-3.46513503719965,-1.86409034322349,
-33.0559137159986));
#16249=CARTESIAN_POINT('Ctrl Pts',(-3.40849450365517,-1.9657504074155,-33.0500486184419));
#16250=CARTESIAN_POINT('Ctrl Pts',(-3.34745205280478,-2.06471638589252,
-33.0441835208851));
#16251=CARTESIAN_POINT('Ctrl Pts',(-3.28641776167668,-2.16366913529878,
-33.0383192073331));
#16252=CARTESIAN_POINT('Ctrl Pts',(-3.22098293935824,-2.25992816527032,
-33.032454893781));
#16253=CARTESIAN_POINT('Ctrl Pts',(-3.15142271737998,-2.35308815312588,
-33.0265905802289));
#16254=CARTESIAN_POINT('Ctrl Pts',(-3.0818551605482,-2.44625796433804,-33.0207256483079));
#16255=CARTESIAN_POINT('Ctrl Pts',(-3.00816158534893,-2.53632775427524,
-33.0148607163869));
#16256=CARTESIAN_POINT('Ctrl Pts',(-2.93065855470544,-2.62292383338362,
-33.0089957844659));
#16257=CARTESIAN_POINT('Ctrl Pts',(-2.85129964023448,-2.71159353801871,
-33.0029904111685));
#16258=CARTESIAN_POINT('Ctrl Pts',(-2.76794680303372,-2.79662070864973,
-32.996985037871));
#16259=CARTESIAN_POINT('Ctrl Pts',(-2.68098034811745,-2.87764371891449,
-32.9909796645736));
#16260=CARTESIAN_POINT('Ctrl Pts',(-2.59592353883439,-2.95688759217879,
-32.9851061597639));
#16261=CARTESIAN_POINT('Ctrl Pts',(-2.50741053123919,-3.03230111937766,
-32.9792326549541));
#16262=CARTESIAN_POINT('Ctrl Pts',(-2.41583023454058,-3.10358716292609,
-32.9733591501444));
#16263=CARTESIAN_POINT('Ctrl Pts',(-2.32116577711776,-3.17727391518177,
-32.9672878426031));
#16264=CARTESIAN_POINT('Ctrl Pts',(-2.22322418970466,-3.24654999930959,
-32.9612165350618));
#16265=CARTESIAN_POINT('Ctrl Pts',(-2.12246591290477,-3.3111368815797,-32.9551452275205));
#16266=CARTESIAN_POINT('Ctrl Pts',(-2.02170763610487,-3.37572376384981,
-32.9490739199792));
#16267=CARTESIAN_POINT('Ctrl Pts',(-1.91813311646427,-3.43562126052983,
-32.9430026124379));
#16268=CARTESIAN_POINT('Ctrl Pts',(-1.81222775722322,-3.49060446856267,
-32.9369313048966));
#16269=CARTESIAN_POINT('Ctrl Pts',(-1.70957815735091,-3.54389737408429,
-32.9310466424557));
#16270=CARTESIAN_POINT('Ctrl Pts',(-1.60441260888199,-3.59274317505789,
-32.9251619800147));
#16271=CARTESIAN_POINT('Ctrl Pts',(-1.49715247406656,-3.63689750603401,
-32.9192773175738));
#16272=CARTESIAN_POINT('Ctrl Pts',(-1.39002672970553,-3.68099651430692,
-32.9134000282586));
#16273=CARTESIAN_POINT('Ctrl Pts',(-1.28081199578994,-3.72041558845105,
-32.9075227389434));
#16274=CARTESIAN_POINT('Ctrl Pts',(-1.16995414392166,-3.7549562315852,-32.9016454496283));
#16275=CARTESIAN_POINT('Ctrl Pts',(-1.05920591713262,-3.78946271817855,
-32.8957739722452));
#16276=CARTESIAN_POINT('Ctrl Pts',(-0.946818195253127,-3.81910024897877,
-32.8899024948621));
#16277=CARTESIAN_POINT('Ctrl Pts',(-0.833256141587372,-3.84371866849109,
-32.884031017479));
#16278=CARTESIAN_POINT('Ctrl Pts',(-0.71826999020284,-3.86864580939349,
-32.8780859102409));
#16279=CARTESIAN_POINT('Ctrl Pts',(-0.602080246841668,-3.88842692692477,
-32.8721408030027));
#16280=CARTESIAN_POINT('Ctrl Pts',(-0.485185310360534,-3.9029583926312,
-32.8661956957646));
#16281=CARTESIAN_POINT('Ctrl Pts',(-0.369862899223941,-3.91729437426618,
-32.860330564889));
#16282=CARTESIAN_POINT('Ctrl Pts',(-0.253854572799971,-3.92652103580639,
-32.8544654340133));
#16283=CARTESIAN_POINT('Ctrl Pts',(-0.137647740870454,-3.9305905535216,
-32.8486003031376));
#16284=CARTESIAN_POINT('Ctrl Pts',(-0.021456440484935,-3.93465952732823,
-32.842735956162));
#16285=CARTESIAN_POINT('Ctrl Pts',(0.0949329017311209,-3.9335727137738,
-32.8368716091863));
#16286=CARTESIAN_POINT('Ctrl Pts',(0.211030418065854,-3.92733435839768,
-32.8310072622107));
#16287=CARTESIAN_POINT('Ctrl Pts',(0.327140177661687,-3.92109534514519,
-32.8251422968003));
#16288=CARTESIAN_POINT('Ctrl Pts',(0.442957639529098,-3.90970373216336,
-32.81927733139));
#16289=CARTESIAN_POINT('Ctrl Pts',(0.557996290726594,-3.89321578383929,
-32.8134123659797));
#16290=CARTESIAN_POINT('Ctrl Pts',(0.675788068279957,-3.87633324287516,
-32.8074070391284));
#16291=CARTESIAN_POINT('Ctrl Pts',(0.792762833562814,-3.85410738747903,
-32.8014017122771));
#16292=CARTESIAN_POINT('Ctrl Pts',(0.908408792051104,-3.8266542130854,-32.7953963854258));
#16293=CARTESIAN_POINT('Ctrl Pts',(1.02151686524768,-3.79980350684903,-32.7895228472759));
#16294=CARTESIAN_POINT('Ctrl Pts',(1.13335346959867,-3.76795272140445,-32.7836493091259));
#16295=CARTESIAN_POINT('Ctrl Pts',(1.24345568871581,-3.7312607722056,-32.777775770976));
#16296=CARTESIAN_POINT('Ctrl Pts',(1.35726356908134,-3.69333389844878,-32.771704549774));
#16297=CARTESIAN_POINT('Ctrl Pts',(1.46921780783199,-3.65023442009615,-32.7656333285721));
#16298=CARTESIAN_POINT('Ctrl Pts',(1.57883133942658,-3.60219108344414,-32.7595621073701));
#16299=CARTESIAN_POINT('Ctrl Pts',(1.68844487102117,-3.55414774679213,-32.7534908861681));
#16300=CARTESIAN_POINT('Ctrl Pts',(1.79571729501313,-3.50116082156502,-32.7474196649661));
#16301=CARTESIAN_POINT('Ctrl Pts',(1.90019233549209,-3.4435095597569,-32.7413484437642));
#16302=CARTESIAN_POINT('Ctrl Pts',(2.00145443157965,-3.38763126015519,-32.7354639321918));
#16303=CARTESIAN_POINT('Ctrl Pts',(2.10041065483412,-3.32719367701901,-32.7295794206194));
#16304=CARTESIAN_POINT('Ctrl Pts',(2.19662403138074,-3.26241197042321,-32.723694909047));
#16305=CARTESIAN_POINT('Ctrl Pts',(2.29271685043375,-3.19771143674181,-32.7178177708981));
#16306=CARTESIAN_POINT('Ctrl Pts',(2.38607332008407,-3.12867783359656,-32.7119406327492));
#16307=CARTESIAN_POINT('Ctrl Pts',(2.47628104895044,-3.05557215045054,-32.7060634946002));
#16308=CARTESIAN_POINT('Ctrl Pts',(2.56639956928246,-2.98253876322558,-32.7001921684908));
#16309=CARTESIAN_POINT('Ctrl Pts',(2.6533752255352,-2.90544156451583,-32.6943208423813));
#16310=CARTESIAN_POINT('Ctrl Pts',(2.73682515998634,-2.82458440193699,-32.6884495162718));
#16311=CARTESIAN_POINT('Ctrl Pts',(2.82132456074276,-2.74271037974974,-32.6825043523702));
#16312=CARTESIAN_POINT('Ctrl Pts',(2.90220859319854,-2.65698140870002,-32.6765591884685));
#16313=CARTESIAN_POINT('Ctrl Pts',(2.97911465530891,-2.56775483068841,-32.6706140245668));
#16314=CARTESIAN_POINT('Ctrl Pts',(3.05498347035287,-2.47973166894529,-32.6647490442508));
#16315=CARTESIAN_POINT('Ctrl Pts',(3.12698068875266,-2.38830499211795,-32.6588840639347));
#16316=CARTESIAN_POINT('Ctrl Pts',(3.1947962814962,-2.29385390113191,-32.6530190836187));
#16317=CARTESIAN_POINT('Ctrl Pts',(3.26260281637298,-2.19941542561322,-32.6471548866654));
#16318=CARTESIAN_POINT('Ctrl Pts',(3.3262285965868,-2.10195367335074,-32.6412906897121));
#16319=CARTESIAN_POINT('Ctrl Pts',(3.38540556353765,-2.00187866025099,-32.6354264927588));
#16320=CARTESIAN_POINT('Ctrl Pts',(3.4445887783888,-1.90179308123793,-32.629561676664));
#16321=CARTESIAN_POINT('Ctrl Pts',(3.49932203689145,-1.79909404692213,-32.6236968605692));
#16322=CARTESIAN_POINT('Ctrl Pts',(3.54938243186301,-1.69421762249783,-32.6178320444744));
#16323=CARTESIAN_POINT('Ctrl Pts',(3.60064399297771,-1.58682475747607,-32.6118265059875));
#16324=CARTESIAN_POINT('Ctrl Pts',(3.64700538402346,-1.47714908601084,-32.6058209675006));
#16325=CARTESIAN_POINT('Ctrl Pts',(3.68827935888879,-1.36568091836817,-32.5998154290138));
#16326=CARTESIAN_POINT('Ctrl Pts',(3.72864513663629,-1.25666550864162,-32.5939420370614));
#16327=CARTESIAN_POINT('Ctrl Pts',(3.76414500498145,-1.14593608744854,-32.588068645109));
#16328=CARTESIAN_POINT('Ctrl Pts',(3.79465457177639,-1.03396599600593,-32.5821952531567));
#16329=CARTESIAN_POINT('Ctrl Pts',(3.82619379917154,-0.918217050791476,
-32.5761236414025));
#16330=CARTESIAN_POINT('Ctrl Pts',(3.85239983575519,-0.801142687395448,
-32.5700520296484));
#16331=CARTESIAN_POINT('Ctrl Pts',(3.87319299810052,-0.683275200387892,
-32.5639804178942));
#16332=CARTESIAN_POINT('Ctrl Pts',(3.89398616044585,-0.565407713380327,
-32.5579088061401));
#16333=CARTESIAN_POINT('Ctrl Pts',(3.90936645103122,-0.446747585810446,
-32.5518371943859));
#16334=CARTESIAN_POINT('Ctrl Pts',(3.91931331057507,-0.327829488528789,
-32.5457655826318));
#16335=CARTESIAN_POINT('Ctrl Pts',(3.92837945707135,-0.219440616014741,
-32.5402315624328));
#16336=CARTESIAN_POINT('Ctrl Pts',(3.932950010281,-0.11067065348999,-32.5346975422339));
#16337=CARTESIAN_POINT('Ctrl Pts',(3.93299959219997,-0.00179102061575733,
-32.529163522035));
#16338=CARTESIAN_POINT('',(3.93299993544946,-0.00071256899522975,-31.2791635220851));
#16339=CARTESIAN_POINT('Ctrl Pts',(3.93299959220032,-0.00179101985566553,
-32.5291635219964));
#16340=CARTESIAN_POINT('Ctrl Pts',(3.93305171423223,0.112666633760392,-32.5233459879883));
#16341=CARTESIAN_POINT('Ctrl Pts',(3.92810321604783,0.227316899582816,-32.5175284539803));
#16342=CARTESIAN_POINT('Ctrl Pts',(3.9181299609264,0.341682029511204,-32.5117109199722));
#16343=CARTESIAN_POINT('Ctrl Pts',(3.90816838821679,0.455913195099014,-32.5059002004723));
#16344=CARTESIAN_POINT('Ctrl Pts',(3.89319379647479,0.56985947233263,-32.5000894809724));
#16345=CARTESIAN_POINT('Ctrl Pts',(3.87323406790185,0.683042352452951,-32.4942787614725));
#16346=CARTESIAN_POINT('Ctrl Pts',(3.85261041818044,0.799990038666822,-32.4882747598069));
#16347=CARTESIAN_POINT('Ctrl Pts',(3.82666418253833,0.916122200091492,-32.4822707581414));
#16348=CARTESIAN_POINT('Ctrl Pts',(3.79548448130774,1.03091539524448,-32.4762667564758));
#16349=CARTESIAN_POINT('Ctrl Pts',(3.76535245975493,1.14185138545445,-32.4704644972992));
#16350=CARTESIAN_POINT('Ctrl Pts',(3.73033314601399,1.25153650408435,-32.4646622381226));
#16351=CARTESIAN_POINT('Ctrl Pts',(3.69055888857356,1.35950876789032,-32.458859978946));
#16352=CARTESIAN_POINT('Ctrl Pts',(3.65079462690175,1.46745389691527,-32.4530591779497));
#16353=CARTESIAN_POINT('Ctrl Pts',(3.60627794228205,1.57368663149507,-32.4472583769534));
#16354=CARTESIAN_POINT('Ctrl Pts',(3.5571905223991,1.67776177908368,-32.4414575759572));
#16355=CARTESIAN_POINT('Ctrl Pts',(3.50810303093362,1.78183707844156,-32.4356567665018));
#16356=CARTESIAN_POINT('Ctrl Pts',(3.45444497145797,1.88375440369289,-32.4298559570464));
#16357=CARTESIAN_POINT('Ctrl Pts',(3.3964451407445,1.98309087182436,-32.424055147591));
#16358=CARTESIAN_POINT('Ctrl Pts',(3.33843056402285,2.08245259548421,-32.4182528633247));
#16359=CARTESIAN_POINT('Ctrl Pts',(3.2760722352333,2.1792317944758,-32.4124505790584));
#16360=CARTESIAN_POINT('Ctrl Pts',(3.20964319846377,2.27303311426721,-32.4066482947921));
#16361=CARTESIAN_POINT('Ctrl Pts',(3.14314496263893,2.36693214679135,-32.4008399662926));
#16362=CARTESIAN_POINT('Ctrl Pts',(3.07256780052672,2.45784676568021,-32.395031637793));
#16363=CARTESIAN_POINT('Ctrl Pts',(2.99822606403165,2.54541341808384,-32.3892233092935));
#16364=CARTESIAN_POINT('Ctrl Pts',(2.9238378888289,2.63303477034203,-32.3834113525324));
#16365=CARTESIAN_POINT('Ctrl Pts',(2.84568074474241,2.71730368548287,-32.3775993957713));
#16366=CARTESIAN_POINT('Ctrl Pts',(2.76410571389922,2.79789360097729,-32.3717874390101));
#16367=CARTESIAN_POINT('Ctrl Pts',(2.68241606262938,2.87859675272063,-32.3659673159148));
#16368=CARTESIAN_POINT('Ctrl Pts',(2.59729925430606,2.95561030985458,-32.3601471928195));
#16369=CARTESIAN_POINT('Ctrl Pts',(2.50913919232883,3.02864813299918,-32.3543270697242));
#16370=CARTESIAN_POINT('Ctrl Pts',(2.48821374737605,3.04598420234176,-32.3529456203159));
#16371=CARTESIAN_POINT('Ctrl Pts',(2.46711697543488,3.06309647867762,-32.3515641709077));
#16372=CARTESIAN_POINT('Ctrl Pts',(2.44585423534079,3.07998150310444,-32.3501827214994));
#16373=CARTESIAN_POINT('Ctrl Pts',(2.35527673756693,3.15191029759021,-32.3442978623446));
#16374=CARTESIAN_POINT('Ctrl Pts',(2.26137970117448,3.21995436481127,-32.3384130031897));
#16375=CARTESIAN_POINT('Ctrl Pts',(2.16453006659768,3.28379332339821,-32.3325281440348));
#16376=CARTESIAN_POINT('Ctrl Pts',(2.06780174887448,3.34755231532728,-32.3266506564369));
#16377=CARTESIAN_POINT('Ctrl Pts',(1.96812852948163,3.40711645073853,-32.320773168839));
#16378=CARTESIAN_POINT('Ctrl Pts',(1.86591016926874,3.46220569005071,-32.314895681241));
#16379=CARTESIAN_POINT('Ctrl Pts',(1.76379286466078,3.51724046677523,-32.3090240042731));
#16380=CARTESIAN_POINT('Ctrl Pts',(1.65913578480731,3.56780895416281,-32.3031523273051));
#16381=CARTESIAN_POINT('Ctrl Pts',(1.55236686215112,3.61367487819465,-32.2972806503371));
#16382=CARTESIAN_POINT('Ctrl Pts',(1.44426405557712,3.66011381370697,-32.2913356174217));
#16383=CARTESIAN_POINT('Ctrl Pts',(1.33399663377892,3.70173164382356,-32.2853905845063));
#16384=CARTESIAN_POINT('Ctrl Pts',(1.22203397624083,3.73833144075175,-32.2794455515908));
#16385=CARTESIAN_POINT('Ctrl Pts',(1.11157231774895,3.7744405717607,-32.2735802192554));
#16386=CARTESIAN_POINT('Ctrl Pts',(0.999461004124491,3.80566527020334,-32.2677148869199));
#16387=CARTESIAN_POINT('Ctrl Pts',(0.886169354619096,3.83186545626722,-32.2618495545844));
#16388=CARTESIAN_POINT('Ctrl Pts',(0.772892840062088,3.85806214217494,-32.255985005815));
#16389=CARTESIAN_POINT('Ctrl Pts',(0.658436703789539,3.8792355580563,-32.2501204570457));
#16390=CARTESIAN_POINT('Ctrl Pts',(0.543282626586267,3.89529626442579,-32.2442559082764));
#16391=CARTESIAN_POINT('Ctrl Pts',(0.428116404063426,3.91135866472064,-32.2383907409721));
#16392=CARTESIAN_POINT('Ctrl Pts',(0.312252501559839,3.92230722672671,-32.2325255736678));
#16393=CARTESIAN_POINT('Ctrl Pts',(0.196179246584895,3.92810421236624,-32.2266604063636));
#16394=CARTESIAN_POINT('Ctrl Pts',(0.0773377641063493,3.93403945013877,
-32.2206553608639));
#16395=CARTESIAN_POINT('Ctrl Pts',(-0.0417227306380141,3.93457424637719,
-32.2146503153641));
#16396=CARTESIAN_POINT('Ctrl Pts',(-0.160477806242441,3.92972465622003,
-32.2086452698644));
#16397=CARTESIAN_POINT('Ctrl Pts',(-0.276636168396961,3.92498110781244,
-32.2027715314465));
#16398=CARTESIAN_POINT('Ctrl Pts',(-0.392501921659066,3.91508632444816,
-32.1968977930285));
#16399=CARTESIAN_POINT('Ctrl Pts',(-0.507590284058821,3.90010783229504,
-32.1910240546105));
#16400=CARTESIAN_POINT('Ctrl Pts',(-0.626537836959727,3.8846270751567,-32.1849533555699));
#16401=CARTESIAN_POINT('Ctrl Pts',(-0.744654470882471,3.86371577033904,
-32.1788826565293));
#16402=CARTESIAN_POINT('Ctrl Pts',(-0.861418538167016,3.83750532274578,
-32.1728119574888));
#16403=CARTESIAN_POINT('Ctrl Pts',(-0.978182605451561,3.81129487515252,
-32.1667412584482));
#16404=CARTESIAN_POINT('Ctrl Pts',(-1.09359366177943,3.77978547286386,-32.1606705594076));
#16405=CARTESIAN_POINT('Ctrl Pts',(-1.20715061798569,3.74316395386266,-32.1545998603671));
#16406=CARTESIAN_POINT('Ctrl Pts',(-1.31721038200262,3.70767026088368,-32.1487161195013));
#16407=CARTESIAN_POINT('Ctrl Pts',(-1.42587865616431,3.66726183895507,-32.1428323786355));
#16408=CARTESIAN_POINT('Ctrl Pts',(-1.53268548963072,3.62206628733869,-32.1369486377698));
#16409=CARTESIAN_POINT('Ctrl Pts',(-1.63935845199653,3.57692738357938,-32.1310722715526));
#16410=CARTESIAN_POINT('Ctrl Pts',(-1.74417423832575,3.52701344283815,-32.1251959053355));
#16411=CARTESIAN_POINT('Ctrl Pts',(-1.84667826186071,3.47250174905227,-32.1193195391183));
#16412=CARTESIAN_POINT('Ctrl Pts',(-1.9490808989236,3.41804397264572,-32.1134489852002));
#16413=CARTESIAN_POINT('Ctrl Pts',(-2.04917596062447,3.35899768197562,-32.1075784312821));
#16414=CARTESIAN_POINT('Ctrl Pts',(-2.14652965376657,3.29558787555434,-32.101707877364));
#16415=CARTESIAN_POINT('Ctrl Pts',(-2.24512543193172,3.23136905646669,-32.0957624241086));
#16416=CARTESIAN_POINT('Ctrl Pts',(-2.34090900591231,3.16267476497765,-32.0898169708532));
#16417=CARTESIAN_POINT('Ctrl Pts',(-2.43345601439873,3.08978653404837,-32.0838715175978));
#16418=CARTESIAN_POINT('Ctrl Pts',(-2.52473842753528,3.01789427391708,-32.0780073051374));
#16419=CARTESIAN_POINT('Ctrl Pts',(-2.61287184749229,2.9419222435584,-32.0721430926769));
#16420=CARTESIAN_POINT('Ctrl Pts',(-2.69747958601758,2.8621832371493,-32.0662788802165));
#16421=CARTESIAN_POINT('Ctrl Pts',(-2.78207606554118,2.78245484184532,-32.0604154481241));
#16422=CARTESIAN_POINT('Ctrl Pts',(-2.86314749740785,2.69896074954711,-32.0545520160318));
#16423=CARTESIAN_POINT('Ctrl Pts',(-2.9403524823033,2.61205212042426,-32.0486885839394));
#16424=CARTESIAN_POINT('Ctrl Pts',(-3.01756567032978,2.52513425714542,-32.0428245288497));
#16425=CARTESIAN_POINT('Ctrl Pts',(-3.09091132148113,2.43480144339318,-32.03696047376));
#16426=CARTESIAN_POINT('Ctrl Pts',(-3.16008737867501,2.34143903596462,-32.0310964186702));
#16427=CARTESIAN_POINT('Ctrl Pts',(-3.23094520039683,2.2458068607663,-32.0250898003839));
#16428=CARTESIAN_POINT('Ctrl Pts',(-3.29742779643953,2.14699624324494,-32.0190831820976));
#16429=CARTESIAN_POINT('Ctrl Pts',(-3.35925750524257,2.04545300935305,-32.0130765638113));
#16430=CARTESIAN_POINT('Ctrl Pts',(-3.41970817227618,1.94617458251997,-32.0072039163567));
#16431=CARTESIAN_POINT('Ctrl Pts',(-3.47571118555646,1.84428455241217,-32.0013312689021));
#16432=CARTESIAN_POINT('Ctrl Pts',(-3.52705408247575,1.74022369231405,-31.9954586214474));
#16433=CARTESIAN_POINT('Ctrl Pts',(-3.58015388307097,1.63260197144264,-31.9893850177453));
#16434=CARTESIAN_POINT('Ctrl Pts',(-3.6282687334104,1.52265863931259,-31.9833114140432));
#16435=CARTESIAN_POINT('Ctrl Pts',(-3.6712185706291,1.41090155810674,-31.9772378103411));
#16436=CARTESIAN_POINT('Ctrl Pts',(-3.7141684078478,1.29914447690088,-31.9711642066389));
#16437=CARTESIAN_POINT('Ctrl Pts',(-3.75195314199437,1.18557412248454,-31.9650906029368));
#16438=CARTESIAN_POINT('Ctrl Pts',(-3.78445039868035,1.07071199672375,-31.9590169992347));
#16439=CARTESIAN_POINT('Ctrl Pts',(-3.81594193452872,0.959404608965796,
-31.9531313606233));
#16440=CARTESIAN_POINT('Ctrl Pts',(-3.84256869735034,0.846530012854143,
-31.9472457220119));
#16441=CARTESIAN_POINT('Ctrl Pts',(-3.86417636695459,0.732550343027453,
-31.9413600834006));
#16442=CARTESIAN_POINT('Ctrl Pts',(-3.88575695202142,0.61871354314872,-31.935481822253));
#16443=CARTESIAN_POINT('Ctrl Pts',(-3.90233088084884,0.503774825099512,
-31.9296035611053));
#16444=CARTESIAN_POINT('Ctrl Pts',(-3.91379370506384,0.388211069139834,
-31.9237252999577));
#16445=CARTESIAN_POINT('Ctrl Pts',(-3.9252451851199,0.27276168059867,-31.9178528562184));
#16446=CARTESIAN_POINT('Ctrl Pts',(-3.93159558268809,0.156688891572664,
-31.9119804124791));
#16447=CARTESIAN_POINT('Ctrl Pts',(-3.9327916895247,0.0404787204031693,
-31.9061079687398));
#16448=CARTESIAN_POINT('Ctrl Pts',(-3.93400252235544,-0.0771621844156868,
-31.9001632257965));
#16449=CARTESIAN_POINT('Ctrl Pts',(-3.9299312103716,-0.194943457129721,
-31.8942184828533));
#16450=CARTESIAN_POINT('Ctrl Pts',(-3.92057681599806,-0.312356254713251,
-31.8882737399101));
#16451=CARTESIAN_POINT('Ctrl Pts',(-3.91134620590901,-0.42821535907428,
-31.8824076622147));
#16452=CARTESIAN_POINT('Ctrl Pts',(-3.89697153222601,-0.54371526059975,
-31.8765415845193));
#16453=CARTESIAN_POINT('Ctrl Pts',(-3.87750429054874,-0.658368799971655,
-31.8706755068239));
#16454=CARTESIAN_POINT('Ctrl Pts',(-3.85803968014414,-0.773006842298287,
-31.8648102220117));
#16455=CARTESIAN_POINT('Ctrl Pts',(-3.8334839395444,-0.886798344779898,
-31.8589449371996));
#16456=CARTESIAN_POINT('Ctrl Pts',(-3.80394005912343,-0.999264242628561,
-31.8530796523875));
#16457=CARTESIAN_POINT('Ctrl Pts',(-3.77439311406386,-1.11174180676233,
-31.847213759159));
#16458=CARTESIAN_POINT('Ctrl Pts',(-3.73985710503007,-1.2228930952866,-31.8413478659306));
#16459=CARTESIAN_POINT('Ctrl Pts',(-3.70048529600371,-1.33225281912268,
-31.8354819727021));
#16460=CARTESIAN_POINT('Ctrl Pts',(-3.66018660840177,-1.44418705471125,
-31.8294779864855));
#16461=CARTESIAN_POINT('Ctrl Pts',(-3.61482172994897,-1.55424388785106,
-31.8234740002688));
#16462=CARTESIAN_POINT('Ctrl Pts',(-3.56460727454468,-1.66194584095365,
-31.8174700140522));
#16463=CARTESIAN_POINT('Ctrl Pts',(-3.51547634177199,-1.76732381179428,
-31.8115955812658));
#16464=CARTESIAN_POINT('Ctrl Pts',(-3.46170324796393,-1.87044716029178,
-31.8057211484794));
#16465=CARTESIAN_POINT('Ctrl Pts',(-3.40353702545444,-1.97089439503002,
-31.799846715693));
#16466=CARTESIAN_POINT('Ctrl Pts',(-3.34344662560106,-2.07466449113008,
-31.7937779527612));
#16467=CARTESIAN_POINT('Ctrl Pts',(-3.27866766660018,-2.17557794348095,
-31.7877091898294));
#16468=CARTESIAN_POINT('Ctrl Pts',(-3.20952190686546,-2.273204374743,-31.7816404268976));
#16469=CARTESIAN_POINT('Ctrl Pts',(-3.14037614713074,-2.37083080600505,
-31.7755716639658));
#16470=CARTESIAN_POINT('Ctrl Pts',(-3.06686393037735,-2.46516987925628,
-31.7695029010341));
#16471=CARTESIAN_POINT('Ctrl Pts',(-2.98935019207031,-2.55583145554812,
-31.7634341381023));
#16472=CARTESIAN_POINT('Ctrl Pts',(-2.91417255045495,-2.64376068770246,
-31.7575482745806));
#16473=CARTESIAN_POINT('Ctrl Pts',(-2.83499306814641,-2.72850939594701,
-31.7516624110588));
#16474=CARTESIAN_POINT('Ctrl Pts',(-2.75211092009533,-2.80969295181734,
-31.7457765475371));
#16475=CARTESIAN_POINT('Ctrl Pts',(-2.66933239946434,-2.89077500401473,
-31.7398980431014));
#16476=CARTESIAN_POINT('Ctrl Pts',(-2.58286071195722,-2.96830048431027,
-31.7340195386656));
#16477=CARTESIAN_POINT('Ctrl Pts',(-2.49303494529769,-3.04191810565711,
-31.7281410342298));
#16478=CARTESIAN_POINT('Ctrl Pts',(-2.40329779861645,-3.11546309759874,
-31.7222683293876));
#16479=CARTESIAN_POINT('Ctrl Pts',(-2.3102134718646,-3.18510764119335,-31.7163956245454));
#16480=CARTESIAN_POINT('Ctrl Pts',(-2.21415705663655,-3.25053803677892,
-31.7105229197031));
#16481=CARTESIAN_POINT('Ctrl Pts',(-2.11692384721111,-3.31677002494606,
-31.7045782679226));
#16482=CARTESIAN_POINT('Ctrl Pts',(-2.01664554141955,-3.37868361472674,
-31.698633616142));
#16483=CARTESIAN_POINT('Ctrl Pts',(-1.91374511930567,-3.43599601547116,
-31.6926889643615));
#16484=CARTESIAN_POINT('Ctrl Pts',(-1.81219955576724,-3.4925538012584,-31.6868225840037));
#16485=CARTESIAN_POINT('Ctrl Pts',(-1.70810088469865,-3.54463063851432,
-31.6809562036459));
#16486=CARTESIAN_POINT('Ctrl Pts',(-1.60188317654743,-3.59199934419458,
-31.6750898232882));
#16487=CARTESIAN_POINT('Ctrl Pts',(-1.49567955441164,-3.63936176809443,
-31.6692242208979));
#16488=CARTESIAN_POINT('Ctrl Pts',(-1.38735782941932,-3.68201713481731,
-31.6633586185076));
#16489=CARTESIAN_POINT('Ctrl Pts',(-1.27737387499542,-3.71978560988119,
-31.6574930161173));
#16490=CARTESIAN_POINT('Ctrl Pts',(-1.16737824096497,-3.75755809572038,
-31.6516267908368));
#16491=CARTESIAN_POINT('Ctrl Pts',(-1.0557204153621,-3.79044252472724,-31.6457605655564));
#16492=CARTESIAN_POINT('Ctrl Pts',(-0.942872669685536,-3.81830854289698,
-31.6398943402759));
#16493=CARTESIAN_POINT('Ctrl Pts',(-0.827382485098032,-3.84682707078469,
-31.633890751667));
#16494=CARTESIAN_POINT('Ctrl Pts',(-0.710646397335317,-3.87008912208951,
-31.6278871630582));
#16495=CARTESIAN_POINT('Ctrl Pts',(-0.593181743754018,-3.88801034192001,
-31.6218835744494));
#16496=CARTESIAN_POINT('Ctrl Pts',(-0.478236988361779,-3.90554710865743,
-31.616008777197));
#16497=CARTESIAN_POINT('Ctrl Pts',(-0.362595031718715,-3.91796990281258,
-31.6101339799445));
#16498=CARTESIAN_POINT('Ctrl Pts',(-0.246744773518751,-3.92525235070832,
-31.6042591826921));
#16499=CARTESIAN_POINT('Ctrl Pts',(-0.127084891449762,-3.93277427487074,
-31.5981911984051));
#16500=CARTESIAN_POINT('Ctrl Pts',(-0.00720325506352192,-3.93481194975495,
-31.5921232141181));
#16501=CARTESIAN_POINT('Ctrl Pts',(0.112363832481439,-3.9313945832427,-31.586055229831));
#16502=CARTESIAN_POINT('Ctrl Pts',(0.231930920026399,-3.92797721673046,
-31.579987245544));
#16503=CARTESIAN_POINT('Ctrl Pts',(0.351182988310738,-3.91910490808594,
-31.573919261257));
#16504=CARTESIAN_POINT('Ctrl Pts',(0.469593286093134,-3.90486506113287,
-31.56785127697));
#16505=CARTESIAN_POINT('Ctrl Pts',(0.584294806373449,-3.89107122626661,
-31.5619733505076));
#16506=CARTESIAN_POINT('Ctrl Pts',(0.698572919306183,-3.87219701765988,
-31.5560954240451));
#16507=CARTESIAN_POINT('Ctrl Pts',(0.811942726654698,-3.84827727803397,
-31.5502174975827));
#16508=CARTESIAN_POINT('Ctrl Pts',(0.925170039140109,-3.82438760320312,
-31.5443469591043));
#16509=CARTESIAN_POINT('Ctrl Pts',(1.03749091658504,-3.79546509425855,-31.5384764206259));
#16510=CARTESIAN_POINT('Ctrl Pts',(1.14842598251843,-3.76159630511789,-31.5326058821475));
#16511=CARTESIAN_POINT('Ctrl Pts',(1.25925109854133,-3.72776108399564,-31.5267411620745));
#16512=CARTESIAN_POINT('Ctrl Pts',(1.36869274309091,-3.68898945429681,-31.5208764420014));
#16513=CARTESIAN_POINT('Ctrl Pts',(1.47628278024491,-3.64541878976234,-31.5150117219284));
#16514=CARTESIAN_POINT('Ctrl Pts',(1.58539396695761,-3.60123210632054,-31.5090640841746));
#16515=CARTESIAN_POINT('Ctrl Pts',(1.69260036333872,-3.55210972764478,-31.5031164464208));
#16516=CARTESIAN_POINT('Ctrl Pts',(1.79743036528644,-3.49824714420612,-31.497168808667));
#16517=CARTESIAN_POINT('Ctrl Pts',(1.90068752249324,-3.4451927023254,-31.4913104078739));
#16518=CARTESIAN_POINT('Ctrl Pts',(2.00163872939307,-3.38753952073739,-31.4854520070808));
#16519=CARTESIAN_POINT('Ctrl Pts',(2.0998550913667,-3.32552215377696,-31.4795936062877));
#16520=CARTESIAN_POINT('Ctrl Pts',(2.19805868078675,-3.26351285186929,-31.4737359673507));
#16521=CARTESIAN_POINT('Ctrl Pts',(2.29352778400063,-3.19714071333686,-31.4678783284138));
#16522=CARTESIAN_POINT('Ctrl Pts',(2.38586080640622,-3.12668469987855,-31.4620206894768));
#16523=CARTESIAN_POINT('Ctrl Pts',(2.47820404212279,-3.05622089300943,-31.4561624026039));
#16524=CARTESIAN_POINT('Ctrl Pts',(2.5674101796388,-2.98167256333388,-31.4503041157309));
#16525=CARTESIAN_POINT('Ctrl Pts',(2.65310970997126,-2.90335975498321,-31.4444458288579));
#16526=CARTESIAN_POINT('Ctrl Pts',(2.74109860687635,-2.82295490803035,-31.4384310444396));
#16527=CARTESIAN_POINT('Ctrl Pts',(2.82539055430386,-2.73858191763267,-31.4324162600212));
#16528=CARTESIAN_POINT('Ctrl Pts',(2.90562603120515,-2.65062754207056,-31.4264014756028));
#16529=CARTESIAN_POINT('Ctrl Pts',(2.98389002092637,-2.56483431679443,-31.4205344820474));
#16530=CARTESIAN_POINT('Ctrl Pts',(3.05829435436076,-2.47563402424389,-31.414667488492));
#16531=CARTESIAN_POINT('Ctrl Pts',(3.12854700286134,-2.38341827023444,-31.4088004949366));
#16532=CARTESIAN_POINT('Ctrl Pts',(3.20145417095092,-2.28771811342087,-31.4027118150868));
#16533=CARTESIAN_POINT('Ctrl Pts',(3.2698894444237,-2.18877053340756,-31.3966231352369));
#16534=CARTESIAN_POINT('Ctrl Pts',(3.33357715425003,-2.08704392782285,-31.3905344553871));
#16535=CARTESIAN_POINT('Ctrl Pts',(3.39726486407637,-1.98531732223815,-31.3844457755372));
#16536=CARTESIAN_POINT('Ctrl Pts',(3.45620482858731,-1.88081215020138,-31.3783570956874));
#16537=CARTESIAN_POINT('Ctrl Pts',(3.51017619113269,-1.77402145060458,-31.3722684158376));
#16538=CARTESIAN_POINT('Ctrl Pts',(3.56572192470471,-1.66411561410128,-31.3660021262203));
#16539=CARTESIAN_POINT('Ctrl Pts',(3.61616462233887,-1.55147512007693,-31.3597358366031));
#16540=CARTESIAN_POINT('Ctrl Pts',(3.66124566739239,-1.43658245951997,-31.3534695469859));
#16541=CARTESIAN_POINT('Ctrl Pts',(3.70619995623913,-1.32201284732672,-31.3472208765499));
#16542=CARTESIAN_POINT('Ctrl Pts',(3.74582253378528,-1.20520400118841,-31.3409722061139));
#16543=CARTESIAN_POINT('Ctrl Pts',(3.77990204431146,-1.08665980665986,-31.3347235356779));
#16544=CARTESIAN_POINT('Ctrl Pts',(3.81392381785851,-0.968316447870441,
-31.3284854516427));
#16545=CARTESIAN_POINT('Ctrl Pts',(3.84242114239712,-0.848243912120649,
-31.3222473676074));
#16546=CARTESIAN_POINT('Ctrl Pts',(3.86523110494377,-0.726964583301815,
-31.3160092835721));
#16547=CARTESIAN_POINT('Ctrl Pts',(3.88798371869111,-0.605990174926128,
-31.3097868833254));
#16548=CARTESIAN_POINT('Ctrl Pts',(3.90507742094504,-0.483815345367452,
-31.3035644830787));
#16549=CARTESIAN_POINT('Ctrl Pts',(3.9163996318116,-0.360974963045875,-31.2973420828319));
#16550=CARTESIAN_POINT('Ctrl Pts',(3.9274254680305,-0.241350098917437,-31.291282562583));
#16551=CARTESIAN_POINT('Ctrl Pts',(3.93297812503326,-0.121094407183991,
-31.285223042334));
#16552=CARTESIAN_POINT('Ctrl Pts',(3.93299993544946,-0.000712568995229939,
-31.2791635220851));
#16553=CARTESIAN_POINT('',(0.654108433901418,3.87822525863301,-31.));
#16554=CARTESIAN_POINT('Ctrl Pts',(3.93299993544964,-0.000712567999896496,
-31.279163522035));
#16555=CARTESIAN_POINT('Ctrl Pts',(3.93302182838837,0.120124919265748,-31.2730810663097));
#16556=CARTESIAN_POINT('Ctrl Pts',(3.92747046918608,0.240887678128942,-31.2669986105844));
#16557=CARTESIAN_POINT('Ctrl Pts',(3.91639254011805,0.3610518961419,-31.260916154859));
#16558=CARTESIAN_POINT('Ctrl Pts',(3.90530392792135,0.481331995904546,-31.2548278334474));
#16559=CARTESIAN_POINT('Ctrl Pts',(3.88867815372494,0.601012040784996,-31.2487395120357));
#16560=CARTESIAN_POINT('Ctrl Pts',(3.86661343148888,0.719575966406443,-31.2426511906241));
#16561=CARTESIAN_POINT('Ctrl Pts',(3.84450626013787,0.838367990693939,-31.2365511562231));
#16562=CARTESIAN_POINT('Ctrl Pts',(3.81693929734249,0.956039245012285,-31.2304511218222));
#16563=CARTESIAN_POINT('Ctrl Pts',(3.78406158109265,1.07208532799334,-31.2243510874212));
#16564=CARTESIAN_POINT('Ctrl Pts',(3.75115008462019,1.18825064256846,-31.2182447855375));
#16565=CARTESIAN_POINT('Ctrl Pts',(3.71291706603387,1.30278710910749,-31.2121384836538));
#16566=CARTESIAN_POINT('Ctrl Pts',(3.66956041237949,1.41520859942883,-31.2060321817701));
#16567=CARTESIAN_POINT('Ctrl Pts',(3.62611689304407,1.52785532782776,-31.1999136458224));
#16568=CARTESIAN_POINT('Ctrl Pts',(3.57752936691509,1.63837827559699,-31.1937951098748));
#16569=CARTESIAN_POINT('Ctrl Pts',(3.52404300556402,1.74631322933068,-31.1876765739272));
#16570=CARTESIAN_POINT('Ctrl Pts',(3.49201630120468,1.81094280528141,-31.1840129008532));
#16571=CARTESIAN_POINT('Ctrl Pts',(3.45823403773063,1.87464498004681,-31.1803492277792));
#16572=CARTESIAN_POINT('Ctrl Pts',(3.42275629611291,1.93732504691894,-31.1766855547052));
#16573=CARTESIAN_POINT('Ctrl Pts',(3.36644302306109,2.03681615203801,-31.1708702628411));
#16574=CARTESIAN_POINT('Ctrl Pts',(3.3056891682797,2.13402452447637,-31.165054970977));
#16575=CARTESIAN_POINT('Ctrl Pts',(3.24070643811116,2.22852210713397,-31.1592396791128));
#16576=CARTESIAN_POINT('Ctrl Pts',(3.1758044980169,2.32290220524297,-31.1534316171367));
#16577=CARTESIAN_POINT('Ctrl Pts',(3.1066843713842,2.41457786870808,-31.1476235551606));
#16578=CARTESIAN_POINT('Ctrl Pts',(3.03360355966315,2.50314570946221,-31.1418154931845));
#16579=CARTESIAN_POINT('Ctrl Pts',(2.95925294581569,2.59325244435111,-31.1359065143018));
#16580=CARTESIAN_POINT('Ctrl Pts',(2.88080291760339,2.68014194914679,-31.1299975354191));
#16581=CARTESIAN_POINT('Ctrl Pts',(2.79857094634214,2.76341992073041,-31.1240885565364));
#16582=CARTESIAN_POINT('Ctrl Pts',(2.71787516654151,2.84514216031779,-31.1182899644383));
#16583=CARTESIAN_POINT('Ctrl Pts',(2.6335378263978,2.92338631305955,-31.1124913723403));
#16584=CARTESIAN_POINT('Ctrl Pts',(2.54589896308285,2.99781378170387,-31.1066927802422));
#16585=CARTESIAN_POINT('Ctrl Pts',(2.45828820621802,3.07221738089284,-31.1008960477967));
#16586=CARTESIAN_POINT('Ctrl Pts',(2.36737835217052,3.1428064560757,-31.0950993153513));
#16587=CARTESIAN_POINT('Ctrl Pts',(2.27354439861573,3.20928105150095,-31.0893025829058));
#16588=CARTESIAN_POINT('Ctrl Pts',(2.1797167497417,3.27575118051414,-31.0835062399414));
#16589=CARTESIAN_POINT('Ctrl Pts',(2.08296573690538,3.33810713625727,-31.077709896977));
#16590=CARTESIAN_POINT('Ctrl Pts',(1.98369668323778,3.39609135167349,-31.0719135540125));
#16591=CARTESIAN_POINT('Ctrl Pts',(1.88106314204737,3.45604080360682,-31.0659207578448));
#16592=CARTESIAN_POINT('Ctrl Pts',(1.77573824618556,3.51131664947634,-31.0599279616771));
#16593=CARTESIAN_POINT('Ctrl Pts',(1.66819802120471,3.56168560685088,-31.0539351655094));
#16594=CARTESIAN_POINT('Ctrl Pts',(1.56406648301076,3.61045802674836,-31.0481323221256));
#16595=CARTESIAN_POINT('Ctrl Pts',(1.45785835084361,3.65462980752974,-31.0423294787417));
#16596=CARTESIAN_POINT('Ctrl Pts',(1.35002535461948,3.69403851386048,-31.0365266353579));
#16597=CARTESIAN_POINT('Ctrl Pts',(1.23689758052407,3.73538225263511,-31.0304388627982));
#16598=CARTESIAN_POINT('Ctrl Pts',(1.12198182485564,3.7714831080146,-31.0243510902386));
#16599=CARTESIAN_POINT('Ctrl Pts',(1.0058150810249,3.80221317429505,-31.0182633176789));
#16600=CARTESIAN_POINT('Ctrl Pts',(0.88964833719417,3.83294324057551,-31.0121755451193));
#16601=CARTESIAN_POINT('Ctrl Pts',(0.772231136853311,3.85830247151174,-31.0060877725596));
#16602=CARTESIAN_POINT('Ctrl Pts',(0.654108433901418,3.87822525863301,-31.));
#16603=CARTESIAN_POINT('',(3.48540987471235,1.82219839898339,-31.));
#16604=CARTESIAN_POINT('Origin',(0.,0.,-31.));
#16605=CARTESIAN_POINT('',(3.92893057216212,-0.00338598511717015,-31.095833725221));
#16606=CARTESIAN_POINT('Ctrl Pts',(3.48540987471235,1.82219839898339,-31.));
#16607=CARTESIAN_POINT('Ctrl Pts',(3.77799362579873,1.26255884722778,-31.0319436609371));
#16608=CARTESIAN_POINT('Ctrl Pts',(3.92425990185113,0.629251789626864,-31.0638873218741));
#16609=CARTESIAN_POINT('Ctrl Pts',(3.92487792373439,-0.00332812842372134,
-31.0958309828112));
#16610=CARTESIAN_POINT('',(3.93299929380719,-0.00235688610855974,-32.3458364779251));
#16611=CARTESIAN_POINT('Ctrl Pts',(3.93299849204801,-0.00344405983004216,
-31.095836477965));
#16612=CARTESIAN_POINT('Ctrl Pts',(3.93288845114196,-0.129107009634538,
-31.1021690432223));
#16613=CARTESIAN_POINT('Ctrl Pts',(3.92675170311396,-0.25460888520464,-31.1085016084795));
#16614=CARTESIAN_POINT('Ctrl Pts',(3.91465899908993,-0.379386242296975,
-31.1148341737368));
#16615=CARTESIAN_POINT('Ctrl Pts',(3.90253790530163,-0.504456536332721,
-31.1211816058125));
#16616=CARTESIAN_POINT('Ctrl Pts',(3.88443295009405,-0.628798615777614,
-31.1275290378882));
#16617=CARTESIAN_POINT('Ctrl Pts',(3.86046608878056,-0.751858083267953,
-31.1338764699639));
#16618=CARTESIAN_POINT('Ctrl Pts',(3.8364193407474,-0.875327734513778,-31.1402450594002));
#16619=CARTESIAN_POINT('Ctrl Pts',(3.80647165118053,-0.997505924425334,
-31.1466136488364));
#16620=CARTESIAN_POINT('Ctrl Pts',(3.77079568576157,-1.11785012244127,-31.1529822382727));
#16621=CARTESIAN_POINT('Ctrl Pts',(3.73505755223346,-1.23840402946294,-31.1593619254651));
#16622=CARTESIAN_POINT('Ctrl Pts',(3.69357130388557,-1.35711727869021,-31.1657416126575));
#16623=CARTESIAN_POINT('Ctrl Pts',(3.64655818641543,-1.47346611535067,-31.1721212998499));
#16624=CARTESIAN_POINT('Ctrl Pts',(3.59943219296957,-1.59009429933308,-31.1785163043293));
#16625=CARTESIAN_POINT('Ctrl Pts',(3.54675291703733,-1.70434644496144,-31.1849113088088));
#16626=CARTESIAN_POINT('Ctrl Pts',(3.48878881390637,-1.81572068665909,-31.1913063132883));
#16627=CARTESIAN_POINT('Ctrl Pts',(3.47586798582981,-1.84054721465491,-31.1927318292363));
#16628=CARTESIAN_POINT('Ctrl Pts',(3.46268473224403,-1.86523085121481,-31.1941573451844));
#16629=CARTESIAN_POINT('Ctrl Pts',(3.44924232171538,-1.8897662305395,-31.1955828611324));
#16630=CARTESIAN_POINT('Ctrl Pts',(3.39423695124737,-1.99016322603759,-31.201415969165));
#16631=CARTESIAN_POINT('Ctrl Pts',(3.33474002976474,-2.08834716632629,-31.2072490771975));
#16632=CARTESIAN_POINT('Ctrl Pts',(3.27095393633534,-2.1838840047888,-31.21308218523));
#16633=CARTESIAN_POINT('Ctrl Pts',(3.20725631784468,-2.27928832822371,-31.2189072024099));
#16634=CARTESIAN_POINT('Ctrl Pts',(3.13928158462642,-2.372052503483,-31.2247322195899));
#16635=CARTESIAN_POINT('Ctrl Pts',(3.06727850060632,-2.46176595144994,-31.2305572367698));
#16636=CARTESIAN_POINT('Ctrl Pts',(2.99535532717324,-2.55137983348317,-31.2363757892192));
#16637=CARTESIAN_POINT('Ctrl Pts',(2.91941295315617,-2.6379493951853,-31.2421943416685));
#16638=CARTESIAN_POINT('Ctrl Pts',(2.83974361914423,-2.72109264405489,-31.2480128941179));
#16639=CARTESIAN_POINT('Ctrl Pts',(2.75807317376219,-2.80632426108675,-31.2539775952906));
#16640=CARTESIAN_POINT('Ctrl Pts',(2.67248628543714,-2.88795476940036,-31.2599422964634));
#16641=CARTESIAN_POINT('Ctrl Pts',(2.58334229389153,-2.96560813200114,-31.2659069976362));
#16642=CARTESIAN_POINT('Ctrl Pts',(2.49649679742058,-3.04125927472848,-31.271717904526));
#16643=CARTESIAN_POINT('Ctrl Pts',(2.4062757346846,-3.11313557650278,-31.2775288114157));
#16644=CARTESIAN_POINT('Ctrl Pts',(2.3130483080209,-3.18092699142273,-31.2833397183054));
#16645=CARTESIAN_POINT('Ctrl Pts',(2.21983983305758,-3.24870462539184,-31.2891494439273));
#16646=CARTESIAN_POINT('Ctrl Pts',(2.12362654842139,-3.31239877639275,-31.2949591695491));
#16647=CARTESIAN_POINT('Ctrl Pts',(2.02480914457453,-3.37174093430195,-31.300768895171));
#16648=CARTESIAN_POINT('Ctrl Pts',(1.92598704856082,-3.43108590996687,-31.3065788966572));
#16649=CARTESIAN_POINT('Ctrl Pts',(1.82456094781493,-3.48607826618171,-31.3123888981434));
#16650=CARTESIAN_POINT('Ctrl Pts',(1.72095810138853,-3.53649433949288,-31.3181988996296));
#16651=CARTESIAN_POINT('Ctrl Pts',(1.61253055425839,-3.58925824853226,-31.3242794681825));
#16652=CARTESIAN_POINT('Ctrl Pts',(1.50171907493652,-3.63700911638447,-31.3303600367355));
#16653=CARTESIAN_POINT('Ctrl Pts',(1.38903784788383,-3.67954655591504,-31.3364406052884));
#16654=CARTESIAN_POINT('Ctrl Pts',(1.2812187115245,-3.720248544286,-31.3422588029341));
#16655=CARTESIAN_POINT('Ctrl Pts',(1.1716882509613,-3.75617757405178,-31.3480770005797));
#16656=CARTESIAN_POINT('Ctrl Pts',(1.06091210127569,-3.78720933054496,-31.3538951982254));
#16657=CARTESIAN_POINT('Ctrl Pts',(0.950061720735049,-3.81826188135013,
-31.3597172946326));
#16658=CARTESIAN_POINT('Ctrl Pts',(0.83796439726712,-3.84441053232061,-31.3655393910397));
#16659=CARTESIAN_POINT('Ctrl Pts',(0.725095303676809,-3.86558220719542,
-31.3713614874469));
#16660=CARTESIAN_POINT('Ctrl Pts',(0.612067657769103,-3.88678362287888,
-31.377191762416));
#16661=CARTESIAN_POINT('Ctrl Pts',(0.498266492570521,-3.90299405740786,
-31.3830220373852));
#16662=CARTESIAN_POINT('Ctrl Pts',(0.384171317235336,-3.91419230480743,
-31.3888523123543));
#16663=CARTESIAN_POINT('Ctrl Pts',(0.36908061049378,-3.91567343200697,-31.3896234489911));
#16664=CARTESIAN_POINT('Ctrl Pts',(0.353984758379108,-3.91706695155966,
-31.3903945856279));
#16665=CARTESIAN_POINT('Ctrl Pts',(0.338884867325807,-3.91837288254928,
-31.3911657222647));
#16666=CARTESIAN_POINT('Ctrl Pts',(0.223539665693932,-3.92834864149907,
-31.397056288663));
#16667=CARTESIAN_POINT('Ctrl Pts',(0.107572026652748,-3.93324268448918,
-31.4029468550613));
#16668=CARTESIAN_POINT('Ctrl Pts',(-0.00853435788344206,-3.93299074048433,
-31.4088374214595));
#16669=CARTESIAN_POINT('Ctrl Pts',(-0.124495126349702,-3.93273911245777,
-31.4147206001407));
#16670=CARTESIAN_POINT('Ctrl Pts',(-0.240593887336033,-3.92735433517721,
-31.4206037788218));
#16671=CARTESIAN_POINT('Ctrl Pts',(-0.356341900523714,-3.91682389825368,
-31.4264869575029));
#16672=CARTESIAN_POINT('Ctrl Pts',(-0.47197512477886,-3.90630390451254,
-31.432364301753));
#16673=CARTESIAN_POINT('Ctrl Pts',(-0.587257886849221,-3.89064844015712,
-31.4382416460031));
#16674=CARTESIAN_POINT('Ctrl Pts',(-0.701702152312787,-3.86989703860963,
-31.4441189902532));
#16675=CARTESIAN_POINT('Ctrl Pts',(-0.817422920671509,-3.84891417745998,
-31.4500618899676));
#16676=CARTESIAN_POINT('Ctrl Pts',(-0.932285946629697,-3.82272100001071,
-31.4560047896819));
#16677=CARTESIAN_POINT('Ctrl Pts',(-1.04579232132231,-3.79141232532987,
-31.4619476893962));
#16678=CARTESIAN_POINT('Ctrl Pts',(-1.15792355827808,-3.7604829574515,-31.4678185904613));
#16679=CARTESIAN_POINT('Ctrl Pts',(-1.26873043180122,-3.72456148096188,
-31.4736894915263));
#16680=CARTESIAN_POINT('Ctrl Pts',(-1.37774352204889,-3.68379041035892,
-31.4795603925913));
#16681=CARTESIAN_POINT('Ctrl Pts',(-1.48674117497777,-3.64302511333794,
-31.4854304622794));
#16682=CARTESIAN_POINT('Ctrl Pts',(-1.59394516568978,-3.59741173182533,
-31.4913005319675));
#16683=CARTESIAN_POINT('Ctrl Pts',(-1.69890371294145,-3.54714183169404,
-31.4971706016556));
#16684=CARTESIAN_POINT('Ctrl Pts',(-1.80387234132728,-3.49686710320316,
-31.5030412351564));
#16685=CARTESIAN_POINT('Ctrl Pts',(-1.90659472750348,-3.4419351442463,-31.5089118686571));
#16686=CARTESIAN_POINT('Ctrl Pts',(-2.0066420688035,-3.38258430903178,-31.5147825021579));
#16687=CARTESIAN_POINT('Ctrl Pts',(-2.10884590380171,-3.32195418242921,
-31.5207796755945));
#16688=CARTESIAN_POINT('Ctrl Pts',(-2.208257657063,-3.25671271250808,-31.5267768490311));
#16689=CARTESIAN_POINT('Ctrl Pts',(-2.30445085540019,-3.18716100237269,
-31.5327740224677));
#16690=CARTESIAN_POINT('Ctrl Pts',(-2.3987488390712,-3.11897961179613,-31.5386530385788));
#16691=CARTESIAN_POINT('Ctrl Pts',(-2.48995363833394,-3.04665656586699,
-31.5445320546898));
#16692=CARTESIAN_POINT('Ctrl Pts',(-2.5776973771932,-2.97051598743573,-31.5504110708008));
#16693=CARTESIAN_POINT('Ctrl Pts',(-2.66808634579564,-2.89207998228404,
-31.5564673229002));
#16694=CARTESIAN_POINT('Ctrl Pts',(-2.75480192024057,-2.80959294879769,
-31.5625235749996));
#16695=CARTESIAN_POINT('Ctrl Pts',(-2.837484066154,-2.72344876476906,-31.568579827099));
#16696=CARTESIAN_POINT('Ctrl Pts',(-2.92016621206744,-2.63730458074044,
-31.5746360791984));
#16697=CARTESIAN_POINT('Ctrl Pts',(-2.99881466652138,-2.54750364007306,
-31.5806923312978));
#16698=CARTESIAN_POINT('Ctrl Pts',(-3.07311643582633,-2.45447435754666,
-31.5867485833971));
#16699=CARTESIAN_POINT('Ctrl Pts',(-3.14542210974768,-2.36394427959004,
-31.5926421360484));
#16700=CARTESIAN_POINT('Ctrl Pts',(-3.21383489080398,-2.2700777034157,-31.5985356886997));
#16701=CARTESIAN_POINT('Ctrl Pts',(-3.27803367643307,-2.17324278813268,
-31.604429241351));
#16702=CARTESIAN_POINT('Ctrl Pts',(-3.34215395399215,-2.07652629132492,
-31.6103155868342));
#16703=CARTESIAN_POINT('Ctrl Pts',(-3.40207026179529,-1.97684901452301,
-31.6162019323173));
#16704=CARTESIAN_POINT('Ctrl Pts',(-3.45750187819924,-1.87461189643316,
-31.6220882778004));
#16705=CARTESIAN_POINT('Ctrl Pts',(-3.51288020561038,-1.77247306364337,
-31.6279689644657));
#16706=CARTESIAN_POINT('Ctrl Pts',(-3.56378222474554,-1.66777964389323,
-31.6338496511309));
#16707=CARTESIAN_POINT('Ctrl Pts',(-3.60997100205417,-1.56096071838083,
-31.6397303377962));
#16708=CARTESIAN_POINT('Ctrl Pts',(-3.65663909781835,-1.45303329237582,
-31.6456720505767));
#16709=CARTESIAN_POINT('Ctrl Pts',(-3.6984953340556,-1.34293634713679,-31.6516137633573));
#16710=CARTESIAN_POINT('Ctrl Pts',(-3.73534330456992,-1.23113744033909,
-31.6575554761379));
#16711=CARTESIAN_POINT('Ctrl Pts',(-3.77177541596714,-1.12060027452805,
-31.6634301318893));
#16712=CARTESIAN_POINT('Ctrl Pts',(-3.80331160853401,-1.0083997689392,-31.6693047876408));
#16713=CARTESIAN_POINT('Ctrl Pts',(-3.8298110422003,-0.895006358100695,
-31.6751794433922));
#16714=CARTESIAN_POINT('Ctrl Pts',(-3.85630739569812,-0.781626127574343,
-31.6810534163016));
#16715=CARTESIAN_POINT('Ctrl Pts',(-3.87776806151683,-0.667053666515133,
-31.6869273892109));
#16716=CARTESIAN_POINT('Ctrl Pts',(-3.89410283350252,-0.551771802566638,
-31.6928013621203));
#16717=CARTESIAN_POINT('Ctrl Pts',(-3.91043957582767,-0.436476033042626,
-31.6986760435623));
#16718=CARTESIAN_POINT('Ctrl Pts',(-3.9216491374739,-0.320471096193623,
-31.7045507250044));
#16719=CARTESIAN_POINT('Ctrl Pts',(-3.92769300733848,-0.204246517973773,
-31.7104254064465));
#16720=CARTESIAN_POINT('Ctrl Pts',(-3.93385774921905,-0.0856975516728088,
-31.7164175762867));
#16721=CARTESIAN_POINT('Ctrl Pts',(-3.93464793608923,0.0330794915937387,
-31.722409746127));
#16722=CARTESIAN_POINT('Ctrl Pts',(-3.9300785144255,0.151564740131223,-31.7284019159672));
#16723=CARTESIAN_POINT('Ctrl Pts',(-3.92559204599207,0.267899008778536,
-31.7342853040225));
#16724=CARTESIAN_POINT('Ctrl Pts',(-3.91593901857735,0.383951580272443,
-31.7401686920779));
#16725=CARTESIAN_POINT('Ctrl Pts',(-3.90118599137473,0.49923627742943,-31.7460520801332));
#16726=CARTESIAN_POINT('Ctrl Pts',(-3.88602379671181,0.61771833510769,-31.7520986408659));
#16727=CARTESIAN_POINT('Ctrl Pts',(-3.86547465590248,0.735388840375355,
-31.7581452015986));
#16728=CARTESIAN_POINT('Ctrl Pts',(-3.83966659809232,0.851733183276386,
-31.7641917623313));
#16729=CARTESIAN_POINT('Ctrl Pts',(-3.81385854028217,0.968077526177417,
-31.7702383230641));
#16730=CARTESIAN_POINT('Ctrl Pts',(-3.78279174634404,1.08309527567172,-31.7762848837968));
#16731=CARTESIAN_POINT('Ctrl Pts',(-3.74664851272451,1.19629173787134,-31.7823314445295));
#16732=CARTESIAN_POINT('Ctrl Pts',(-3.71151110362466,1.30633807303971,-31.7882097364485));
#16733=CARTESIAN_POINT('Ctrl Pts',(-3.67146411556804,1.41501373852729,-31.7940880283675));
#16734=CARTESIAN_POINT('Ctrl Pts',(-3.6266326806316,1.5218490068909,-31.7999663202865));
#16735=CARTESIAN_POINT('Ctrl Pts',(-3.58185810939464,1.62854876657401,-31.8058371562447));
#16736=CARTESIAN_POINT('Ctrl Pts',(-3.53231131853186,1.73341239476686,-31.8117079922028));
#16737=CARTESIAN_POINT('Ctrl Pts',(-3.47816719981031,1.83598527503999,-31.8175788281609));
#16738=CARTESIAN_POINT('Ctrl Pts',(-3.42407736618943,1.93845531535078,-31.8234437779965));
#16739=CARTESIAN_POINT('Ctrl Pts',(-3.36539956498137,2.03863881380937,-31.829308727832));
#16740=CARTESIAN_POINT('Ctrl Pts',(-3.30235650108527,2.13610171568206,-31.8351736776675));
#16741=CARTESIAN_POINT('Ctrl Pts',(-3.23842581409762,2.23493685927217,-31.841121203834));
#16742=CARTESIAN_POINT('Ctrl Pts',(-3.17000616205701,2.33097380993132,-31.8470687300004));
#16743=CARTESIAN_POINT('Ctrl Pts',(-3.09737794932883,2.423786054711,-31.8530162561668));
#16744=CARTESIAN_POINT('Ctrl Pts',(-3.02583733452349,2.51520844834546,-31.858874718912));
#16745=CARTESIAN_POINT('Ctrl Pts',(-2.95021360718964,2.60350172132222,-31.8647331816572));
#16746=CARTESIAN_POINT('Ctrl Pts',(-2.87081757249818,2.68828857555056,-31.8705916444024));
#16747=CARTESIAN_POINT('Ctrl Pts',(-2.79143271514784,2.77306349352042,-31.8764492823956));
#16748=CARTESIAN_POINT('Ctrl Pts',(-2.70827688832753,2.8543326735494,-31.8823069203888));
#16749=CARTESIAN_POINT('Ctrl Pts',(-2.62169940402785,2.93175395197483,-31.888164558382));
#16750=CARTESIAN_POINT('Ctrl Pts',(-2.53511327273959,3.00918296290618,-31.894022781411));
#16751=CARTESIAN_POINT('Ctrl Pts',(-2.44510511203493,3.08276303347397,-31.89988100444));
#16752=CARTESIAN_POINT('Ctrl Pts',(-2.35205857871393,3.15219121283881,-31.905739227469));
#16753=CARTESIAN_POINT('Ctrl Pts',(-2.25652846112328,3.22347255887184,-31.9117538173184));
#16754=CARTESIAN_POINT('Ctrl Pts',(-2.15779584488271,3.29037695920454,-31.9177684071678));
#16755=CARTESIAN_POINT('Ctrl Pts',(-2.05630804007415,3.3526237850863,-31.9237829970172));
#16756=CARTESIAN_POINT('Ctrl Pts',(-1.95731441833698,3.41334082145636,-31.9296497711935));
#16757=CARTESIAN_POINT('Ctrl Pts',(-1.85569985651786,3.46962641060938,-31.9355165453697));
#16758=CARTESIAN_POINT('Ctrl Pts',(-1.75190378738148,3.52126711848994,-31.941383319546));
#16759=CARTESIAN_POINT('Ctrl Pts',(-1.64418494432331,3.57485948816136,-31.947471817232));
#16760=CARTESIAN_POINT('Ctrl Pts',(-1.53411690652952,3.62344876785874,-31.9535603149179));
#16761=CARTESIAN_POINT('Ctrl Pts',(-1.422211510523,3.66685197674189,-31.9596488126039));
#16762=CARTESIAN_POINT('Ctrl Pts',(-1.31030611451649,3.71025518562503,-31.9657373102899));
#16763=CARTESIAN_POINT('Ctrl Pts',(-1.19656384528513,3.74847223088484,-31.9718258079759));
#16764=CARTESIAN_POINT('Ctrl Pts',(-1.08151049659051,3.78137859064185,-31.9779143056618));
#16765=CARTESIAN_POINT('Ctrl Pts',(-0.970285561707589,3.81318998737853,
-31.9838002078658));
#16766=CARTESIAN_POINT('Ctrl Pts',(-0.857479633024243,3.84014032372034,
-31.9896861100698));
#16767=CARTESIAN_POINT('Ctrl Pts',(-0.743554482563883,3.86207401941744,
-31.9955720122738));
#16768=CARTESIAN_POINT('Ctrl Pts',(-0.62977194254846,3.88398025871803,-32.0014505465601));
#16769=CARTESIAN_POINT('Ctrl Pts',(-0.514873367582792,3.90088227040903,
-32.0073290808463));
#16770=CARTESIAN_POINT('Ctrl Pts',(-0.399335407964658,3.91267430690898,
-32.0132076151326));
#16771=CARTESIAN_POINT('Ctrl Pts',(-0.283911607503072,3.92445469209585,
-32.0190803410377));
#16772=CARTESIAN_POINT('Ctrl Pts',(-0.167850085885753,3.93113510480027,
-32.0249530669427));
#16773=CARTESIAN_POINT('Ctrl Pts',(-0.0516367685391186,3.93266101312265,
-32.0308257928478));
#16774=CARTESIAN_POINT('Ctrl Pts',(0.0659996431599903,3.9342056070102,-32.0367704334289));
#16775=CARTESIAN_POINT('Ctrl Pts',(0.183791173653705,3.93046852614243,-32.04271507401));
#16776=CARTESIAN_POINT('Ctrl Pts',(0.301229032194601,3.92144744579895,-32.0486597145911));
#16777=CARTESIAN_POINT('Ctrl Pts',(0.417120827942007,3.91254512747012,-32.0545260943138));
#16778=CARTESIAN_POINT('Ctrl Pts',(0.532667787277854,3.89849714383648,-32.0603924740364));
#16779=CARTESIAN_POINT('Ctrl Pts',(0.647382560249071,3.87935366017142,-32.0662588537591));
#16780=CARTESIAN_POINT('Ctrl Pts',(0.762081961465147,3.86021274172908,-32.0721244473881));
#16781=CARTESIAN_POINT('Ctrl Pts',(0.875948992750114,3.83597774888851,-32.0779900410171));
#16782=CARTESIAN_POINT('Ctrl Pts',(0.988504258375365,3.8067503636532,-32.0838556346462));
#16783=CARTESIAN_POINT('Ctrl Pts',(1.10107132092402,3.77751991509409,-32.0897218430484));
#16784=CARTESIAN_POINT('Ctrl Pts',(1.21232594663721,3.74329613725687,-32.0955880514506));
#16785=CARTESIAN_POINT('Ctrl Pts',(1.32180237773559,3.70423102333164,-32.1014542598528));
#16786=CARTESIAN_POINT('Ctrl Pts',(1.43384238434553,3.66425113379296,-32.1074578354312));
#16787=CARTESIAN_POINT('Ctrl Pts',(1.54401945122707,3.61920049195865,-32.1134614110097));
#16788=CARTESIAN_POINT('Ctrl Pts',(1.65185562922367,3.56929432524163,-32.1194649865881));
#16789=CARTESIAN_POINT('Ctrl Pts',(1.75737803034139,3.52045896552841,-32.1253397470081));
#16790=CARTESIAN_POINT('Ctrl Pts',(1.860658644922,3.46697459450396,-32.131214507428));
#16791=CARTESIAN_POINT('Ctrl Pts',(1.96127524441245,3.40908908884102,-32.1370892678479));
#16792=CARTESIAN_POINT('Ctrl Pts',(2.06520115584614,3.34929971049503,-32.1431572510056));
#16793=CARTESIAN_POINT('Ctrl Pts',(2.16628438487693,3.28481495921471,-32.1492252341633));
#16794=CARTESIAN_POINT('Ctrl Pts',(2.26409384522701,3.21595523289818,-32.1552932173211));
#16795=CARTESIAN_POINT('Ctrl Pts',(2.3619033055771,3.14709550658164,-32.1613612004788));
#16796=CARTESIAN_POINT('Ctrl Pts',(2.45643865972793,3.07386114764121,-32.1674291836365));
#16797=CARTESIAN_POINT('Ctrl Pts',(2.54730890847625,2.99661581201154,-32.1734971667942));
#16798=CARTESIAN_POINT('Ctrl Pts',(2.63427423100519,2.92268990535426,-32.1793043932482));
#16799=CARTESIAN_POINT('Ctrl Pts',(2.7181748340813,2.84484219312201,-32.1851116197022));
#16800=CARTESIAN_POINT('Ctrl Pts',(2.79863052019651,2.76335958778886,-32.1909188461562));
#16801=CARTESIAN_POINT('Ctrl Pts',(2.87898489175215,2.6819795901727,-32.1967187598071));
#16802=CARTESIAN_POINT('Ctrl Pts',(2.95590267489068,2.59697409683223,-32.202518673458));
#16803=CARTESIAN_POINT('Ctrl Pts',(3.02903642612008,2.50867043057427,-32.2083185871088));
#16804=CARTESIAN_POINT('Ctrl Pts',(3.10209185833723,2.42046132880675,-32.214112289626));
#16805=CARTESIAN_POINT('Ctrl Pts',(3.17137105156308,2.32896140468738,-32.2199059921432));
#16806=CARTESIAN_POINT('Ctrl Pts',(3.23656382083118,2.23453432143852,-32.2256996946603));
#16807=CARTESIAN_POINT('Ctrl Pts',(3.30171799691789,2.14016313766427,-32.231489967389));
#16808=CARTESIAN_POINT('Ctrl Pts',(3.36279031607265,2.04286858521363,-32.2372802401176));
#16809=CARTESIAN_POINT('Ctrl Pts',(3.41951159785563,1.94304643077071,-32.2430705128463));
#16810=CARTESIAN_POINT('Ctrl Pts',(3.47621377014188,1.84325790658216,-32.2488588348221));
#16811=CARTESIAN_POINT('Ctrl Pts',(3.52856760988196,1.74094384073624,-32.254647156798));
#16812=CARTESIAN_POINT('Ctrl Pts',(3.57634837369138,1.63652721028251,-32.2604354787739));
#16813=CARTESIAN_POINT('Ctrl Pts',(3.62412522745937,1.53211912455092,-32.2662233270742));
#16814=CARTESIAN_POINT('Ctrl Pts',(3.66732957434697,1.42560920173296,-32.2720111753745));
#16815=CARTESIAN_POINT('Ctrl Pts',(3.70578394079474,1.31744236463982,-32.2777990236749));
#16816=CARTESIAN_POINT('Ctrl Pts',(3.74426510439598,1.20920015084436,-32.2835909052716));
#16817=CARTESIAN_POINT('Ctrl Pts',(3.77798953120207,1.09929911511907,-32.2893827868684));
#16818=CARTESIAN_POINT('Ctrl Pts',(3.80682902228904,0.98820129278295,-32.2951746684652));
#16819=CARTESIAN_POINT('Ctrl Pts',(3.83567813033554,0.877066423216763,-32.3009684814515));
#16820=CARTESIAN_POINT('Ctrl Pts',(3.85963896757854,0.764734386023264,-32.3067622944377));
#16821=CARTESIAN_POINT('Ctrl Pts',(3.87863444631211,0.651677705527191,-32.312556107424));
#16822=CARTESIAN_POINT('Ctrl Pts',(3.8976559144384,0.538466342197817,-32.3183578474378));
#16823=CARTESIAN_POINT('Ctrl Pts',(3.91169839772483,0.424528775291612,-32.3241595874515));
#16824=CARTESIAN_POINT('Ctrl Pts',(3.92073667789608,0.310343201311663,-32.3299613274652));
#16825=CARTESIAN_POINT('Ctrl Pts',(3.92898041496336,0.206195528200064,-32.3352530442852));
#16826=CARTESIAN_POINT('Ctrl Pts',(3.9330617358394,0.101841813893803,-32.3405447611052));
#16827=CARTESIAN_POINT('Ctrl Pts',(3.93299929380719,-0.00235688610856188,
-32.3458364779251));
#16828=CARTESIAN_POINT('',(3.93299863980535,0.00327097680709692,-33.5958364779274));
#16829=CARTESIAN_POINT('Ctrl Pts',(3.93299929380672,-0.00235688689347031,
-32.345836477965));
#16830=CARTESIAN_POINT('Ctrl Pts',(3.93290786947772,-0.154919074919968,
-32.3535843279522));
#16831=CARTESIAN_POINT('Ctrl Pts',(3.92393949909681,-0.307206649636701,
-32.3613321779394));
#16832=CARTESIAN_POINT('Ctrl Pts',(3.9061895909518,-0.458445067090745,-32.3690800279266));
#16833=CARTESIAN_POINT('Ctrl Pts',(3.89271012912065,-0.573297068510666,
-32.3749638244692));
#16834=CARTESIAN_POINT('Ctrl Pts',(3.87413948421733,-0.687737169573374,
-32.3808476210119));
#16835=CARTESIAN_POINT('Ctrl Pts',(3.85051165487551,-0.801279598934025,
-32.3867314175545));
#16836=CARTESIAN_POINT('Ctrl Pts',(3.82691348143223,-0.914679518260579,
-32.3926078291923));
#16837=CARTESIAN_POINT('Ctrl Pts',(3.79827083100888,-1.02718360738723,-32.39848424083));
#16838=CARTESIAN_POINT('Ctrl Pts',(3.7646694235675,-1.1383115264531,-32.4043606524677));
#16839=CARTESIAN_POINT('Ctrl Pts',(3.73110130936551,-1.24932933678556,-32.410231241588));
#16840=CARTESIAN_POINT('Ctrl Pts',(3.69258433062127,-1.35897329793973,-32.4161018307083));
#16841=CARTESIAN_POINT('Ctrl Pts',(3.64925504953696,-1.46677421010494,-32.4219724198286));
#16842=CARTESIAN_POINT('Ctrl Pts',(3.60537334162382,-1.575949530397,-32.4279178560465));
#16843=CARTESIAN_POINT('Ctrl Pts',(3.55655585067352,-1.68323405766395,-32.4338632922645));
#16844=CARTESIAN_POINT('Ctrl Pts',(3.50299642499465,-1.78815688530808,-32.4398087284824));
#16845=CARTESIAN_POINT('Ctrl Pts',(3.45016861389524,-1.89164648118303,-32.4456729508381));
#16846=CARTESIAN_POINT('Ctrl Pts',(3.39272780919716,-1.99283812295064,-32.4515371731938));
#16847=CARTESIAN_POINT('Ctrl Pts',(3.33090777942233,-2.09130159589281,-32.4574013955495));
#16848=CARTESIAN_POINT('Ctrl Pts',(3.26909607629266,-2.18975180662201,-32.4632648280431));
#16849=CARTESIAN_POINT('Ctrl Pts',(3.2029065398853,-2.2854742310021,-32.4691282605367));
#16850=CARTESIAN_POINT('Ctrl Pts',(3.1326174228084,-2.37806582800335,-32.4749916930303));
#16851=CARTESIAN_POINT('Ctrl Pts',(3.0623209512491,-2.47066711303738,-32.4808557390258));
#16852=CARTESIAN_POINT('Ctrl Pts',(2.9879242950677,-2.5601365918027,-32.4867197850214));
#16853=CARTESIAN_POINT('Ctrl Pts',(2.90974688741391,-2.64610318226351,-32.492583831017));
#16854=CARTESIAN_POINT('Ctrl Pts',(2.82966915740579,-2.73415943313237,-32.4985904191871));
#16855=CARTESIAN_POINT('Ctrl Pts',(2.74562479919922,-2.81853996037597,-32.5045970073573));
#16856=CARTESIAN_POINT('Ctrl Pts',(2.65799729820821,-2.89888588301055,-32.5106035955274));
#16857=CARTESIAN_POINT('Ctrl Pts',(2.57232427483763,-2.97743973916022,-32.5164762104355));
#16858=CARTESIAN_POINT('Ctrl Pts',(2.48322663197954,-3.0521368632481,-32.5223488253436));
#16859=CARTESIAN_POINT('Ctrl Pts',(2.39109555004112,-3.12268331256526,-32.5282214402517));
#16860=CARTESIAN_POINT('Ctrl Pts',(2.29581175799552,-3.1956438494966,-32.5342950150529));
#16861=CARTESIAN_POINT('Ctrl Pts',(2.19728360198152,-3.26416427734106,-32.5403685898541));
#16862=CARTESIAN_POINT('Ctrl Pts',(2.09597436760318,-3.32796941848186,-32.5464421646553));
#16863=CARTESIAN_POINT('Ctrl Pts',(1.99466513322484,-3.39177455962266,-32.5525157394565));
#16864=CARTESIAN_POINT('Ctrl Pts',(1.89057526983297,-3.45086423343124,-32.5585893142577));
#16865=CARTESIAN_POINT('Ctrl Pts',(1.78419264010639,-3.50501720723168,-32.5646628890589));
#16866=CARTESIAN_POINT('Ctrl Pts',(1.68111551557648,-3.55748754791079,-32.5705477466501));
#16867=CARTESIAN_POINT('Ctrl Pts',(1.57555808635996,-3.60549039330302,-32.5764326042414));
#16868=CARTESIAN_POINT('Ctrl Pts',(1.46794369784586,-3.64878477029745,-32.5823174618327));
#16869=CARTESIAN_POINT('Ctrl Pts',(1.36046410956057,-3.69202491577131,-32.5881949479176));
#16870=CARTESIAN_POINT('Ctrl Pts',(1.25093306492191,-3.73056817116982,-32.5940724340025));
#16871=CARTESIAN_POINT('Ctrl Pts',(1.13979804754758,-3.76421962839667,-32.5999499200874));
#16872=CARTESIAN_POINT('Ctrl Pts',(1.02877290005148,-3.79783781724784,-32.6058215955943));
#16873=CARTESIAN_POINT('Ctrl Pts',(0.916147325773982,-3.82657371003728,
-32.6116932711013));
#16874=CARTESIAN_POINT('Ctrl Pts',(0.802387709503257,-3.85028089412164,
-32.6175649466082));
#16875=CARTESIAN_POINT('Ctrl Pts',(0.687206833635811,-3.87428426470869,
-32.6235099800909));
#16876=CARTESIAN_POINT('Ctrl Pts',(0.570863781666884,-3.89313225162008,
-32.6294550135735));
#16877=CARTESIAN_POINT('Ctrl Pts',(0.453857729347805,-3.9067252477633,-32.6354000470561));
#16878=CARTESIAN_POINT('Ctrl Pts',(0.338420326141269,-3.92013600853567,
-32.6412653780677));
#16879=CARTESIAN_POINT('Ctrl Pts',(0.222338012342579,-3.92843178006083,
-32.6471307090793));
#16880=CARTESIAN_POINT('Ctrl Pts',(0.106098594155559,-3.93156865491603,
-32.6529960400909));
#16881=CARTESIAN_POINT('Ctrl Pts',(-0.010125296343861,-3.93470511073598,
-32.65886058759));
#16882=CARTESIAN_POINT('Ctrl Pts',(-0.126505838513776,-3.932684029393,-32.6647251350892));
#16883=CARTESIAN_POINT('Ctrl Pts',(-0.242553186744214,-3.9255135908057,
-32.6705896825884));
#16884=CARTESIAN_POINT('Ctrl Pts',(-0.358612775602586,-3.91834239588339,
-32.6764548486777));
#16885=CARTESIAN_POINT('Ctrl Pts',(-0.47433869020946,-3.90602078932509,
-32.682320014767));
#16886=CARTESIAN_POINT('Ctrl Pts',(-0.589244857220856,-3.88860894128463,
-32.6881851808563));
#16887=CARTESIAN_POINT('Ctrl Pts',(-0.70689148036391,-3.8707818291468,-32.6941902283009));
#16888=CARTESIAN_POINT('Ctrl Pts',(-0.823678309532684,-3.84761865795514,
-32.7001952757455));
#16889=CARTESIAN_POINT('Ctrl Pts',(-0.939094590741654,-3.81923949885835,
-32.7062003231901));
#16890=CARTESIAN_POINT('Ctrl Pts',(-1.05198710792769,-3.79148089606418,
-32.712074060541));
#16891=CARTESIAN_POINT('Ctrl Pts',(-1.16356801858427,-3.75873225249553,
-32.7179477978919));
#16892=CARTESIAN_POINT('Ctrl Pts',(-1.27337566660935,-3.72115619286361,
-32.7238215352428));
#16893=CARTESIAN_POINT('Ctrl Pts',(-1.38686551517042,-3.68232008814917,
-32.7298922377342));
#16894=CARTESIAN_POINT('Ctrl Pts',(-1.49846063602563,-3.63832730397798,
-32.7359629402257));
#16895=CARTESIAN_POINT('Ctrl Pts',(-1.60767595214863,-3.58941040184638,
-32.7420336427171));
#16896=CARTESIAN_POINT('Ctrl Pts',(-1.71689126827162,-3.54049349971479,
-32.7481043452085));
#16897=CARTESIAN_POINT('Ctrl Pts',(-1.82372638164384,-3.48665275234288,
-32.7541750476999));
#16898=CARTESIAN_POINT('Ctrl Pts',(-1.92772739141904,-3.42817095611825,
-32.7602457501914));
#16899=CARTESIAN_POINT('Ctrl Pts',(-2.02854192543948,-3.37148097735932,
-32.766130453082));
#16900=CARTESIAN_POINT('Ctrl Pts',(-2.12701386129577,-3.31025008180474,
-32.7720151559726));
#16901=CARTESIAN_POINT('Ctrl Pts',(-2.22270794992252,-3.24469696109686,
-32.7778998588632));
#16902=CARTESIAN_POINT('Ctrl Pts',(-2.31828216821603,-3.1792259549118,-32.783777190334));
#16903=CARTESIAN_POINT('Ctrl Pts',(-2.41108512357713,-3.10944372242548,
-32.7896545218048));
#16904=CARTESIAN_POINT('Ctrl Pts',(-2.50070651882283,-3.03561458467919,
-32.7955318532757));
#16905=CARTESIAN_POINT('Ctrl Pts',(-2.59023931497713,-2.96185843390778,
-32.8014033744573));
#16906=CARTESIAN_POINT('Ctrl Pts',(-2.67659649230363,-2.88406359674231,
-32.8072748956388));
#16907=CARTESIAN_POINT('Ctrl Pts',(-2.75939763216431,-2.80253701270937,
-32.8131464168204));
#16908=CARTESIAN_POINT('Ctrl Pts',(-2.84323627165616,-2.71998889925055,
-32.8190915082581));
#16909=CARTESIAN_POINT('Ctrl Pts',(-2.92342879285128,-2.63361511917308,
-32.8250365996957));
#16910=CARTESIAN_POINT('Ctrl Pts',(-2.9996155108833,-2.54377589163596,-32.8309816911333));
#16911=CARTESIAN_POINT('Ctrl Pts',(-3.07477813895752,-2.45514426895587,
-32.8368468695809));
#16912=CARTESIAN_POINT('Ctrl Pts',(-3.14604172766473,-2.36314012029348,
-32.8427120480285));
#16913=CARTESIAN_POINT('Ctrl Pts',(-3.21309928916625,-2.26814504782197,
-32.8485772264761));
#16914=CARTESIAN_POINT('Ctrl Pts',(-3.2801479034551,-2.1731626501495,-32.8544416223573));
#16915=CARTESIAN_POINT('Ctrl Pts',(-3.34299136954786,-2.07519045824185,
-32.8603060182384));
#16916=CARTESIAN_POINT('Ctrl Pts',(-3.40136491724334,-1.97464065078844,
-32.8661704141195));
#16917=CARTESIAN_POINT('Ctrl Pts',(-3.45974463353904,-1.87408021777623,
-32.8720354297182));
#16918=CARTESIAN_POINT('Ctrl Pts',(-3.51365328594307,-1.77094198339011,
-32.8779004453169));
#16919=CARTESIAN_POINT('Ctrl Pts',(-3.56287146345836,-1.66566381208037,
-32.8837654609156));
#16920=CARTESIAN_POINT('Ctrl Pts',(-3.6132665685438,-1.55786818099041,-32.8897707234496));
#16921=CARTESIAN_POINT('Ctrl Pts',(-3.65874382689069,-1.44782937750596,
-32.8957759859836));
#16922=CARTESIAN_POINT('Ctrl Pts',(-3.6991199637996,-1.33603910624624,-32.9017812485177));
#16923=CARTESIAN_POINT('Ctrl Pts',(-3.73861081307489,-1.22669994973603,
-32.9076548395975));
#16924=CARTESIAN_POINT('Ctrl Pts',(-3.77322186797733,-1.1156857559224,-32.9135284306774));
#16925=CARTESIAN_POINT('Ctrl Pts',(-3.80283252423422,-1.00347087283408,
-32.9194020217573));
#16926=CARTESIAN_POINT('Ctrl Pts',(-3.83343887753063,-0.88748261755462,
-32.9254731200184));
#16927=CARTESIAN_POINT('Ctrl Pts',(-3.85870252048206,-0.77021197615689,
-32.9315442182795));
#16928=CARTESIAN_POINT('Ctrl Pts',(-3.87854805071123,-0.652191703660906,
-32.9376153165405));
#16929=CARTESIAN_POINT('Ctrl Pts',(-3.8983935809404,-0.534171431164921,
-32.9436864148016));
#16930=CARTESIAN_POINT('Ctrl Pts',(-3.91282100477258,-0.415402010263376,
-32.9497575130626));
#16931=CARTESIAN_POINT('Ctrl Pts',(-3.92181403309018,-0.296418099745836,
-32.9558286113237));
#16932=CARTESIAN_POINT('Ctrl Pts',(-3.93053068511083,-0.181090836513672,
-32.9617131308711));
#16933=CARTESIAN_POINT('Ctrl Pts',(-3.93416982632619,-0.0651953659832383,
-32.9675976504184));
#16934=CARTESIAN_POINT('Ctrl Pts',(-3.93267210647658,0.0507848692139364,
-32.9734821699658));
#16935=CARTESIAN_POINT('Ctrl Pts',(-3.93117626367143,0.166619750085193,
-32.9793593146326));
#16936=CARTESIAN_POINT('Ctrl Pts',(-3.92455636942314,0.282538776546033,
-32.9852364592995));
#16937=CARTESIAN_POINT('Ctrl Pts',(-3.91280488118397,0.398053968430045,
-32.9911136039664));
#16938=CARTESIAN_POINT('Ctrl Pts',(-3.90106501715643,0.513454896230318,
-32.9969849351421));
#16939=CARTESIAN_POINT('Ctrl Pts',(-3.88420369839419,0.628452377167216,
-33.0028562663178));
#16940=CARTESIAN_POINT('Ctrl Pts',(-3.86226541634821,0.74255966338108,-33.0087275974935));
#16941=CARTESIAN_POINT('Ctrl Pts',(-3.84005126678914,0.858101815515895,
-33.0146727589502));
#16942=CARTESIAN_POINT('Ctrl Pts',(-3.81263159476208,0.972730802578463,
-33.020617920407));
#16943=CARTESIAN_POINT('Ctrl Pts',(-3.78010674175324,1.08594752219051,-33.0265630818638));
#16944=CARTESIAN_POINT('Ctrl Pts',(-3.74802053654203,1.19763733975325,-33.0324280636506));
#16945=CARTESIAN_POINT('Ctrl Pts',(-3.71096613123705,1.30795234443374,-33.0382930454374));
#16946=CARTESIAN_POINT('Ctrl Pts',(-3.66909086963857,1.41642549762947,-33.0441580272242));
#16947=CARTESIAN_POINT('Ctrl Pts',(-3.6272212107881,1.52488413753693,-33.0500222242992));
#16948=CARTESIAN_POINT('Ctrl Pts',(-3.58053212654854,1.63150103247949,-33.0558864213741));
#16949=CARTESIAN_POINT('Ctrl Pts',(-3.5292198152104,1.73582732318807,-33.0617506184491));
#16950=CARTESIAN_POINT('Ctrl Pts',(-3.47790209812912,1.84016460465336,-33.0676154333162));
#16951=CARTESIAN_POINT('Ctrl Pts',(-3.4219603672357,1.9422104331075,-33.0734802481833));
#16952=CARTESIAN_POINT('Ctrl Pts',(-3.36163734700523,2.04153945521992,-33.0793450630504));
#16953=CARTESIAN_POINT('Ctrl Pts',(-3.29986694772536,2.14325175895605,-33.0853505971675));
#16954=CARTESIAN_POINT('Ctrl Pts',(-3.23350255939668,2.24211482894883,-33.0913561312846));
#16955=CARTESIAN_POINT('Ctrl Pts',(-3.1628518234218,2.33770343351704,-33.0973616654018));
#16956=CARTESIAN_POINT('Ctrl Pts',(-3.09375569744753,2.43118869126863,-33.1032350527936));
#16957=CARTESIAN_POINT('Ctrl Pts',(-3.02056021980915,2.52154181398208,-33.1091084401855));
#16958=CARTESIAN_POINT('Ctrl Pts',(-2.94359326470448,2.60839945023504,-33.1149818275774));
#16959=CARTESIAN_POINT('Ctrl Pts',(-2.8640287631433,2.698188432089,-33.1210534350571));
#16960=CARTESIAN_POINT('Ctrl Pts',(-2.78043405929133,2.78424147427113,-33.1271250425369));
#16961=CARTESIAN_POINT('Ctrl Pts',(-2.69321084009126,2.86620033682486,-33.1331966500167));
#16962=CARTESIAN_POINT('Ctrl Pts',(-2.60598762089118,2.94815919937859,-33.1392682574965));
#16963=CARTESIAN_POINT('Ctrl Pts',(-2.51513629182969,3.02602361977077,-33.1453398649762));
#16964=CARTESIAN_POINT('Ctrl Pts',(-2.42109291475038,3.09948352119277,-33.151411472456));
#16965=CARTESIAN_POINT('Ctrl Pts',(-2.32994515332462,3.17068157657018,-33.1572961338455));
#16966=CARTESIAN_POINT('Ctrl Pts',(-2.23550924406806,3.23796877116968,-33.163180795235));
#16967=CARTESIAN_POINT('Ctrl Pts',(-2.13815464494391,3.30102767548301,-33.1690654566246));
#16968=CARTESIAN_POINT('Ctrl Pts',(-2.04092202264943,3.36400757248391,-33.1749427450461));
#16969=CARTESIAN_POINT('Ctrl Pts',(-1.9407783259589,3.42276949413999,-33.1808200334676));
#16970=CARTESIAN_POINT('Ctrl Pts',(-1.83812551117062,3.47703661257453,-33.1866973218892));
#16971=CARTESIAN_POINT('Ctrl Pts',(-1.73557420493279,3.53125006880272,-33.1925687985361));
#16972=CARTESIAN_POINT('Ctrl Pts',(-1.63051907802622,3.58097737262402,-33.198440275183));
#16973=CARTESIAN_POINT('Ctrl Pts',(-1.52338990881487,3.62598568470989,-33.2043117518299));
#16974=CARTESIAN_POINT('Ctrl Pts',(-1.4149172922143,3.67155842103063,-33.2102568594031));
#16975=CARTESIAN_POINT('Ctrl Pts',(-1.30431861513318,3.71229276106702,-33.2162019669764));
#16976=CARTESIAN_POINT('Ctrl Pts',(-1.19206485361884,3.74799551557452,-33.2221470745497));
#16977=CARTESIAN_POINT('Ctrl Pts',(-1.0813211949525,3.78321797587596,-33.2280122050803));
#16978=CARTESIAN_POINT('Ctrl Pts',(-0.968967114970975,3.81354327603183,
-33.2338773356108));
#16979=CARTESIAN_POINT('Ctrl Pts',(-0.855473010787105,3.83883510036767,
-33.2397424661414));
#16980=CARTESIAN_POINT('Ctrl Pts',(-0.741994072734053,3.86412354497626,
-33.245606812919));
#16981=CARTESIAN_POINT('Ctrl Pts',(-0.627375814775837,3.88437976206234,
-33.2514711596967));
#16982=CARTESIAN_POINT('Ctrl Pts',(-0.512100590272377,3.89951817349819,
-33.2573355064743));
#16983=CARTESIAN_POINT('Ctrl Pts',(-0.396813206327458,3.91465818176136,
-33.263200471834));
#16984=CARTESIAN_POINT('Ctrl Pts',(-0.280869125837155,3.92467925766785,
-33.2690654371936));
#16985=CARTESIAN_POINT('Ctrl Pts',(-0.164756934862439,3.92954757604673,
-33.2749304025533));
#16986=CARTESIAN_POINT('Ctrl Pts',(-0.045865909800695,3.93453240457794,
-33.2809357301396));
#16987=CARTESIAN_POINT('Ctrl Pts',(0.0732009217401429,3.93411467667804,
-33.2869410577258));
#16988=CARTESIAN_POINT('Ctrl Pts',(0.19191917622264,3.92831465514131,-33.2929463853121));
#16989=CARTESIAN_POINT('Ctrl Pts',(0.308032114969537,3.9226419172093,-33.2988199237769));
#16990=CARTESIAN_POINT('Ctrl Pts',(0.423811209757561,3.91182078482897,-33.3046934622417));
#16991=CARTESIAN_POINT('Ctrl Pts',(0.538772264323822,3.8959226695605,-33.3105670007065));
#16992=CARTESIAN_POINT('Ctrl Pts',(0.657602523920222,3.87948947684516,-33.3166382228535));
#16993=CARTESIAN_POINT('Ctrl Pts',(0.775558231229076,3.85763162002537,-33.3227094450005));
#16994=CARTESIAN_POINT('Ctrl Pts',(0.892118655377857,3.83048473495546,-33.3287806671475));
#16995=CARTESIAN_POINT('Ctrl Pts',(1.00867907952663,3.80333784988555,-33.3348518892945));
#16996=CARTESIAN_POINT('Ctrl Pts',(1.12384377742956,3.77090212835676,-33.3409231114414));
#16997=CARTESIAN_POINT('Ctrl Pts',(1.2371130332575,3.7333684981454,-33.3469943335884));
#16998=CARTESIAN_POINT('Ctrl Pts',(1.3469010622397,3.69698842968524,-33.3528789622828));
#16999=CARTESIAN_POINT('Ctrl Pts',(1.45525749307561,3.6557036013568,-33.3587635909771));
#17000=CARTESIAN_POINT('Ctrl Pts',(1.56171331480212,3.60964548430587,-33.3646482196714));
#17001=CARTESIAN_POINT('Ctrl Pts',(1.66803575248797,3.56364507586739,-33.3705254752081));
#17002=CARTESIAN_POINT('Ctrl Pts',(1.77246194313386,3.51288343575072,-33.3764027307448));
#17003=CARTESIAN_POINT('Ctrl Pts',(1.8745386466048,3.45754159228563,-33.3822799862815));
#17004=CARTESIAN_POINT('Ctrl Pts',(1.97651440811705,3.40225447545147,-33.3881514298978));
#17005=CARTESIAN_POINT('Ctrl Pts',(2.07614494481964,3.34239636046427,-33.394022873514));
#17006=CARTESIAN_POINT('Ctrl Pts',(2.17299819887174,3.27819581899864,-33.3998943171302));
#17007=CARTESIAN_POINT('Ctrl Pts',(2.27106679079648,3.21318967373321,-33.4058394370298));
#17008=CARTESIAN_POINT('Ctrl Pts',(2.36628752689966,3.14373154093288,-33.4117845569294));
#17009=CARTESIAN_POINT('Ctrl Pts',(2.45823849561404,3.07010626830428,-33.417729676829));
#17010=CARTESIAN_POINT('Ctrl Pts',(2.54895178535895,2.99747200700299,-33.4235947741908));
#17011=CARTESIAN_POINT('Ctrl Pts',(2.63648246611203,2.92078236986249,-33.4294598715526));
#17012=CARTESIAN_POINT('Ctrl Pts',(2.72045628843409,2.84035324963628,-33.4353249689144));
#17013=CARTESIAN_POINT('Ctrl Pts',(2.80441888946648,2.75993487702679,-33.4411892825325));
#17014=CARTESIAN_POINT('Ctrl Pts',(2.8848252804178,2.67577829955866,-33.4470535961506));
#17015=CARTESIAN_POINT('Ctrl Pts',(2.96133680772466,2.58823749126991,-33.4529179097686));
#17016=CARTESIAN_POINT('Ctrl Pts',(3.03785640627714,2.50068744825025,-33.4587828420166));
#17017=CARTESIAN_POINT('Ctrl Pts',(3.1104800537526,2.4097527743698,-33.4646477742645));
#17018=CARTESIAN_POINT('Ctrl Pts',(3.17890871093214,2.31582132461892,-33.4705127065124));
#17019=CARTESIAN_POINT('Ctrl Pts',(3.2489759619245,2.21964059074156,-33.4765180805298));
#17020=CARTESIAN_POINT('Ctrl Pts',(3.31464448561763,2.12031809477642,-33.4825234545472));
#17021=CARTESIAN_POINT('Ctrl Pts',(3.37564039807835,2.0183014895851,-33.4885288285645));
#17022=CARTESIAN_POINT('Ctrl Pts',(3.43529693959773,1.91852500296919,-33.4944023343447));
#17023=CARTESIAN_POINT('Ctrl Pts',(3.49048381712388,1.81617189948764,-33.5002758401249));
#17024=CARTESIAN_POINT('Ctrl Pts',(3.5409920065088,1.71168472851772,-33.5061493459051));
#17025=CARTESIAN_POINT('Ctrl Pts',(3.59320116278114,1.60367873772582,-33.5122206540411));
#17026=CARTESIAN_POINT('Ctrl Pts',(3.64041075589718,1.49339285329059,-33.518291962177));
#17027=CARTESIAN_POINT('Ctrl Pts',(3.68244494504431,1.38133566764838,-33.524363270313));
#17028=CARTESIAN_POINT('Ctrl Pts',(3.72447913419144,1.26927848200616,-33.5304345784489));
#17029=CARTESIAN_POINT('Ctrl Pts',(3.761337833314,1.15545047029401,-33.5365058865849));
#17030=CARTESIAN_POINT('Ctrl Pts',(3.79290287308455,1.04037339227171,-33.5425771947208));
#17031=CARTESIAN_POINT('Ctrl Pts',(3.83119867671295,0.900757880486982,-33.5499431168243));
#17032=CARTESIAN_POINT('Ctrl Pts',(3.86180261359598,0.758949987624212,-33.5573090389277));
#17033=CARTESIAN_POINT('Ctrl Pts',(3.88450769868466,0.615701988675996,-33.5646749610311));
#17034=CARTESIAN_POINT('Ctrl Pts',(3.90687601725961,0.474578673648444,-33.5719316302559));
#17035=CARTESIAN_POINT('Ctrl Pts',(3.92157806086247,0.332057550685683,-33.5791882994806));
#17036=CARTESIAN_POINT('Ctrl Pts',(3.92846204140117,0.188878239271026,-33.5864449687053));
#17037=CARTESIAN_POINT('Ctrl Pts',(3.93143176781017,0.127111158446251,-33.5895754717793));
#17038=CARTESIAN_POINT('Ctrl Pts',(3.93294711680607,0.0652218550975597,
-33.5927059748534));
#17039=CARTESIAN_POINT('Ctrl Pts',(3.93299863980535,0.00327097680709954,
-33.5958364779274));
#17040=CARTESIAN_POINT('',(3.93299901959195,-0.00277702875856491,-34.8458364780034));
#17041=CARTESIAN_POINT('Ctrl Pts',(3.93299863980597,0.00327097606317273,
-33.595836477965));
#17042=CARTESIAN_POINT('Ctrl Pts',(3.93309624041199,-0.114083306980526,
-33.6017666270437));
#17043=CARTESIAN_POINT('Ctrl Pts',(3.9279367460832,-0.231548868260059,-33.6076967761224));
#17044=CARTESIAN_POINT('Ctrl Pts',(3.91751920417218,-0.348614808839455,
-33.613626925201));
#17045=CARTESIAN_POINT('Ctrl Pts',(3.90730826068607,-0.463359123152169,
-33.6194394688532));
#17046=CARTESIAN_POINT('Ctrl Pts',(3.89204593702237,-0.577719083384085,
-33.6252520125054));
#17047=CARTESIAN_POINT('Ctrl Pts',(3.87178389998692,-0.691215184875232,
-33.6310645561577));
#17048=CARTESIAN_POINT('Ctrl Pts',(3.85152588368495,-0.804688764564849,
-33.6368759463874));
#17049=CARTESIAN_POINT('Ctrl Pts',(3.82627019998669,-0.917298413337728,
-33.6426873366171));
#17050=CARTESIAN_POINT('Ctrl Pts',(3.79611999416202,-1.02857279271978,-33.6484987268469));
#17051=CARTESIAN_POINT('Ctrl Pts',(3.76596821706489,-1.1398529711457,-33.6543104199361));
#17052=CARTESIAN_POINT('Ctrl Pts',(3.73092152122106,-1.24979733697056,-33.6601221130254));
#17053=CARTESIAN_POINT('Ctrl Pts',(3.69113327348597,-1.35794851057202,-33.6659338061147));
#17054=CARTESIAN_POINT('Ctrl Pts',(3.64992675137281,-1.46995479333782,-33.6719526602595));
#17055=CARTESIAN_POINT('Ctrl Pts',(3.60363449834118,-1.58003720159471,-33.6779715144044));
#17056=CARTESIAN_POINT('Ctrl Pts',(3.55248123063851,-1.68771031458633,-33.6839903685493));
#17057=CARTESIAN_POINT('Ctrl Pts',(3.50301921804101,-1.79182348487604,-33.6898102243064));
#17058=CARTESIAN_POINT('Ctrl Pts',(3.44901280294868,-1.89368381053235,-33.6956300800636));
#17059=CARTESIAN_POINT('Ctrl Pts',(3.39071134500875,-1.99287871553413,-33.7014499358207));
#17060=CARTESIAN_POINT('Ctrl Pts',(3.32941963354287,-2.09716127914546,-33.7075682891595));
#17061=CARTESIAN_POINT('Ctrl Pts',(3.26338090755395,-2.19849730185159,-33.7136866424982));
#17062=CARTESIAN_POINT('Ctrl Pts',(3.19293463525649,-2.29644451598106,-33.719804995837));
#17063=CARTESIAN_POINT('Ctrl Pts',(3.12248836295904,-2.39439173011053,-33.7259233491757));
#17064=CARTESIAN_POINT('Ctrl Pts',(3.04763493272809,-2.48894976633921,-33.7320417025144));
#17065=CARTESIAN_POINT('Ctrl Pts',(2.96875942677061,-2.57972023017238,-33.7381600558532));
#17066=CARTESIAN_POINT('Ctrl Pts',(2.89289700477522,-2.66702321667546,-33.74404468502));
#17067=CARTESIAN_POINT('Ctrl Pts',(2.81305973462294,-2.75111579554493,-33.7499293141867));
#17068=CARTESIAN_POINT('Ctrl Pts',(2.72954960188932,-2.83161578799558,-33.7558139433535));
#17069=CARTESIAN_POINT('Ctrl Pts',(2.64614410503506,-2.91201491618913,-33.7616911992431));
#17070=CARTESIAN_POINT('Ctrl Pts',(2.55907519218587,-2.98883012786828,-33.7675684551328));
#17071=CARTESIAN_POINT('Ctrl Pts',(2.46868450730728,-3.06171288715663,-33.7734457110225));
#17072=CARTESIAN_POINT('Ctrl Pts',(2.37838321010869,-3.13452357241685,-33.7793171548723));
#17073=CARTESIAN_POINT('Ctrl Pts',(2.28476699406984,-3.20340928468332,-33.785188598722));
#17074=CARTESIAN_POINT('Ctrl Pts',(2.1882132186511,-3.26805934917354,-33.7910600425718));
#17075=CARTESIAN_POINT('Ctrl Pts',(2.09044786935521,-3.33352065412488,-33.797005162339));
#17076=CARTESIAN_POINT('Ctrl Pts',(1.98967103841307,-3.39463898224683,-33.8029502821063));
#17077=CARTESIAN_POINT('Ctrl Pts',(1.88630811055672,-3.45113469920372,-33.8088954018735));
#17078=CARTESIAN_POINT('Ctrl Pts',(1.78433646783499,-3.50686997281016,-33.8147604991711));
#17079=CARTESIAN_POINT('Ctrl Pts',(1.67984829521716,-3.55810611873482,-33.8206255964687));
#17080=CARTESIAN_POINT('Ctrl Pts',(1.57327926792445,-3.6046194452562,-33.8264906937663));
#17081=CARTESIAN_POINT('Ctrl Pts',(1.4667244833205,-3.65112655538572,-33.8323550072081));
#17082=CARTESIAN_POINT('Ctrl Pts',(1.35808977397541,-3.69291193697634,-33.8382193206498));
#17083=CARTESIAN_POINT('Ctrl Pts',(1.24783224668237,-3.72979941607315,-33.8440836340916));
#17084=CARTESIAN_POINT('Ctrl Pts',(1.13756309037341,-3.76669078574409,-33.8499485660507));
#17085=CARTESIAN_POINT('Ctrl Pts',(1.0256711658779,-3.79868309549359,-33.8558134980098));
#17086=CARTESIAN_POINT('Ctrl Pts',(0.912629587461413,-3.8256497795917,-33.8616784299689));
#17087=CARTESIAN_POINT('Ctrl Pts',(0.79688110965979,-3.85326220927852,-33.867683803887));
#17088=CARTESIAN_POINT('Ctrl Pts',(0.679927657319526,-3.87560514942635,
-33.873689177805));
#17089=CARTESIAN_POINT('Ctrl Pts',(0.562287838856864,-3.89259828215983,
-33.8796945517231));
#17090=CARTESIAN_POINT('Ctrl Pts',(0.447231208518604,-3.90921827203024,
-33.8855680569355));
#17091=CARTESIAN_POINT('Ctrl Pts',(0.331518464586647,-3.92072099962597,
-33.891441562148));
#17092=CARTESIAN_POINT('Ctrl Pts',(0.215638522254376,-3.92708403624368,
-33.8973150673604));
#17093=CARTESIAN_POINT('Ctrl Pts',(0.0958560709140378,-3.93366136195422,
-33.9033863756313));
#17094=CARTESIAN_POINT('Ctrl Pts',(-0.0241045538234508,-3.93474670906188,
-33.9094576839021));
#17095=CARTESIAN_POINT('Ctrl Pts',(-0.143706271518569,-3.93037371092448,
-33.915528992173));
#17096=CARTESIAN_POINT('Ctrl Pts',(-0.263307989213692,-3.92600071278707,
-33.9216003004438));
#17097=CARTESIAN_POINT('Ctrl Pts',(-0.382550328244256,-3.91616947300749,
-33.9276716087147));
#17098=CARTESIAN_POINT('Ctrl Pts',(-0.500906271424316,-3.90097191828495,
-33.9337429169855));
#17099=CARTESIAN_POINT('Ctrl Pts',(-0.615622924103891,-3.88624166849908,
-33.9396275404654));
#17100=CARTESIAN_POINT('Ctrl Pts',(-0.729871617218782,-3.8664234877586,
-33.9455121639452));
#17101=CARTESIAN_POINT('Ctrl Pts',(-0.843166860449312,-3.84155679971545,
-33.9513967874251));
#17102=CARTESIAN_POINT('Ctrl Pts',(-0.956320146799781,-3.81672126918036,
-33.9572740375787));
#17103=CARTESIAN_POINT('Ctrl Pts',(-1.06852196100831,-3.78684990002925,
-33.9631512877323));
#17104=CARTESIAN_POINT('Ctrl Pts',(-1.17929282290527,-3.7520337735479,-33.9690285378859));
#17105=CARTESIAN_POINT('Ctrl Pts',(-1.2899541422015,-3.71725207714119,-33.9748999759581));
#17106=CARTESIAN_POINT('Ctrl Pts',(-1.3991869340485,-3.67753547372865,-33.9807714140303));
#17107=CARTESIAN_POINT('Ctrl Pts',(-1.50652342501249,-3.63302575959607,
-33.9866428521026));
#17108=CARTESIAN_POINT('Ctrl Pts',(-1.61520693952953,-3.58795746903961,
-33.9925879740199));
#17109=CARTESIAN_POINT('Ctrl Pts',(-1.72194581173416,-3.53797502735493,
-33.9985330959372));
#17110=CARTESIAN_POINT('Ctrl Pts',(-1.82627147174328,-3.48327740949478,
-34.0044782178545));
#17111=CARTESIAN_POINT('Ctrl Pts',(-1.92919274833091,-3.42931610547832,
-34.0103433093108));
#17112=CARTESIAN_POINT('Ctrl Pts',(-2.02976501427928,-3.37076599738194,
-34.0162084007672));
#17113=CARTESIAN_POINT('Ctrl Pts',(-2.12756055287515,-3.30786564023534,
-34.0220734922235));
#17114=CARTESIAN_POINT('Ctrl Pts',(-2.22534302110393,-3.24497368971721,
-34.0279377998108));
#17115=CARTESIAN_POINT('Ctrl Pts',(-2.32034915424173,-3.17773286889969,
-34.0338021073981));
#17116=CARTESIAN_POINT('Ctrl Pts',(-2.41217889844789,-3.10642591443651,
-34.0396664149854));
#17117=CARTESIAN_POINT('Ctrl Pts',(-2.50401832797392,-3.03511143920031,
-34.0455313410836));
#17118=CARTESIAN_POINT('Ctrl Pts',(-2.59268037774681,-2.95973023001703,
-34.0513962671817));
#17119=CARTESIAN_POINT('Ctrl Pts',(-2.67779740387659,-2.88060585012803,
-34.0572611932799));
#17120=CARTESIAN_POINT('Ctrl Pts',(-2.76495285204481,-2.7995865628735,-34.0632665753497));
#17121=CARTESIAN_POINT('Ctrl Pts',(-2.8483909820269,-2.71464283968997,-34.0692719574195));
#17122=CARTESIAN_POINT('Ctrl Pts',(-2.92775741230827,-2.6261617495261,-34.0752773394894));
#17123=CARTESIAN_POINT('Ctrl Pts',(-3.0053808964421,-2.53962377025539,-34.081150838879));
#17124=CARTESIAN_POINT('Ctrl Pts',(-3.07910945607348,-2.44970254953049,
-34.0870243382687));
#17125=CARTESIAN_POINT('Ctrl Pts',(-3.14865335206111,-2.35679253829317,
-34.0928978376583));
#17126=CARTESIAN_POINT('Ctrl Pts',(-3.22053954046738,-2.26075324573149,
-34.0989691610682));
#17127=CARTESIAN_POINT('Ctrl Pts',(-3.28795393741286,-2.16152068481002,
-34.1050404844782));
#17128=CARTESIAN_POINT('Ctrl Pts',(-3.35062675256515,-2.05956047859604,
-34.1111118078881));
#17129=CARTESIAN_POINT('Ctrl Pts',(-3.41329956771743,-1.95760027238206,
-34.1171831312981));
#17130=CARTESIAN_POINT('Ctrl Pts',(-3.47123062580845,-1.85291287082147,
-34.123254454708));
#17131=CARTESIAN_POINT('Ctrl Pts',(-3.52420422986645,-1.74598784250962,
-34.1293257781179));
#17132=CARTESIAN_POINT('Ctrl Pts',(-3.57554882409555,-1.64235090314647,
-34.1352104001379));
#17133=CARTESIAN_POINT('Ctrl Pts',(-3.62239966877812,-1.53628245983126,
-34.1410950221579));
#17134=CARTESIAN_POINT('Ctrl Pts',(-3.66452039789657,-1.42820840685104,
-34.1469796441779));
#17135=CARTESIAN_POINT('Ctrl Pts',(-3.70658835021612,-1.32026976944123,
-34.1528568928328));
#17136=CARTESIAN_POINT('Ctrl Pts',(-3.74393782675065,-1.2103309004938,-34.1587341414877));
#17137=CARTESIAN_POINT('Ctrl Pts',(-3.77637878444347,-1.09884133358973,
-34.1646113901426));
#17138=CARTESIAN_POINT('Ctrl Pts',(-3.80878766068298,-0.987462020746884,
-34.1704828266793));
#17139=CARTESIAN_POINT('Ctrl Pts',(-3.83629756025312,-0.874535453351869,
-34.1763542632161));
#17140=CARTESIAN_POINT('Ctrl Pts',(-3.8587671369953,-0.760529540810288,
-34.1822256997529));
#17141=CARTESIAN_POINT('Ctrl Pts',(-3.88151870468208,-0.645092865449426,
-34.1881708222319));
#17142=CARTESIAN_POINT('Ctrl Pts',(-3.89910241080427,-0.528549965408921,
-34.194115944711));
#17143=CARTESIAN_POINT('Ctrl Pts',(-3.91142405295958,-0.411401115615005,
-34.20006106719));
#17144=CARTESIAN_POINT('Ctrl Pts',(-3.92357982241177,-0.295829311813609,
-34.2059261570303));
#17145=CARTESIAN_POINT('Ctrl Pts',(-3.93061429748689,-0.179668194380369,
-34.2117912468706));
#17146=CARTESIAN_POINT('Ctrl Pts',(-3.932488866005,-0.0634059835242513,
-34.2176563367108));
#17147=CARTESIAN_POINT('Ctrl Pts',(-3.93436318397833,0.0528406883477371,
-34.2235206426546));
#17148=CARTESIAN_POINT('Ctrl Pts',(-3.93107896035696,0.169188015656239,
-34.2293849485984));
#17149=CARTESIAN_POINT('Ctrl Pts',(-3.92264968935785,0.285146303817477,
-34.2352492545422));
#17150=CARTESIAN_POINT('Ctrl Pts',(-3.91421952935678,0.401116821641947,
-34.2411141789712));
#17151=CARTESIAN_POINT('Ctrl Pts',(-3.90064327308692,0.516697808568232,
-34.2469791034002));
#17152=CARTESIAN_POINT('Ctrl Pts',(-3.88198636099284,0.631403906438346,
-34.2528440278292));
#17153=CARTESIAN_POINT('Ctrl Pts',(-3.86288263202675,0.748857115919984,
-34.2588494121143));
#17154=CARTESIAN_POINT('Ctrl Pts',(-3.83845186018606,0.865392548235749,
-34.2648547963994));
#17155=CARTESIAN_POINT('Ctrl Pts',(-3.80881969032344,0.980500671394169,
-34.2708601806845));
#17156=CARTESIAN_POINT('Ctrl Pts',(-3.77983828423253,1.09308085965185,-34.2767336783563));
#17157=CARTESIAN_POINT('Ctrl Pts',(-3.74588176504571,1.20429540379539,-34.2826071760281));
#17158=CARTESIAN_POINT('Ctrl Pts',(-3.70711776117573,1.31368447687236,-34.2884806736999));
#17159=CARTESIAN_POINT('Ctrl Pts',(-3.66704811623616,1.42675796982645,-34.2945520012916));
#17160=CARTESIAN_POINT('Ctrl Pts',(-3.62184161023935,1.53788040401586,-34.3006233288834));
#17161=CARTESIAN_POINT('Ctrl Pts',(-3.57173616386766,1.64656909230069,-34.3066946564751));
#17162=CARTESIAN_POINT('Ctrl Pts',(-3.52163071749597,1.75525778058552,-34.3127659840668));
#17163=CARTESIAN_POINT('Ctrl Pts',(-3.46662660803095,1.86151232763336,-34.3188373116586));
#17164=CARTESIAN_POINT('Ctrl Pts',(-3.40701167590485,1.96488178785596,-34.3249086392503));
#17165=CARTESIAN_POINT('Ctrl Pts',(-3.34923000101901,2.0650724671152,-34.3307932635302));
#17166=CARTESIAN_POINT('Ctrl Pts',(-3.28693325400658,2.16287145976681,-34.3366778878101));
#17167=CARTESIAN_POINT('Ctrl Pts',(-3.22034482403828,2.25784592350538,-34.3425625120899));
#17168=CARTESIAN_POINT('Ctrl Pts',(-3.15383982820297,2.35270138590931,-34.3484397630389));
#17169=CARTESIAN_POINT('Ctrl Pts',(-3.08305407872684,2.44473902442852,-34.354317013988));
#17170=CARTESIAN_POINT('Ctrl Pts',(-3.00825632123417,2.53355144130817,-34.360194264937));
#17171=CARTESIAN_POINT('Ctrl Pts',(-2.93353253218,2.62227603047723,-34.366065703799));
#17172=CARTESIAN_POINT('Ctrl Pts',(-2.8548048913113,2.70778143004122,-34.3719371426609));
#17173=CARTESIAN_POINT('Ctrl Pts',(-2.77238443652447,2.78969058071265,-34.3778085815229));
#17174=CARTESIAN_POINT('Ctrl Pts',(-2.68892965838043,2.87262763820562,-34.3837537031421));
#17175=CARTESIAN_POINT('Ctrl Pts',(-2.60168898803608,2.95187721300267,-34.3896988247613));
#17176=CARTESIAN_POINT('Ctrl Pts',(-2.51102653650519,3.02708353584217,-34.3956439463804));
#17177=CARTESIAN_POINT('Ctrl Pts',(-2.42158452441485,3.10127747967556,-34.4015090386073));
#17178=CARTESIAN_POINT('Ctrl Pts',(-2.32881262063838,3.17153609527604,-34.4073741308341));
#17179=CARTESIAN_POINT('Ctrl Pts',(-2.23309572594469,3.23755655993337,-34.4132392230609));
#17180=CARTESIAN_POINT('Ctrl Pts',(-2.13739162394793,3.3035682008632,-34.41910353141));
#17181=CARTESIAN_POINT('Ctrl Pts',(-2.0387436523071,3.36534258394099,-34.424967839759));
#17182=CARTESIAN_POINT('Ctrl Pts',(-1.93756682863945,3.42261943320552,-34.430832148108));
#17183=CARTESIAN_POINT('Ctrl Pts',(-1.83637933397904,3.47990232338753,-34.4366970749583));
#17184=CARTESIAN_POINT('Ctrl Pts',(-1.73266281497774,3.5326865341732,-34.4425620018086));
#17185=CARTESIAN_POINT('Ctrl Pts',(-1.62685748141285,3.58075742478753,-34.4484269286589));
#17186=CARTESIAN_POINT('Ctrl Pts',(-1.51851830623253,3.62997952412666,-34.4544323096359));
#17187=CARTESIAN_POINT('Ctrl Pts',(-1.40798940641783,3.67425948458499,-34.4604376906129));
#17188=CARTESIAN_POINT('Ctrl Pts',(-1.29576448807703,3.71341936649208,-34.4664430715899));
#17189=CARTESIAN_POINT('Ctrl Pts',(-1.18600407939974,3.75171927978607,-34.4723165717006));
#17190=CARTESIAN_POINT('Ctrl Pts',(-1.07462179118489,3.785121614066,-34.4781900718112));
#17191=CARTESIAN_POINT('Ctrl Pts',(-0.962093242570019,3.81351092729536,
-34.4840635719219));
#17192=CARTESIAN_POINT('Ctrl Pts',(-0.84577469765106,3.84285640137047,-34.4901348933321));
#17193=CARTESIAN_POINT('Ctrl Pts',(-0.728231793541606,3.86684512381164,
-34.4962062147422));
#17194=CARTESIAN_POINT('Ctrl Pts',(-0.609998144737329,3.88540747714021,
-34.5022775361523));
#17195=CARTESIAN_POINT('Ctrl Pts',(-0.491764495933051,3.90396983046877,
-34.5083488575625));
#17196=CARTESIAN_POINT('Ctrl Pts',(-0.372840585171041,3.91710582625685,
-34.5144201789726));
#17197=CARTESIAN_POINT('Ctrl Pts',(-0.253761288374039,3.92480498987182,
-34.5204915003827));
#17198=CARTESIAN_POINT('Ctrl Pts',(-0.138343775920815,3.93226739800079,
-34.5263761237665));
#17199=CARTESIAN_POINT('Ctrl Pts',(-0.0224133461781239,3.93464621096049,
-34.5322607471504));
#17200=CARTESIAN_POINT('Ctrl Pts',(0.0935459234724902,3.93188735344766,
-34.5381453705342));
#17201=CARTESIAN_POINT('Ctrl Pts',(0.209359897989908,3.92913195273972,-34.5440226205779));
#17202=CARTESIAN_POINT('Ctrl Pts',(0.325202232851273,3.92125169474425,-34.5498998706215));
#17203=CARTESIAN_POINT('Ctrl Pts',(0.440584878799683,3.9082443583498,-34.5557771206652));
#17204=CARTESIAN_POINT('Ctrl Pts',(0.555853421229502,3.89524988509294,-34.5616485586138));
#17205=CARTESIAN_POINT('Ctrl Pts',(0.670662772626538,3.87713846563527,-34.5675199965624));
#17206=CARTESIAN_POINT('Ctrl Pts',(0.7845266835988,3.85395989635614,-34.573391434511));
#17207=CARTESIAN_POINT('Ctrl Pts',(0.899819537466818,3.83049044604525,-34.5793365564695));
#17208=CARTESIAN_POINT('Ctrl Pts',(1.01414262987097,3.80182579812155,-34.585281678428));
#17209=CARTESIAN_POINT('Ctrl Pts',(1.12699800331394,3.76807172178641,-34.5912268003865));
#17210=CARTESIAN_POINT('Ctrl Pts',(1.23833416655996,3.73477202821916,-34.597091891686));
#17211=CARTESIAN_POINT('Ctrl Pts',(1.34824148095915,3.69651921823463,-34.6029569829856));
#17212=CARTESIAN_POINT('Ctrl Pts',(1.45625452603846,3.653465718382,-34.6088220742852));
#17213=CARTESIAN_POINT('Ctrl Pts',(1.56425313495665,3.61041797271638,-34.6146863817035));
#17214=CARTESIAN_POINT('Ctrl Pts',(1.67035759613018,3.56257096550373,-34.6205506891218));
#17215=CARTESIAN_POINT('Ctrl Pts',(1.77412119952072,3.51012577686486,-34.62641499654));
#17216=CARTESIAN_POINT('Ctrl Pts',(1.87789574668625,3.45767505691902,-34.6322799224571));
#17217=CARTESIAN_POINT('Ctrl Pts',(1.97932857822698,3.40062537699027,-34.6381448483742));
#17218=CARTESIAN_POINT('Ctrl Pts',(2.0779969952556,3.33922408468026,-34.6440097742912));
#17219=CARTESIAN_POINT('Ctrl Pts',(2.17902837578433,3.27635232170741,-34.6500151565599));
#17220=CARTESIAN_POINT('Ctrl Pts',(2.27716085985052,3.2089180970275,-34.6560205388285));
#17221=CARTESIAN_POINT('Ctrl Pts',(2.37197263114538,3.13723362807064,-34.6620259210972));
#17222=CARTESIAN_POINT('Ctrl Pts',(2.46470225867718,3.06712340847026,-34.6678994202772));
#17223=CARTESIAN_POINT('Ctrl Pts',(2.55425523969155,2.99294801054815,-34.6737729194572));
#17224=CARTESIAN_POINT('Ctrl Pts',(2.64027179851076,2.91503925016264,-34.6796464186373));
#17225=CARTESIAN_POINT('Ctrl Pts',(2.72918547089927,2.8345064540103,-34.6857177424502));
#17226=CARTESIAN_POINT('Ctrl Pts',(2.81431995726265,2.74998471745796,-34.6917890662632));
#17227=CARTESIAN_POINT('Ctrl Pts',(2.89532146271884,2.66187952911465,-34.6978603900762));
#17228=CARTESIAN_POINT('Ctrl Pts',(2.97632296817504,2.57377434077133,-34.7039317138891));
#17229=CARTESIAN_POINT('Ctrl Pts',(3.05319123470526,2.48208610879974,-34.7100030377021));
#17230=CARTESIAN_POINT('Ctrl Pts',(3.12562098824291,2.38725416281037,-34.716074361515));
#17231=CARTESIAN_POINT('Ctrl Pts',(3.19582130929989,2.29534120260056,-34.7219588062369));
#17232=CARTESIAN_POINT('Ctrl Pts',(3.26207947609405,2.20017791712166,-34.7278432509588));
#17233=CARTESIAN_POINT('Ctrl Pts',(3.32408079320321,2.10213602800997,-34.7337276956806));
#17234=CARTESIAN_POINT('Ctrl Pts',(3.38600596947555,2.00421453942891,-34.7396049139988));
#17235=CARTESIAN_POINT('Ctrl Pts',(3.44368447223116,1.9034218193157,-34.745482132317));
#17236=CARTESIAN_POINT('Ctrl Pts',(3.49684230894722,1.8001619000403,-34.7513593506352));
#17237=CARTESIAN_POINT('Ctrl Pts',(3.54994754095069,1.69700416623199,-34.7572307528894));
#17238=CARTESIAN_POINT('Ctrl Pts',(3.59854081669175,1.59138445150422,-34.7631021551436));
#17239=CARTESIAN_POINT('Ctrl Pts',(3.64239224160431,1.48373439614398,-34.7689735573978));
#17240=CARTESIAN_POINT('Ctrl Pts',(3.68621072592521,1.3761652060355,-34.7748405491348));
#17241=CARTESIAN_POINT('Ctrl Pts',(3.72529429092247,1.26656908823968,-34.7807075408718));
#17242=CARTESIAN_POINT('Ctrl Pts',(3.75945997591371,1.15540022914264,-34.7865745326088));
#17243=CARTESIAN_POINT('Ctrl Pts',(3.79361010033921,1.04428200126641,-34.792438852258));
#17244=CARTESIAN_POINT('Ctrl Pts',(3.82284667914449,0.931592848625983,-34.7983031719072));
#17245=CARTESIAN_POINT('Ctrl Pts',(3.84703590292379,0.81780423183997,-34.8041674915563));
#17246=CARTESIAN_POINT('Ctrl Pts',(3.87121878030779,0.70404546915547,-34.8100302726158));
#17247=CARTESIAN_POINT('Ctrl Pts',(3.89035685524024,0.589188218375522,-34.8158930536753));
#17248=CARTESIAN_POINT('Ctrl Pts',(3.90436711264923,0.473715578868916,-34.8217558347347));
#17249=CARTESIAN_POINT('Ctrl Pts',(3.91837958235046,0.358224705634153,-34.8276195415577));
#17250=CARTESIAN_POINT('Ctrl Pts',(3.92726256756757,0.242118657273612,-34.8334832483807));
#17251=CARTESIAN_POINT('Ctrl Pts',(3.93098480463834,0.125886717736397,-34.8393469552036));
#17252=CARTESIAN_POINT('Ctrl Pts',(3.93235797141511,0.0830077084910385,
-34.8415101294574));
#17253=CARTESIAN_POINT('Ctrl Pts',(3.93302930256552,0.0401115937067086,
-34.8436733037112));
#17254=CARTESIAN_POINT('Ctrl Pts',(3.93299901959249,-0.00277702799701734,
-34.845836477965));
#17255=CARTESIAN_POINT('',(3.93299981803602,0.00119638148616161,-36.0958364779956));
#17256=CARTESIAN_POINT('Ctrl Pts',(3.93299901959195,-0.00277702875855888,
-34.8458364780034));
#17257=CARTESIAN_POINT('Ctrl Pts',(3.93290411654262,-0.137184567338229,
-34.8526155936621));
#17258=CARTESIAN_POINT('Ctrl Pts',(3.92591531627658,-0.271321633643327,
-34.8593947093209));
#17259=CARTESIAN_POINT('Ctrl Pts',(3.91213938866519,-0.404542214922395,
-34.8661738249796));
#17260=CARTESIAN_POINT('Ctrl Pts',(3.89828763983609,-0.538496027892523,
-34.8729902521588));
#17261=CARTESIAN_POINT('Ctrl Pts',(3.87757395605432,-0.671523115649326,
-34.8798066793379));
#17262=CARTESIAN_POINT('Ctrl Pts',(3.85015627438072,-0.802985468639864,
-34.886623106517));
#17263=CARTESIAN_POINT('Ctrl Pts',(3.82257135468943,-0.935249694800271,
-34.8934811114555));
#17264=CARTESIAN_POINT('Ctrl Pts',(3.78820048763923,-1.06592991939294,-34.9003391163939));
#17265=CARTESIAN_POINT('Ctrl Pts',(3.74725292585918,-1.19439713229722,-34.9071971213324));
#17266=CARTESIAN_POINT('Ctrl Pts',(3.73837618129646,-1.22224666921866,-34.9086838217707));
#17267=CARTESIAN_POINT('Ctrl Pts',(3.72919054225404,-1.2499922865566,-34.9101705222091));
#17268=CARTESIAN_POINT('Ctrl Pts',(3.71969843258908,-1.27762771204853,-34.9116572226475));
#17269=CARTESIAN_POINT('Ctrl Pts',(3.68212698190591,-1.38701361914676,-34.9175418462109));
#17270=CARTESIAN_POINT('Ctrl Pts',(3.63966663410879,-1.49491469887107,-34.9234264697742));
#17271=CARTESIAN_POINT('Ctrl Pts',(3.59245394985051,-1.6008633977337,-34.9293110933376));
#17272=CARTESIAN_POINT('Ctrl Pts',(3.54530042233089,-1.70667934457029,-34.9351883435618));
#17273=CARTESIAN_POINT('Ctrl Pts',(3.49340656754212,-1.81054740353643,-34.9410655937859));
#17274=CARTESIAN_POINT('Ctrl Pts',(3.43695832899016,-1.9120163296335,-34.94694284401));
#17275=CARTESIAN_POINT('Ctrl Pts',(3.3805659128858,-2.01338491169939,-34.9528142821397));
#17276=CARTESIAN_POINT('Ctrl Pts',(3.31962827159465,-2.11235872321046,-34.9586857202694));
#17277=CARTESIAN_POINT('Ctrl Pts',(3.25437865893949,-2.20850821692815,-34.9645571583991));
#17278=CARTESIAN_POINT('Ctrl Pts',(3.18831019462166,-2.30586434114666,-34.97050228029));
#17279=CARTESIAN_POINT('Ctrl Pts',(3.11782096049279,-2.40032438035578,-34.9764474021809));
#17280=CARTESIAN_POINT('Ctrl Pts',(3.04320037395452,-2.49146954305347,-34.9823925240717));
#17281=CARTESIAN_POINT('Ctrl Pts',(2.9695842943429,-2.58138775282158,-34.9882576155528));
#17282=CARTESIAN_POINT('Ctrl Pts',(2.89194768309327,-2.66807946298302,-34.9941227070339));
#17283=CARTESIAN_POINT('Ctrl Pts',(2.81061048168482,-2.75117388040876,-34.9999877985149));
#17284=CARTESIAN_POINT('Ctrl Pts',(2.72928415115963,-2.83425719209574,-35.0058521061146));
#17285=CARTESIAN_POINT('Ctrl Pts',(2.64425850175204,-2.91374387342072,-35.0117164137142));
#17286=CARTESIAN_POINT('Ctrl Pts',(2.55589116707806,-2.98929913893748,-35.0175807213138));
#17287=CARTESIAN_POINT('Ctrl Pts',(2.46751451245395,-3.06486237313758,-35.0234456474118));
#17288=CARTESIAN_POINT('Ctrl Pts',(2.37579578451845,-3.13649309998798,-35.0293105735098));
#17289=CARTESIAN_POINT('Ctrl Pts',(2.28112606525489,-3.20389651431109,-35.0351754996078));
#17290=CARTESIAN_POINT('Ctrl Pts',(2.18418915251842,-3.27291413624138,-35.0411808816221));
#17291=CARTESIAN_POINT('Ctrl Pts',(2.08415847107028,-3.33749912379196,-35.0471862636364));
#17292=CARTESIAN_POINT('Ctrl Pts',(1.98148462704563,-3.39738247372618,-35.0531916456508));
#17293=CARTESIAN_POINT('Ctrl Pts',(1.88106557700872,-3.45595074075219,-35.059065145009));
#17294=CARTESIAN_POINT('Ctrl Pts',(1.77811865621738,-3.51002160514262,-35.0649386443673));
#17295=CARTESIAN_POINT('Ctrl Pts',(1.67308865941643,-3.55939086610787,-35.0708121437255));
#17296=CARTESIAN_POINT('Ctrl Pts',(1.56452117139397,-3.61042292182316,-35.0768834670679));
#17297=CARTESIAN_POINT('Ctrl Pts',(1.45372826226303,-3.65643089712131,-35.0829547904103));
#17298=CARTESIAN_POINT('Ctrl Pts',(1.34122041071177,-3.69724448879029,-35.0890261137527));
#17299=CARTESIAN_POINT('Ctrl Pts',(1.22871255916052,-3.73805808045926,-35.095097437095));
#17300=CARTESIAN_POINT('Ctrl Pts',(1.11449024124293,-3.77367720761152,-35.1011687604374));
#17301=CARTESIAN_POINT('Ctrl Pts',(0.999076475456495,-3.80398937908473,
-35.1072400837798));
#17302=CARTESIAN_POINT('Ctrl Pts',(0.887211810708316,-3.83336941773553,
-35.1131247072096));
#17303=CARTESIAN_POINT('Ctrl Pts',(0.773872255728606,-3.85785755251595,
-35.1190093306395));
#17304=CARTESIAN_POINT('Ctrl Pts',(0.659522634313266,-3.87730820219756,
-35.1248939540693));
#17305=CARTESIAN_POINT('Ctrl Pts',(0.54531629118452,-3.89673448051943,-35.130771204158));
#17306=CARTESIAN_POINT('Ctrl Pts',(0.430102800820088,-3.91113575917428,
-35.1366484542468));
#17307=CARTESIAN_POINT('Ctrl Pts',(0.314360794522347,-3.92041659659624,
-35.1425257043355));
#17308=CARTESIAN_POINT('Ctrl Pts',(0.198733247138435,-3.92968825606627,
-35.1483971423282));
#17309=CARTESIAN_POINT('Ctrl Pts',(0.0825786312786711,-3.93384951493226,
-35.1542685803209));
#17310=CARTESIAN_POINT('Ctrl Pts',(-0.033616248424685,-3.93285633450319,
-35.1601400183135));
#17311=CARTESIAN_POINT('Ctrl Pts',(-0.151269322456923,-3.93185069009917,
-35.1660851402551));
#17312=CARTESIAN_POINT('Ctrl Pts',(-0.268963256133996,-3.92556027080728,
-35.1720302621967));
#17313=CARTESIAN_POINT('Ctrl Pts',(-0.386189056632202,-3.91399374201563,
-35.1779753841383));
#17314=CARTESIAN_POINT('Ctrl Pts',(-0.501836815279357,-3.90258291671611,
-35.1838404754792));
#17315=CARTESIAN_POINT('Ctrl Pts',(-0.617028546701187,-3.88603720961323,
-35.1897055668201));
#17316=CARTESIAN_POINT('Ctrl Pts',(-0.731278279749321,-3.86441730116804,
-35.195570658161));
#17317=CARTESIAN_POINT('Ctrl Pts',(-0.845512743068666,-3.84280028227129,
-35.2014349656195));
#17318=CARTESIAN_POINT('Ctrl Pts',(-0.958805054411566,-3.81611048726668,
-35.207299273078));
#17319=CARTESIAN_POINT('Ctrl Pts',(-1.07067831106139,-3.78445992900212,
-35.2131635805365));
#17320=CARTESIAN_POINT('Ctrl Pts',(-1.18256336677593,-3.75280603261193,
-35.2190285064926));
#17321=CARTESIAN_POINT('Ctrl Pts',(-1.29302867453848,-3.71619044482881,
-35.2248934324488));
#17322=CARTESIAN_POINT('Ctrl Pts',(-1.40161205905972,-3.67477518168096,
-35.2307583584049));
#17323=CARTESIAN_POINT('Ctrl Pts',(-1.51279585412699,-3.6323680845842,-35.2367637406138));
#17324=CARTESIAN_POINT('Ctrl Pts',(-1.62200601345193,-3.58492865021709,
-35.2427691228228));
#17325=CARTESIAN_POINT('Ctrl Pts',(-1.72876883209973,-3.53268273768825,
-35.2487745050317));
#17326=CARTESIAN_POINT('Ctrl Pts',(-1.83318705391937,-3.48158418715631,
-35.2546480042475));
#17327=CARTESIAN_POINT('Ctrl Pts',(-1.93526398218542,-3.42588834359902,
-35.2605215034633));
#17328=CARTESIAN_POINT('Ctrl Pts',(-2.03458306425122,-3.36585215876487,
-35.2663950026791));
#17329=CARTESIAN_POINT('Ctrl Pts',(-2.13724729816016,-3.30379390374867,
-35.2724663263846));
#17330=CARTESIAN_POINT('Ctrl Pts',(-2.23696423412104,-3.23709804963224,
-35.2785376500901));
#17331=CARTESIAN_POINT('Ctrl Pts',(-2.33330911196602,-3.16609500615764,
-35.2846089737956));
#17332=CARTESIAN_POINT('Ctrl Pts',(-2.429653989811,-3.09509196268304,-35.2906802975011));
#17333=CARTESIAN_POINT('Ctrl Pts',(-2.52262647828011,-3.01978208118662,
-35.2967516212066));
#17334=CARTESIAN_POINT('Ctrl Pts',(-2.61184297721808,-2.94053826065171,
-35.3028229449121));
#17335=CARTESIAN_POINT('Ctrl Pts',(-2.6983159669777,-2.86373127805096,-35.3087075684836));
#17336=CARTESIAN_POINT('Ctrl Pts',(-2.78153553523632,-2.78298459042336,
-35.3145921920551));
#17337=CARTESIAN_POINT('Ctrl Pts',(-2.8611228090182,-2.69860431922054,-35.3204768156265));
#17338=CARTESIAN_POINT('Ctrl Pts',(-2.94061036119725,-2.61432977517098,
-35.3263540658572));
#17339=CARTESIAN_POINT('Ctrl Pts',(-3.0164743910532,-2.5264309993937,-35.3322313160878));
#17340=CARTESIAN_POINT('Ctrl Pts',(-3.08837009760411,-2.43525340369842,
-35.3381085663184));
#17341=CARTESIAN_POINT('Ctrl Pts',(-3.16019470547257,-2.34416597481887,
-35.3439800044531));
#17342=CARTESIAN_POINT('Ctrl Pts',(-3.228058543559,-2.2498064975538,-35.3498514425877));
#17343=CARTESIAN_POINT('Ctrl Pts',(-3.29165505796186,-2.15255568555011,
-35.3557228807224));
#17344=CARTESIAN_POINT('Ctrl Pts',(-3.35604967834843,-2.05408442214732,
-35.3616680026108));
#17345=CARTESIAN_POINT('Ctrl Pts',(-3.41606883728247,-1.95264906512456,
-35.3676131244992));
#17346=CARTESIAN_POINT('Ctrl Pts',(-3.47143754046562,-1.84867801486522,
-35.3735582463876));
#17347=CARTESIAN_POINT('Ctrl Pts',(-3.52606089647284,-1.7461065734866,-35.3794233378698));
#17348=CARTESIAN_POINT('Ctrl Pts',(-3.5761580415076,-1.64106766609363,-35.385288429352));
#17349=CARTESIAN_POINT('Ctrl Pts',(-3.62151003356077,-1.53399937314806,
-35.3911535208341));
#17350=CARTESIAN_POINT('Ctrl Pts',(-3.66685596421629,-1.42694539012519,
-35.3970178284334));
#17351=CARTESIAN_POINT('Ctrl Pts',(-3.70745784284173,-1.31786293958858,
-35.4028821360326));
#17352=CARTESIAN_POINT('Ctrl Pts',(-3.74314447536411,-1.20721101575124,
-35.4087464436319));
#17353=CARTESIAN_POINT('Ctrl Pts',(-3.77883487168513,-1.09654742167408,
-35.414611369728));
#17354=CARTESIAN_POINT('Ctrl Pts',(-3.80960886511949,-0.984314416649301,
-35.4204762958242));
#17355=CARTESIAN_POINT('Ctrl Pts',(-3.83534504090498,-0.870986462125324,
-35.4263412219204));
#17356=CARTESIAN_POINT('Ctrl Pts',(-3.86169755831827,-0.754944478269699,
-35.4323466039307));
#17357=CARTESIAN_POINT('Ctrl Pts',(-3.88276778282798,-0.637754873362918,
-35.4383519859411));
#17358=CARTESIAN_POINT('Ctrl Pts',(-3.89848103892302,-0.519937101155188,
-35.4443573679514));
#17359=CARTESIAN_POINT('Ctrl Pts',(-3.91384922022218,-0.404706694891866,
-35.4502308673043));
#17360=CARTESIAN_POINT('Ctrl Pts',(-3.92409331811529,-0.288875846870358,
-35.4561043666572));
#17361=CARTESIAN_POINT('Ctrl Pts',(-3.92919622061545,-0.172933686427134,
-35.46197786601));
#17362=CARTESIAN_POINT('Ctrl Pts',(-3.93447099280575,-0.0530865046378151,
-35.4680491893491));
#17363=CARTESIAN_POINT('Ctrl Pts',(-3.93425214587245,0.0668791348487649,
-35.4741205126882));
#17364=CARTESIAN_POINT('Ctrl Pts',(-3.92857915073386,0.186426544298882,
-35.4801918360273));
#17365=CARTESIAN_POINT('Ctrl Pts',(-3.92290615559527,0.305973953748994,
-35.4862631593664));
#17366=CARTESIAN_POINT('Ctrl Pts',(-3.91177912097813,0.425102662685562,
-35.4923344827054));
#17367=CARTESIAN_POINT('Ctrl Pts',(-3.89529569908986,0.543286679987709,
-35.4984058060445));
#17368=CARTESIAN_POINT('Ctrl Pts',(-3.87931916098607,0.657836405674736,
-35.5042904293542));
#17369=CARTESIAN_POINT('Ctrl Pts',(-3.85826008052821,0.771862885642022,
-35.5101750526639));
#17370=CARTESIAN_POINT('Ctrl Pts',(-3.83216315702605,0.884881086888037,
-35.5160596759736));
#17371=CARTESIAN_POINT('Ctrl Pts',(-3.8060989325574,0.997757678110552,-35.5219369259431));
#17372=CARTESIAN_POINT('Ctrl Pts',(-3.77500951150435,1.10962810597062,-35.5278141759126));
#17373=CARTESIAN_POINT('Ctrl Pts',(-3.73899118241851,1.22001390885376,-35.5336914258821));
#17374=CARTESIAN_POINT('Ctrl Pts',(-3.70300847236422,1.33029054966591,-35.5395628637566));
#17375=CARTESIAN_POINT('Ctrl Pts',(-3.66210667767968,1.43908509731551,-35.545434301631));
#17376=CARTESIAN_POINT('Ctrl Pts',(-3.61643267165019,1.54593134757695,-35.5513057395055));
#17377=CARTESIAN_POINT('Ctrl Pts',(-3.57018547577501,1.65411847399581,-35.5572508614918));
#17378=CARTESIAN_POINT('Ctrl Pts',(-3.51904556041223,1.7603076483752,-35.5631959834781));
#17379=CARTESIAN_POINT('Ctrl Pts',(-3.46321698282404,1.86403249163719,-35.5691411054644));
#17380=CARTESIAN_POINT('Ctrl Pts',(-3.40813994633525,1.96636103418532,-35.5750061966904));
#17381=CARTESIAN_POINT('Ctrl Pts',(-3.34849991474435,2.06629081748993,-35.5808712879163));
#17382=CARTESIAN_POINT('Ctrl Pts',(-3.28454007888917,2.16339674358883,-35.5867363791423));
#17383=CARTESIAN_POINT('Ctrl Pts',(-3.22058879139169,2.26048969128994,-35.5926006864873));
#17384=CARTESIAN_POINT('Ctrl Pts',(-3.15231907405219,2.35475918902425,-35.5984649938323));
#17385=CARTESIAN_POINT('Ctrl Pts',(-3.08001799598553,2.44580828038612,-35.6043293011773));
#17386=CARTESIAN_POINT('Ctrl Pts',(-3.00770929243914,2.53686697455085,-35.6101942270214));
#17387=CARTESIAN_POINT('Ctrl Pts',(-2.93136863868749,2.62470426506676,-35.6160591528656));
#17388=CARTESIAN_POINT('Ctrl Pts',(-2.85132357567657,2.70895604740848,-35.6219240787098));
#17389=CARTESIAN_POINT('Ctrl Pts',(-2.76936154867657,2.79522553860931,-35.627929461082));
#17390=CARTESIAN_POINT('Ctrl Pts',(-2.68351573030301,2.87773526593777,-35.6339348434543));
#17391=CARTESIAN_POINT('Ctrl Pts',(-2.59417701938815,2.95613507676466,-35.6399402258266));
#17392=CARTESIAN_POINT('Ctrl Pts',(-2.50680026193911,3.0328131616007,-35.6458137249352));
#17393=CARTESIAN_POINT('Ctrl Pts',(-2.41608280721572,3.10555977107576,-35.6516872240439));
#17394=CARTESIAN_POINT('Ctrl Pts',(-2.32242223273743,3.17408947146846,-35.6575607231526));
#17395=CARTESIAN_POINT('Ctrl Pts',(-2.22560708327707,3.24492731570493,-35.6636320471567));
#17396=CARTESIAN_POINT('Ctrl Pts',(-2.12564746892987,3.311258915708,-35.6697033711607));
#17397=CARTESIAN_POINT('Ctrl Pts',(-2.02301191846946,3.37281955902336,-35.6757746951648));
#17398=CARTESIAN_POINT('Ctrl Pts',(-1.92037636800905,3.43438020233871,-35.6818460191688));
#17399=CARTESIAN_POINT('Ctrl Pts',(-1.81506533326051,3.49116971860004,-35.6879173431729));
#17400=CARTESIAN_POINT('Ctrl Pts',(-1.70757069904962,3.54297774587241,-35.6939886671769));
#17401=CARTESIAN_POINT('Ctrl Pts',(-1.60338165575405,3.59319261321128,-35.6998732905738));
#17402=CARTESIAN_POINT('Ctrl Pts',(-1.49681010637261,3.63888755925846,-35.7057579139707));
#17403=CARTESIAN_POINT('Ctrl Pts',(-1.38828449001756,3.67983086225124,-35.7116425373676));
#17404=CARTESIAN_POINT('Ctrl Pts',(-1.27989485459223,3.72072286391448,-35.7175197874218));
#17405=CARTESIAN_POINT('Ctrl Pts',(-1.1695564034432,3.75687492005202,-35.723397037476));
#17406=CARTESIAN_POINT('Ctrl Pts',(-1.05772070994583,3.7881018861366,-35.7292742875302));
#17407=CARTESIAN_POINT('Ctrl Pts',(-0.945995612383948,3.81929797142259,
-35.7351457254868));
#17408=CARTESIAN_POINT('Ctrl Pts',(-0.832776611923762,3.84557854566843,
-35.7410171634434));
#17409=CARTESIAN_POINT('Ctrl Pts',(-0.718533127238244,3.86680735815236,
-35.7468886014));
#17410=CARTESIAN_POINT('Ctrl Pts',(-0.602855936405293,3.88830258301897,
-35.7528337233546));
#17411=CARTESIAN_POINT('Ctrl Pts',(-0.486128770665354,3.90461822605745,
-35.7587788453091));
#17412=CARTESIAN_POINT('Ctrl Pts',(-0.368852899251572,3.91566552947436,
-35.7647239672637));
#17413=CARTESIAN_POINT('Ctrl Pts',(-0.253155744754137,3.92656411888408,
-35.770589058565));
#17414=CARTESIAN_POINT('Ctrl Pts',(-0.136924988936943,3.93233530731509,
-35.7764541498663));
#17415=CARTESIAN_POINT('Ctrl Pts',(-0.020649243143645,3.93294579275606,
-35.7823192411676));
#17416=CARTESIAN_POINT('Ctrl Pts',(0.0956109621152175,3.93355619660417,
-35.7881835485852));
#17417=CARTESIAN_POINT('Ctrl Pts',(0.211915734229722,3.92900726708336,-35.7940478560029));
#17418=CARTESIAN_POINT('Ctrl Pts',(0.327775554067432,3.91931782152912,-35.7999121634206));
#17419=CARTESIAN_POINT('Ctrl Pts',(0.44364759340196,3.909627354049,-35.8057770893347));
#17420=CARTESIAN_POINT('Ctrl Pts',(0.559074177333016,3.89479532703279,-35.8116420152488));
#17421=CARTESIAN_POINT('Ctrl Pts',(0.673570687652138,3.87489245382834,-35.8175069411629));
#17422=CARTESIAN_POINT('Ctrl Pts',(0.79080922096394,3.85451293608866,-35.8235123234251));
#17423=CARTESIAN_POINT('Ctrl Pts',(0.907072117552487,3.82881667211364,-35.8295177056873));
#17424=CARTESIAN_POINT('Ctrl Pts',(1.02185124222059,3.79793483866854,-35.8355230879495));
#17425=CARTESIAN_POINT('Ctrl Pts',(1.1341097237269,3.76773119546511,-35.8413965871208));
#17426=CARTESIAN_POINT('Ctrl Pts',(1.24494855309132,3.73256757789242,-35.8472700862921));
#17427=CARTESIAN_POINT('Ctrl Pts',(1.3539097527593,3.6926166036272,-35.8531435854633));
#17428=CARTESIAN_POINT('Ctrl Pts',(1.4665408618073,3.65132004528578,-35.859214909271));
#17429=CARTESIAN_POINT('Ctrl Pts',(1.5771651834653,3.60490814754724,-35.8652862330786));
#17430=CARTESIAN_POINT('Ctrl Pts',(1.68530264677118,3.55362406407685,-35.8713575568863));
#17431=CARTESIAN_POINT('Ctrl Pts',(1.79344011007705,3.50233998060646,-35.8774288806939));
#17432=CARTESIAN_POINT('Ctrl Pts',(1.89909032273816,3.44618399296587,-35.8835002045016));
#17433=CARTESIAN_POINT('Ctrl Pts',(2.00180549605808,3.38544882636729,-35.8895715283092));
#17434=CARTESIAN_POINT('Ctrl Pts',(2.1013620714965,3.32658132899761,-35.8954561526265));
#17435=CARTESIAN_POINT('Ctrl Pts',(2.19847801556756,3.26322502789782,-35.9013407769437));
#17436=CARTESIAN_POINT('Ctrl Pts',(2.29272294013962,3.19560800470858,-35.9072254012609));
#17437=CARTESIAN_POINT('Ctrl Pts',(2.38684977736114,3.12807570454455,-35.91310265224));
#17438=CARTESIAN_POINT('Ctrl Pts',(2.47811241854201,3.05629353807602,-35.9189799032191));
#17439=CARTESIAN_POINT('Ctrl Pts',(2.56610641169226,2.980534664095,-35.9248571541983));
#17440=CARTESIAN_POINT('Ctrl Pts',(2.65401338637372,2.90485070910531,-35.9307285930831));
#17441=CARTESIAN_POINT('Ctrl Pts',(2.73865783338161,2.82519813675476,-35.936600031968));
#17442=CARTESIAN_POINT('Ctrl Pts',(2.81966609718282,2.74189206578191,-35.9424714708529));
#17443=CARTESIAN_POINT('Ctrl Pts',(2.90169096178298,2.65754055803096,-35.9484165924608));
#17444=CARTESIAN_POINT('Ctrl Pts',(2.979987402897,2.56944347077906,-35.9543617140686));
#17445=CARTESIAN_POINT('Ctrl Pts',(3.05420363075142,2.4779687612851,-35.9603068356765));
#17446=CARTESIAN_POINT('Ctrl Pts',(3.12742080782104,2.38772542507636,-35.9661719279083));
#17447=CARTESIAN_POINT('Ctrl Pts',(3.196666687942,2.29419517737096,-35.9720370201401));
#17448=CARTESIAN_POINT('Ctrl Pts',(3.26164265077544,2.19776618834729,-35.9779021123719));
#17449=CARTESIAN_POINT('Ctrl Pts',(3.32660992940628,2.10135008730311,-35.9837664207193));
#17450=CARTESIAN_POINT('Ctrl Pts',(3.3873081959877,2.0020363564448,-35.9896307290666));
#17451=CARTESIAN_POINT('Ctrl Pts',(3.44348170183205,1.90024281847026,-35.9954950374139));
#17452=CARTESIAN_POINT('Ctrl Pts',(3.49966113216127,1.79843854457555,-36.0013599642558));
#17453=CARTESIAN_POINT('Ctrl Pts',(3.55131465437506,1.6941543037207,-36.0072248910976));
#17454=CARTESIAN_POINT('Ctrl Pts',(3.59823242615284,1.58783261314983,-36.0130898179395));
#17455=CARTESIAN_POINT('Ctrl Pts',(3.6462737915181,1.47896471534855,-36.019095198898));
#17456=CARTESIAN_POINT('Ctrl Pts',(3.68934950422021,1.36796095135993,-36.0251005798565));
#17457=CARTESIAN_POINT('Ctrl Pts',(3.72728700246295,1.2553169325994,-36.031105960815));
#17458=CARTESIAN_POINT('Ctrl Pts',(3.76439137614381,1.14514662726556,-36.0369794609007));
#17459=CARTESIAN_POINT('Ctrl Pts',(3.79658082777674,1.03340778284127,-36.0428529609865));
#17460=CARTESIAN_POINT('Ctrl Pts',(3.82374509287204,0.920577245393874,-36.0487264610722));
#17461=CARTESIAN_POINT('Ctrl Pts',(3.85182425886221,0.803946540361708,-36.0547977824671));
#17462=CARTESIAN_POINT('Ctrl Pts',(3.8745336789633,0.686149785033932,-36.060869103862));
#17463=CARTESIAN_POINT('Ctrl Pts',(3.8918095410351,0.567721319229954,-36.0669404252569));
#17464=CARTESIAN_POINT('Ctrl Pts',(3.90908540310689,0.449292853425975,-36.0730117466518));
#17465=CARTESIAN_POINT('Ctrl Pts',(3.92092772396887,0.330233159728559,-36.0790830680467));
#17466=CARTESIAN_POINT('Ctrl Pts',(3.92733184454616,0.21107719633736,-36.0851543894417));
#17467=CARTESIAN_POINT('Ctrl Pts',(3.93108772010556,0.141194850235918,-36.0887150856161));
#17468=CARTESIAN_POINT('Ctrl Pts',(3.9329785201217,0.0712113825834814,-36.0922757817906));
#17469=CARTESIAN_POINT('Ctrl Pts',(3.93299981803583,0.0011963820870183,
-36.095836477965));
#17470=CARTESIAN_POINT('',(3.93299985616677,0.0010636691862063,-37.3458364779175));
#17471=CARTESIAN_POINT('Ctrl Pts',(3.93299981803602,0.00119638148616424,
-36.0958364779956));
#17472=CARTESIAN_POINT('Ctrl Pts',(3.93303472923432,-0.113571138876911,
-36.1016731168274));
#17473=CARTESIAN_POINT('Ctrl Pts',(3.92804190460838,-0.228532354691529,
-36.1075097556592));
#17474=CARTESIAN_POINT('Ctrl Pts',(3.91799665328228,-0.343207262261184,
-36.113346394491));
#17475=CARTESIAN_POINT('Ctrl Pts',(3.90796365309392,-0.457742312893272,
-36.1191759149876));
#17476=CARTESIAN_POINT('Ctrl Pts',(3.89289051400948,-0.571991335969501,
-36.1250054354842));
#17477=CARTESIAN_POINT('Ctrl Pts',(3.87280455357822,-0.685473478541502,
-36.1308349559808));
#17478=CARTESIAN_POINT('Ctrl Pts',(3.85273755558346,-0.798848486683462,
-36.1366589730357));
#17479=CARTESIAN_POINT('Ctrl Pts',(3.82766722039873,-0.91145764399696,-36.1424829900906));
#17480=CARTESIAN_POINT('Ctrl Pts',(3.7976726789898,-1.02282511860751,-36.1483070071455));
#17481=CARTESIAN_POINT('Ctrl Pts',(3.76769688722855,-1.13412297718745,-36.1541273835957));
#17482=CARTESIAN_POINT('Ctrl Pts',(3.73280311890834,-1.24418029337354,-36.159947760046));
#17483=CARTESIAN_POINT('Ctrl Pts',(3.69312146758863,-1.35253200540173,-36.1657681364962));
#17484=CARTESIAN_POINT('Ctrl Pts',(3.65345227475206,-1.46084969923931,-36.1715866855763));
#17485=CARTESIAN_POINT('Ctrl Pts',(3.60899833068204,-1.56746246052562,-36.1774052346565));
#17486=CARTESIAN_POINT('Ctrl Pts',(3.55993919554999,-1.67192162614964,-36.1832237837367));
#17487=CARTESIAN_POINT('Ctrl Pts',(3.5108832290179,-1.77637404503209,-36.1890419570121));
#17488=CARTESIAN_POINT('Ctrl Pts',(3.45722284116619,-1.87867276600166,-36.1948601302875));
#17489=CARTESIAN_POINT('Ctrl Pts',(3.39918489340035,-1.97839102820419,-36.200678303563));
#17490=CARTESIAN_POINT('Ctrl Pts',(3.34113622069995,-2.07812771751998,-36.2064975519889));
#17491=CARTESIAN_POINT('Ctrl Pts',(3.27870859125413,-2.17528263869596,-36.2123168004148));
#17492=CARTESIAN_POINT('Ctrl Pts',(3.2121733758323,-2.26945614709651,-36.2181360488407));
#17493=CARTESIAN_POINT('Ctrl Pts',(3.14557087454878,-2.36372489146527,-36.2239611821675));
#17494=CARTESIAN_POINT('Ctrl Pts',(3.07485273583628,-2.45500586105009,-36.2297863154942));
#17495=CARTESIAN_POINT('Ctrl Pts',(3.00033201241088,-2.54293075314734,-36.235611448821));
#17496=CARTESIAN_POINT('Ctrl Pts',(2.92576983950635,-2.63090455031169,-36.2414398221692));
#17497=CARTESIAN_POINT('Ctrl Pts',(2.84740115471939,-2.71551824625154,-36.2472681955174));
#17498=CARTESIAN_POINT('Ctrl Pts',(2.76557616733952,-2.79644014108003,-36.2530965688656));
#17499=CARTESIAN_POINT('Ctrl Pts',(2.68362851809338,-2.8774833439705,-36.2589336793878));
#17500=CARTESIAN_POINT('Ctrl Pts',(2.59821453075075,-2.95482341483499,-36.26477078991));
#17501=CARTESIAN_POINT('Ctrl Pts',(2.50971793012842,-3.02816857377391,-36.2706079004322));
#17502=CARTESIAN_POINT('Ctrl Pts',(2.45852747378525,-3.07059474755056,-36.2739843504795));
#17503=CARTESIAN_POINT('Ctrl Pts',(2.40630614479675,-3.11168501738728,-36.2773608005268));
#17504=CARTESIAN_POINT('Ctrl Pts',(2.3531323840611,-3.15138969076865,-36.280737250574));
#17505=CARTESIAN_POINT('Ctrl Pts',(2.26045884695663,-3.22058871808819,-36.2866218742006));
#17506=CARTESIAN_POINT('Ctrl Pts',(2.16458299500471,-3.28580638831883,-36.2925064978272));
#17507=CARTESIAN_POINT('Ctrl Pts',(2.06588109249667,-3.34673337923187,-36.2983911214538));
#17508=CARTESIAN_POINT('Ctrl Pts',(1.96730286215315,-3.40758402943968,-36.3042683717257));
#17509=CARTESIAN_POINT('Ctrl Pts',(1.86590597102965,-3.46415447885765,-36.3101456219975));
#17510=CARTESIAN_POINT('Ctrl Pts',(1.76209829182777,-3.51617670345756,-36.3160228722693));
#17511=CARTESIAN_POINT('Ctrl Pts',(1.65839326975319,-3.56814748242093,-36.3218943104314));
#17512=CARTESIAN_POINT('Ctrl Pts',(1.55228256797723,-3.61557880094452,-36.3277657485934));
#17513=CARTESIAN_POINT('Ctrl Pts',(1.44420091878299,-3.65824721775147,-36.3336371867555));
#17514=CARTESIAN_POINT('Ctrl Pts',(1.33476289713381,-3.70145110256511,-36.3395823086284));
#17515=CARTESIAN_POINT('Ctrl Pts',(1.22330448215648,-3.73977149249103,-36.3455274305014));
#17516=CARTESIAN_POINT('Ctrl Pts',(1.1103007451359,-3.773025477697,-36.3514725523743));
#17517=CARTESIAN_POINT('Ctrl Pts',(0.998818210562108,-3.80583181360398,
-36.3573376438502));
#17518=CARTESIAN_POINT('Ctrl Pts',(0.885832111814612,-3.83370719955568,
-36.3632027353262));
#17519=CARTESIAN_POINT('Ctrl Pts',(0.771815692665296,-3.85652557836138,
-36.3690678268021));
#17520=CARTESIAN_POINT('Ctrl Pts',(0.657814512314632,-3.87934090738985,
-36.3749321343826));
#17521=CARTESIAN_POINT('Ctrl Pts',(0.542783688610737,-3.89710049282084,
-36.3807964419631));
#17522=CARTESIAN_POINT('Ctrl Pts',(0.427207315885236,-3.90972926290992,
-36.3866607495436));
#17523=CARTESIAN_POINT('Ctrl Pts',(0.311618753792879,-3.92235936490367,
-36.3925256756086));
#17524=CARTESIAN_POINT('Ctrl Pts',(0.195484937133343,-3.92985753116021,
-36.3983906016736));
#17525=CARTESIAN_POINT('Ctrl Pts',(0.0792950664487206,-3.93220056615083,
-36.4042555277387));
#17526=CARTESIAN_POINT('Ctrl Pts',(-0.0396773724094786,-3.93459971321521,
-36.410260909736));
#17527=CARTESIAN_POINT('Ctrl Pts',(-0.158708130861955,-3.93159365437423,
-36.4162662917333));
#17528=CARTESIAN_POINT('Ctrl Pts',(-0.277273370872376,-3.92321404945041,
-36.4222716737306));
#17529=CARTESIAN_POINT('Ctrl Pts',(-0.393234829030164,-3.91501846695366,
-36.4281451730221));
#17530=CARTESIAN_POINT('Ctrl Pts',(-0.508750597896959,-3.9016830282927,
-36.4340186723136));
#17531=CARTESIAN_POINT('Ctrl Pts',(-0.623338153738285,-3.88328965518852,
-36.4398921716052));
#17532=CARTESIAN_POINT('Ctrl Pts',(-0.741785108251943,-3.86427677886501,
-36.4459634949554));
#17533=CARTESIAN_POINT('Ctrl Pts',(-0.859239746550688,-3.83985934955294,
-36.4520348183055));
#17534=CARTESIAN_POINT('Ctrl Pts',(-0.975184380020213,-3.81018430328043,
-36.4581061416557));
#17535=CARTESIAN_POINT('Ctrl Pts',(-1.09112901348974,-3.78050925700792,
-36.4641774650059));
#17536=CARTESIAN_POINT('Ctrl Pts',(-1.20556320326289,-3.74557679518464,
-36.4702487883561));
#17537=CARTESIAN_POINT('Ctrl Pts',(-1.31799147545504,-3.70558868071294,
-36.4763201117063));
#17538=CARTESIAN_POINT('Ctrl Pts',(-1.42696256365722,-3.66683020596125,
-36.482204741074));
#17539=CARTESIAN_POINT('Ctrl Pts',(-1.53439575626693,-3.62319925666182,
-36.4880893704416));
#17540=CARTESIAN_POINT('Ctrl Pts',(-1.63982501144332,-3.57483746929073,
-36.4939739998093));
#17541=CARTESIAN_POINT('Ctrl Pts',(-1.74512216599344,-3.52653627821605,
-36.4998512558609));
#17542=CARTESIAN_POINT('Ctrl Pts',(-1.84842000639157,-3.47351620867746,
-36.5057285119124));
#17543=CARTESIAN_POINT('Ctrl Pts',(-1.94926933526407,-3.41596809976311,
-36.511605767964));
#17544=CARTESIAN_POINT('Ctrl Pts',(-2.05001893320035,-3.35847690076421,
-36.5174772119367));
#17545=CARTESIAN_POINT('Ctrl Pts',(-2.14832448123292,-3.2964667729808,-36.5233486559095));
#17546=CARTESIAN_POINT('Ctrl Pts',(-2.24375899286168,-3.23017562710642,
-36.5292200998822));
#17547=CARTESIAN_POINT('Ctrl Pts',(-2.34039103063641,-3.16305265028245,
-36.5351652195887));
#17548=CARTESIAN_POINT('Ctrl Pts',(-2.43407909406102,-3.09154065538387,
-36.5411103392953));
#17549=CARTESIAN_POINT('Ctrl Pts',(-2.52440756402997,-3.01593359520204,
-36.5470554590018));
#17550=CARTESIAN_POINT('Ctrl Pts',(-2.6135201965227,-2.94134421966899,-36.5529205563262));
#17551=CARTESIAN_POINT('Ctrl Pts',(-2.6993628030752,-2.86276962126291,-36.5587856536506));
#17552=CARTESIAN_POINT('Ctrl Pts',(-2.78156809028633,-2.7805337543538,-36.564650750975));
#17553=CARTESIAN_POINT('Ctrl Pts',(-2.86376239045725,-2.698308878572,-36.5705150644075));
#17554=CARTESIAN_POINT('Ctrl Pts',(-2.94232004745701,-2.61242399830032,
-36.57637937784));
#17555=CARTESIAN_POINT('Ctrl Pts',(-3.01691018322573,-2.52324036634421,
-36.5822436912725));
#17556=CARTESIAN_POINT('Ctrl Pts',(-3.09150818566194,-2.43404732861386,
-36.5881086231863));
#17557=CARTESIAN_POINT('Ctrl Pts',(-3.16213757119426,-2.34155516306203,
-36.5939735551));
#17558=CARTESIAN_POINT('Ctrl Pts',(-3.22850780330919,-2.2461581342309,-36.5998384870138));
#17559=CARTESIAN_POINT('Ctrl Pts',(-3.29646733977885,-2.14847672415659,
-36.6058438608326));
#17560=CARTESIAN_POINT('Ctrl Pts',(-3.35996088153859,-2.04774992820193,
-36.6118492346513));
#17561=CARTESIAN_POINT('Ctrl Pts',(-3.41872434138119,-1.94443124785829,
-36.6178546084701));
#17562=CARTESIAN_POINT('Ctrl Pts',(-3.47619744633893,-1.84338128627688,
-36.6237281135482));
#17563=CARTESIAN_POINT('Ctrl Pts',(-3.52914592394074,-1.7398524930139,-36.6296016186264));
#17564=CARTESIAN_POINT('Ctrl Pts',(-3.57737042052471,-1.63429185715246,
-36.6354751237045));
#17565=CARTESIAN_POINT('Ctrl Pts',(-3.62721898235056,-1.52517623634027,
-36.6415464318935));
#17566=CARTESIAN_POINT('Ctrl Pts',(-3.67201959214682,-1.41388995690449,
-36.6476177400826));
#17567=CARTESIAN_POINT('Ctrl Pts',(-3.7116075074509,-1.30094531423658,-36.6536890482716));
#17568=CARTESIAN_POINT('Ctrl Pts',(-3.75119542275497,-1.18800067156868,
-36.6597603564607));
#17569=CARTESIAN_POINT('Ctrl Pts',(-3.78557056786004,-1.07339814256441,
-36.6658316646497));
#17570=CARTESIAN_POINT('Ctrl Pts',(-3.81462614444298,-0.957661933112155,
-36.6719029728387));
#17571=CARTESIAN_POINT('Ctrl Pts',(-3.84278823538565,-0.845484718295886,
-36.6777875827302));
#17572=CARTESIAN_POINT('Ctrl Pts',(-3.8660426999347,-0.731885884848342,
-36.6836721926216));
#17573=CARTESIAN_POINT('Ctrl Pts',(-3.88424901836939,-0.617331809723478,
-36.689556802513));
#17574=CARTESIAN_POINT('Ctrl Pts',(-3.90243252452278,-0.502921269371648,
-36.6954340390644));
#17575=CARTESIAN_POINT('Ctrl Pts',(-3.9155804009619,-0.387558270641264,
-36.7013112756158));
#17576=CARTESIAN_POINT('Ctrl Pts',(-3.92360241474224,-0.271722452198623,
-36.7071885121672));
#17577=CARTESIAN_POINT('Ctrl Pts',(-3.93161649544519,-0.156001185355937,
-36.7130599366403));
#17578=CARTESIAN_POINT('Ctrl Pts',(-3.9345147692093,-0.03980843702116,-36.7189313611134));
#17579=CARTESIAN_POINT('Ctrl Pts',(-3.93225849176958,0.0763685400279876,
-36.7248027855864));
#17580=CARTESIAN_POINT('Ctrl Pts',(-3.92997389183578,0.194003858009621,
-36.7307479126025));
#17581=CARTESIAN_POINT('Ctrl Pts',(-3.92240437347689,0.31162258351543,-36.7366930396185));
#17582=CARTESIAN_POINT('Ctrl Pts',(-3.90956413481056,0.428715845057024,
-36.7426381666345));
#17583=CARTESIAN_POINT('Ctrl Pts',(-3.8968967854855,0.544232486616664,-36.748503244586));
#17584=CARTESIAN_POINT('Ctrl Pts',(-3.87909983611869,0.659237307992045,
-36.7543683225375));
#17585=CARTESIAN_POINT('Ctrl Pts',(-3.85623924651464,0.773245028202716,
-36.760233400489));
#17586=CARTESIAN_POINT('Ctrl Pts',(-3.83338171200276,0.887237512406752,
-36.7660976946308));
#17587=CARTESIAN_POINT('Ctrl Pts',(-3.80546196394673,1.0002327573192,-36.7719619887725));
#17588=CARTESIAN_POINT('Ctrl Pts',(-3.77259719291646,1.11175510792567,-36.7778262829142));
#17589=CARTESIAN_POINT('Ctrl Pts',(-3.73972895520139,1.22328922227873,-36.7836911956411));
#17590=CARTESIAN_POINT('Ctrl Pts',(-3.70191477382609,1.33334973897271,-36.7895561083679));
#17591=CARTESIAN_POINT('Ctrl Pts',(-3.65932167946615,1.4414762731967,-36.7954210210948));
#17592=CARTESIAN_POINT('Ctrl Pts',(-3.61570830847756,1.55219287460091,-36.8014264221678));
#17593=CARTESIAN_POINT('Ctrl Pts',(-3.56708432021527,1.66088123559898,-36.8074318232409));
#17594=CARTESIAN_POINT('Ctrl Pts',(-3.51368071381787,1.76707012915287,-36.8134372243139));
#17595=CARTESIAN_POINT('Ctrl Pts',(-3.46145017200904,1.8709264755413,-36.8193107106378));
#17596=CARTESIAN_POINT('Ctrl Pts',(-3.40464808210247,1.9723916958076,-36.8251841969617));
#17597=CARTESIAN_POINT('Ctrl Pts',(-3.34353590907388,2.07105205746585,-36.8310576832857));
#17598=CARTESIAN_POINT('Ctrl Pts',(-3.28036492552098,2.17303619212785,-36.8371290417332));
#17599=CARTESIAN_POINT('Ctrl Pts',(-3.21258860658891,2.27202274920149,-36.8432004001808));
#17600=CARTESIAN_POINT('Ctrl Pts',(-3.14054196812054,2.36759057830394,-36.8492717586284));
#17601=CARTESIAN_POINT('Ctrl Pts',(-3.06849532965217,2.46315840740639,-36.855343117076));
#17602=CARTESIAN_POINT('Ctrl Pts',(-2.99217872658223,2.55530718110447,-36.8614144755235));
#17603=CARTESIAN_POINT('Ctrl Pts',(-2.91196921511862,2.64365737004655,-36.8674858339711));
#17604=CARTESIAN_POINT('Ctrl Pts',(-2.83422659571384,2.72929029546813,-36.8733704641159));
#17605=CARTESIAN_POINT('Ctrl Pts',(-2.75257986797348,2.81162715474329,-36.8792550942608));
#17606=CARTESIAN_POINT('Ctrl Pts',(-2.6673392546602,2.8902924247468,-36.8851397244056));
#17607=CARTESIAN_POINT('Ctrl Pts',(-2.58220544780444,2.96885912719558,-36.891016981111));
#17608=CARTESIAN_POINT('Ctrl Pts',(-2.49348701142665,3.04376311380706,-36.8968942378163));
#17609=CARTESIAN_POINT('Ctrl Pts',(-2.40153308591305,3.11466335857745,-36.9027714945217));
#17610=CARTESIAN_POINT('Ctrl Pts',(-2.30967009648456,3.18549348789973,-36.9086429390259));
#17611=CARTESIAN_POINT('Ctrl Pts',(-2.2145783070513,3.25232750222358,-36.9145143835301));
#17612=CARTESIAN_POINT('Ctrl Pts',(-2.11664174195745,3.31486300413808,-36.9203858280343));
#17613=CARTESIAN_POINT('Ctrl Pts',(-2.01747626765401,3.37818320229096,-36.9263309474955));
#17614=CARTESIAN_POINT('Ctrl Pts',(-1.91539444734215,3.43709597863483,-36.9322760669567));
#17615=CARTESIAN_POINT('Ctrl Pts',(-1.81082764429584,3.4913310130456,-36.938221186418));
#17616=CARTESIAN_POINT('Ctrl Pts',(-1.70766832093664,3.54483603843782,-36.9440862839732));
#17617=CARTESIAN_POINT('Ctrl Pts',(-1.60209088022816,3.59378828775386,-36.9499513815285));
#17618=CARTESIAN_POINT('Ctrl Pts',(-1.49453575747148,3.63797359386227,-36.9558164790838));
#17619=CARTESIAN_POINT('Ctrl Pts',(-1.38699501191209,3.6821529935959,-36.9616807926349));
#17620=CARTESIAN_POINT('Ctrl Pts',(-1.27747749040105,3.72156656118633,-36.9675451061859));
#17621=CARTESIAN_POINT('Ctrl Pts',(-1.16644402171783,3.75604810195486,-36.973409419737));
#17622=CARTESIAN_POINT('Ctrl Pts',(-1.05539884497981,3.79053327867005,-36.9792743516576));
#17623=CARTESIAN_POINT('Ctrl Pts',(-0.942837796059542,3.82008527273901,
-36.9851392835781));
#17624=CARTESIAN_POINT('Ctrl Pts',(-0.829236628951203,3.84458783398242,
-36.9910042154987));
#17625=CARTESIAN_POINT('Ctrl Pts',(-0.712915173716917,3.86967713238798,
-36.9970095887991));
#17626=CARTESIAN_POINT('Ctrl Pts',(-0.595503594897514,3.88947198999402,
-37.0030149620995));
#17627=CARTESIAN_POINT('Ctrl Pts',(-0.477522124356276,3.90390338260955,
-37.0090203353999));
#17628=CARTESIAN_POINT('Ctrl Pts',(-0.362131340119266,3.91801788469109,
-37.0148938402103));
#17629=CARTESIAN_POINT('Ctrl Pts',(-0.246195853650308,3.92700206931307,
-37.0207673450208));
#17630=CARTESIAN_POINT('Ctrl Pts',(-0.130204952198965,3.93084414221969,
-37.0266408498313));
#17631=CARTESIAN_POINT('Ctrl Pts',(-0.0103078110709597,3.93481560508226,
-37.0327121573767));
#17632=CARTESIAN_POINT('Ctrl Pts',(0.109648058222881,3.93329251379023,-37.038783464922));
#17633=CARTESIAN_POINT('Ctrl Pts',(0.229126433390375,3.92632017002203,-37.0448547724674));
#17634=CARTESIAN_POINT('Ctrl Pts',(0.34860480855787,3.91934782625383,-37.0509260800128));
#17635=CARTESIAN_POINT('Ctrl Pts',(0.467605220340459,3.90692634384008,-37.0569973875581));
#17636=CARTESIAN_POINT('Ctrl Pts',(0.58560277456768,3.88915908525463,-37.0630686951035));
#17637=CARTESIAN_POINT('Ctrl Pts',(0.699972824622961,3.87193803124999,-37.0689533573104));
#17638=CARTESIAN_POINT('Ctrl Pts',(0.813764377535811,3.84964035700378,-37.0748380195173));
#17639=CARTESIAN_POINT('Ctrl Pts',(0.926492909708655,3.82231603720304,-37.0807226817242));
#17640=CARTESIAN_POINT('Ctrl Pts',(1.0390801998307,3.79502595312676,-37.0865999708043));
#17641=CARTESIAN_POINT('Ctrl Pts',(1.15060672192642,3.76272184592289,-37.0924772598844));
#17642=CARTESIAN_POINT('Ctrl Pts',(1.26059508478111,3.72550520496559,-37.0983545489645));
#17643=CARTESIAN_POINT('Ctrl Pts',(1.37047468235874,3.68832536679506,-37.1042260261118));
#17644=CARTESIAN_POINT('Ctrl Pts',(1.47881875913099,3.64624278994846,-37.1100975032591));
#17645=CARTESIAN_POINT('Ctrl Pts',(1.58516273091977,3.59940941218181,-37.1159689804064));
#17646=CARTESIAN_POINT('Ctrl Pts',(1.69284028972156,3.55198872905769,-37.1219140877326));
#17647=CARTESIAN_POINT('Ctrl Pts',(1.79846681826055,3.49969737174488,-37.1278591950588));
#17648=CARTESIAN_POINT('Ctrl Pts',(1.90157819206338,3.44274445456949,-37.1338043023851));
#17649=CARTESIAN_POINT('Ctrl Pts',(2.00330245784964,3.38655769776096,-37.1396694330246));
#17650=CARTESIAN_POINT('Ctrl Pts',(2.10257845799757,3.3258342435757,-37.1455345636642));
#17651=CARTESIAN_POINT('Ctrl Pts',(2.19898375965077,3.2608218940617,-37.1513996943038));
#17652=CARTESIAN_POINT('Ctrl Pts',(2.29537617632454,3.1958182337253,-37.1572640410437));
#17653=CARTESIAN_POINT('Ctrl Pts',(2.38889831669172,3.1265270480034,-37.1631283877836));
#17654=CARTESIAN_POINT('Ctrl Pts',(2.47915636493696,3.0532397086034,-37.1689927345235));
#17655=CARTESIAN_POINT('Ctrl Pts',(2.56942393150794,2.97994464055445,-37.1748576996986));
#17656=CARTESIAN_POINT('Ctrl Pts',(2.65642640240147,2.90265284030614,-37.1807226648738));
#17657=CARTESIAN_POINT('Ctrl Pts',(2.73980325177983,2.82169579181326,-37.186587630049));
#17658=CARTESIAN_POINT('Ctrl Pts',(2.82517549952317,2.73880125631528,-37.1925929572312));
#17659=CARTESIAN_POINT('Ctrl Pts',(2.90674604863093,2.65206411590826,-37.1985982844134));
#17660=CARTESIAN_POINT('Ctrl Pts',(2.98416902896958,2.56187903823322,-37.2046036115957));
#17661=CARTESIAN_POINT('Ctrl Pts',(3.05989293159331,2.47367310751204,-37.210477149514));
#17662=CARTESIAN_POINT('Ctrl Pts',(3.13164922179133,2.38216937861496,-37.2163506874324));
#17663=CARTESIAN_POINT('Ctrl Pts',(3.1991568005265,2.28776851225054,-37.2222242253508));
#17664=CARTESIAN_POINT('Ctrl Pts',(3.2689364614968,2.19019042437312,-37.2282954471649));
#17665=CARTESIAN_POINT('Ctrl Pts',(3.33417611327404,2.08951715404321,-37.2343666689791));
#17666=CARTESIAN_POINT('Ctrl Pts',(3.39461616518399,1.98622005101941,-37.2404378907933));
#17667=CARTESIAN_POINT('Ctrl Pts',(3.45505621709394,1.88292294799562,-37.2465091126075));
#17668=CARTESIAN_POINT('Ctrl Pts',(3.51069650370839,1.77700246586642,-37.2525803344216));
#17669=CARTESIAN_POINT('Ctrl Pts',(3.56133203022404,1.66895271667604,-37.2586515562358));
#17670=CARTESIAN_POINT('Ctrl Pts',(3.61423885573669,1.55605630539188,-37.2649951077949));
#17671=CARTESIAN_POINT('Ctrl Pts',(3.66183034001354,1.44052089285038,-37.2713386593539));
#17672=CARTESIAN_POINT('Ctrl Pts',(3.70385729676319,1.32284924508202,-37.2776822109129));
#17673=CARTESIAN_POINT('Ctrl Pts',(3.74575017190444,1.20555301359443,-37.2840055241854));
#17674=CARTESIAN_POINT('Ctrl Pts',(3.78211381721462,1.0861344272398,-37.2903288374578));
#17675=CARTESIAN_POINT('Ctrl Pts',(3.81274711943031,0.965115746051162,-37.2966521507302));
#17676=CARTESIAN_POINT('Ctrl Pts',(3.84331913759382,0.844339171153237,-37.3029628137746));
#17677=CARTESIAN_POINT('Ctrl Pts',(3.86818358034013,0.721969177049568,-37.3092734768189));
#17678=CARTESIAN_POINT('Ctrl Pts',(3.88718829857242,0.598545012043067,-37.3155841398632));
#17679=CARTESIAN_POINT('Ctrl Pts',(3.90613595983782,0.475491397570901,-37.3218758567023));
#17680=CARTESIAN_POINT('Ctrl Pts',(3.91925892408688,0.351390225876226,-37.3281675735414));
#17681=CARTESIAN_POINT('Ctrl Pts',(3.9264557247084,0.226791626619253,-37.3344592903805));
#17682=CARTESIAN_POINT('Ctrl Pts',(3.9307936689416,0.151688562975241,-37.3382516862262));
#17683=CARTESIAN_POINT('Ctrl Pts',(3.93297948029164,0.0764050582108798,
-37.3420440820718));
#17684=CARTESIAN_POINT('Ctrl Pts',(3.93299985616677,0.00106366918621726,
-37.3458364779175));
#17685=CARTESIAN_POINT('Ctrl Pts',(3.93299985616703,0.00106366824158364,
-37.345836477965));
#17686=CARTESIAN_POINT('Ctrl Pts',(3.9330321879552,-0.118485748811121,-37.3518541359674));
#17687=CARTESIAN_POINT('Ctrl Pts',(3.92760934873402,-0.237986703531313,
-37.3578717939699));
#17688=CARTESIAN_POINT('Ctrl Pts',(3.91677077722735,-0.356925312436485,
-37.3638894519723));
#17689=CARTESIAN_POINT('Ctrl Pts',(3.9059248975669,-0.475944118408449,-37.3699111675177));
#17690=CARTESIAN_POINT('Ctrl Pts',(3.8896560441002,-0.594399445105386,-37.3759328830631));
#17691=CARTESIAN_POINT('Ctrl Pts',(3.86805530385929,-0.711784494271979,
-37.3819545986086));
#17692=CARTESIAN_POINT('Ctrl Pts',(3.84641826160541,-0.829366819713841,
-37.3879864341959));
#17693=CARTESIAN_POINT('Ctrl Pts',(3.81943149570112,-0.945874899042958,
-37.3940182697832));
#17694=CARTESIAN_POINT('Ctrl Pts',(3.78723705854409,-1.06081311379069,-37.4000501053705));
#17695=CARTESIAN_POINT('Ctrl Pts',(3.75501541025168,-1.17584847573518,-37.4060870391396));
#17696=CARTESIAN_POINT('Ctrl Pts',(3.71757743273379,-1.28931096675788,-37.4121239729087));
#17697=CARTESIAN_POINT('Ctrl Pts',(3.67511420835027,-1.40072286894374,-37.4181609066779));
#17698=CARTESIAN_POINT('Ctrl Pts',(3.63256382233341,-1.51236345944775,-37.4242102320874));
#17699=CARTESIAN_POINT('Ctrl Pts',(3.58496771857707,-1.62194469683356,-37.430259557497));
#17700=CARTESIAN_POINT('Ctrl Pts',(3.53256454584281,-1.72901033237352,-37.4363088829065));
#17701=CARTESIAN_POINT('Ctrl Pts',(3.48080368463642,-1.83476365248756,-37.4422840610604));
#17702=CARTESIAN_POINT('Ctrl Pts',(3.42435318210951,-1.93806242851611,-37.4482592392143));
#17703=CARTESIAN_POINT('Ctrl Pts',(3.36348441947456,-2.03849492517198,-37.4542344173682));
#17704=CARTESIAN_POINT('Ctrl Pts',(3.30353718729878,-2.13740691112987,-37.4601191335441));
#17705=CARTESIAN_POINT('Ctrl Pts',(3.23912784186652,-2.23382952484871,-37.46600384972));
#17706=CARTESIAN_POINT('Ctrl Pts',(3.17048913890051,-2.32733487494041,-37.4718885658958));
#17707=CARTESIAN_POINT('Ctrl Pts',(3.10193644549645,-2.42072305565313,-37.4777659080708));
#17708=CARTESIAN_POINT('Ctrl Pts',(3.02916517655114,-2.51120091460067,-37.4836432502457));
#17709=CARTESIAN_POINT('Ctrl Pts',(2.952452880109,-2.59836698538449,-37.4895205924206));
#17710=CARTESIAN_POINT('Ctrl Pts',(2.8758164543284,-2.6854468464241,-37.4953921217355));
#17711=CARTESIAN_POINT('Ctrl Pts',(2.79524702526215,-2.76922112821716,-37.5012636510505));
#17712=CARTESIAN_POINT('Ctrl Pts',(2.71106376348625,-2.84931961533131,-37.5071351803654));
#17713=CARTESIAN_POINT('Ctrl Pts',(2.62582585971236,-2.93042157067305,-37.5130802677877));
#17714=CARTESIAN_POINT('Ctrl Pts',(2.53688320539153,-3.00775465232699,-37.51902535521));
#17715=CARTESIAN_POINT('Ctrl Pts',(2.44460754525337,-3.0809711049749,-37.5249704426323));
#17716=CARTESIAN_POINT('Ctrl Pts',(2.35357215113052,-3.15320346411599,-37.5308356228518));
#17717=CARTESIAN_POINT('Ctrl Pts',(2.25929313613745,-3.22142892218565,-37.5367008030713));
#17718=CARTESIAN_POINT('Ctrl Pts',(2.16216190151178,-3.28535308782039,-37.5425659832908));
#17719=CARTESIAN_POINT('Ctrl Pts',(2.06504366620733,-3.34926869832077,-37.5484303785583));
#17720=CARTESIAN_POINT('Ctrl Pts',(1.96507431389771,-3.40888393523525,-37.5542947738257));
#17721=CARTESIAN_POINT('Ctrl Pts',(1.86267443087605,-3.46394759841436,-37.5601591690932));
#17722=CARTESIAN_POINT('Ctrl Pts',(1.76026376843625,-3.5190170580283,-37.5660241816931));
#17723=CARTESIAN_POINT('Ctrl Pts',(1.6554224288657,-3.56953379664985,-37.571889194293));
#17724=CARTESIAN_POINT('Ctrl Pts',(1.54859519303285,-3.61529278594633,-37.5777542068928));
#17725=CARTESIAN_POINT('Ctrl Pts',(1.43921351916066,-3.66214595784511,-37.5837594628602));
#17726=CARTESIAN_POINT('Ctrl Pts',(1.3277501828572,-3.7040107694697,-37.5897647188275));
#17727=CARTESIAN_POINT('Ctrl Pts',(1.21470259933593,-3.74072006372657,-37.5957699747948));
#17728=CARTESIAN_POINT('Ctrl Pts',(1.10413374470272,-3.77662445454986,-37.6016435569927));
#17729=CARTESIAN_POINT('Ctrl Pts',(0.992049819009357,-3.80759703358294,
-37.6075171391906));
#17730=CARTESIAN_POINT('Ctrl Pts',(0.878928848537685,-3.83353271529124,
-37.6133907213885));
#17731=CARTESIAN_POINT('Ctrl Pts',(0.762003964862561,-3.86034053486822,
-37.6194618142405));
#17732=CARTESIAN_POINT('Ctrl Pts',(0.643971540502412,-3.88176665637471,
-37.6255329070925));
#17733=CARTESIAN_POINT('Ctrl Pts',(0.525366507130672,-3.89775307493757,
-37.6316039999445));
#17734=CARTESIAN_POINT('Ctrl Pts',(0.406761473758932,-3.91373949350043,
-37.6376750927966));
#17735=CARTESIAN_POINT('Ctrl Pts',(0.287584313608817,-3.92428623115194,
-37.6437461856486));
#17736=CARTESIAN_POINT('Ctrl Pts',(0.168369936222375,-3.92939442720841,
-37.6498172785006));
#17737=CARTESIAN_POINT('Ctrl Pts',(0.052812542204191,-3.93434592582258,
-37.6557021363861));
#17738=CARTESIAN_POINT('Ctrl Pts',(-0.0631470300060075,-3.93420344049839,
-37.6615869942715));
#17739=CARTESIAN_POINT('Ctrl Pts',(-0.17902360411251,-3.92892345931689,
-37.667471852157));
#17740=CARTESIAN_POINT('Ctrl Pts',(-0.294755027470508,-3.92365009201076,
-37.6733493384789));
#17741=CARTESIAN_POINT('Ctrl Pts',(-0.410403252154865,-3.91325204689014,
-37.6792268248008));
#17742=CARTESIAN_POINT('Ctrl Pts',(-0.525480261887363,-3.89773774058322,
-37.6851043111228));
#17743=CARTESIAN_POINT('Ctrl Pts',(-0.640443503513937,-3.88223877212047,
-37.6909759868098));
#17744=CARTESIAN_POINT('Ctrl Pts',(-0.754836248274933,-3.86163365930045,
-37.6968476624969));
#17745=CARTESIAN_POINT('Ctrl Pts',(-0.868173413332504,-3.83598278468277,
-37.7027193381839));
#17746=CARTESIAN_POINT('Ctrl Pts',(-0.982926554842207,-3.81001144118433,
-37.7086643715776));
#17747=CARTESIAN_POINT('Ctrl Pts',(-1.09659713254844,-3.7788674114688,-37.7146094049713));
#17748=CARTESIAN_POINT('Ctrl Pts',(-1.20868965893546,-3.74266727193087,
-37.7205544383651));
#17749=CARTESIAN_POINT('Ctrl Pts',(-1.31927941210295,-3.70695245110235,
-37.7264197694159));
#17750=CARTESIAN_POINT('Ctrl Pts',(-1.42833276785933,-3.66631640021433,
-37.7322851004667));
#17751=CARTESIAN_POINT('Ctrl Pts',(-1.53538770225576,-3.6209216511493,-37.7381504315175));
#17752=CARTESIAN_POINT('Ctrl Pts',(-1.64242833489751,-3.57553296649007,
-37.7440149790031));
#17753=CARTESIAN_POINT('Ctrl Pts',(-1.74747069864278,-3.5253870085123,-37.7498795264887));
#17754=CARTESIAN_POINT('Ctrl Pts',(-1.85007253448565,-3.47069454391219,
-37.7557440739742));
#17755=CARTESIAN_POINT('Ctrl Pts',(-1.95268519180486,-3.41599631086548,
-37.7616092399971));
#17756=CARTESIAN_POINT('Ctrl Pts',(-2.0528564466283,-3.35675081137584,-37.76747440602));
#17757=CARTESIAN_POINT('Ctrl Pts',(-2.15016905196046,-3.29321454630449,
-37.7733395720429));
#17758=CARTESIAN_POINT('Ctrl Pts',(-2.24980251426086,-3.22816297308755,
-37.779344619342));
#17759=CARTESIAN_POINT('Ctrl Pts',(-2.34643885969176,-3.15861361566418,
-37.7853496666412));
#17760=CARTESIAN_POINT('Ctrl Pts',(-2.43966325082814,-3.0848877163616,-37.7913547139404));
#17761=CARTESIAN_POINT('Ctrl Pts',(-2.53084913873483,-3.01277395399022,
-37.7972284510946));
#17762=CARTESIAN_POINT('Ctrl Pts',(-2.61877048248721,-2.93666474777405,
-37.8031021882488));
#17763=CARTESIAN_POINT('Ctrl Pts',(-2.70307477628502,-2.85689967513941,
-37.808975925403));
#17764=CARTESIAN_POINT('Ctrl Pts',(-2.79020606303856,-2.7744598241715,-37.8150466277747));
#17765=CARTESIAN_POINT('Ctrl Pts',(-2.87347312209116,-2.68811496539785,
-37.8211173301463));
#17766=CARTESIAN_POINT('Ctrl Pts',(-2.9525311689054,-2.59827802527792,-37.827188032518));
#17767=CARTESIAN_POINT('Ctrl Pts',(-3.03158921571963,-2.50844108515799,
-37.8332587348896));
#17768=CARTESIAN_POINT('Ctrl Pts',(-3.1064380013842,-2.41511247701759,-37.8393294372613));
#17769=CARTESIAN_POINT('Ctrl Pts',(-3.17678195644198,-2.31873788972033,
-37.8454001396329));
#17770=CARTESIAN_POINT('Ctrl Pts',(-3.24495953773304,-2.22533133823407,
-37.8512838833618));
#17771=CARTESIAN_POINT('Ctrl Pts',(-3.30912257044277,-2.12876658268556,
-37.8571676270907));
#17772=CARTESIAN_POINT('Ctrl Pts',(-3.36896585726649,-2.02942308367985,
-37.8630513708196));
#17773=CARTESIAN_POINT('Ctrl Pts',(-3.42873413691139,-1.93020410115695,
-37.8689277399031));
#17774=CARTESIAN_POINT('Ctrl Pts',(-3.4841932287675,-1.82821365167522,-37.8748041089867));
#17775=CARTESIAN_POINT('Ctrl Pts',(-3.53507956927122,-1.72386236078209,
-37.8806804780702));
#17776=CARTESIAN_POINT('Ctrl Pts',(-3.5859155782458,-1.61961428344266,-37.8865510348544));
#17777=CARTESIAN_POINT('Ctrl Pts',(-3.63218765399647,-1.51301037771174,
-37.8924215916386));
#17778=CARTESIAN_POINT('Ctrl Pts',(-3.67367710123949,-1.4044876488701,-37.8982921484229));
#17779=CARTESIAN_POINT('Ctrl Pts',(-3.71569586260464,-1.29458040862218,
-37.9042376006038));
#17780=CARTESIAN_POINT('Ctrl Pts',(-3.75280888822166,-1.18270540918299,
-37.9101830527847));
#17781=CARTESIAN_POINT('Ctrl Pts',(-3.78483834382535,-1.06933984827526,
-37.9161285049657));
#17782=CARTESIAN_POINT('Ctrl Pts',(-3.81643015856616,-0.957523280347951,
-37.9219927202734));
#17783=CARTESIAN_POINT('Ctrl Pts',(-3.84307635110814,-0.844257040098927,
-37.9278569355812));
#17784=CARTESIAN_POINT('Ctrl Pts',(-3.8646560300124,-0.730015595510648,
-37.933721150889));
#17785=CARTESIAN_POINT('Ctrl Pts',(-3.8862328372021,-0.615789353596278,
-37.9395845858166));
#17786=CARTESIAN_POINT('Ctrl Pts',(-3.90274439532046,-0.500588569600884,
-37.9454480207442));
#17787=CARTESIAN_POINT('Ctrl Pts',(-3.91412091324391,-0.384898007927584,
-37.9513114556719));
#17788=CARTESIAN_POINT('Ctrl Pts',(-3.92549863990729,-0.269195154285753,
-37.9571755135817));
#17789=CARTESIAN_POINT('Ctrl Pts',(-3.93174020151445,-0.15300282894872,
-37.9630395714915));
#17790=CARTESIAN_POINT('Ctrl Pts',(-3.93282773574889,-0.0368103371924791,
-37.9689036294013));
#17791=CARTESIAN_POINT('Ctrl Pts',(-3.93394170814879,0.0822068162847243,
-37.9749102436816));
#17792=CARTESIAN_POINT('Ctrl Pts',(-3.92964781478223,0.201223689949559,
-37.980916857962));
#17793=CARTESIAN_POINT('Ctrl Pts',(-3.91998347243803,0.319716399036246,
-37.9869234722423));
#17794=CARTESIAN_POINT('Ctrl Pts',(-3.9105346715888,0.435566393828449,-37.992796122454));
#17795=CARTESIAN_POINT('Ctrl Pts',(-3.89595257684535,0.550914954431655,
-37.9986687726656));
#17796=CARTESIAN_POINT('Ctrl Pts',(-3.87632438227948,0.665280604967251,
-38.0045414228772));
#17797=CARTESIAN_POINT('Ctrl Pts',(-3.85602456432968,0.783559536724963,
-38.0106150191919));
#17798=CARTESIAN_POINT('Ctrl Pts',(-3.83032724130082,0.900786613951159,
-38.0166886155066));
#17799=CARTESIAN_POINT('Ctrl Pts',(-3.79938525225186,1.01644513131356,-38.0227622118213));
#17800=CARTESIAN_POINT('Ctrl Pts',(-3.76844326320291,1.13210364867596,-38.028835808136));
#17801=CARTESIAN_POINT('Ctrl Pts',(-3.73225681506575,1.24619316832321,-38.0349094044507));
#17802=CARTESIAN_POINT('Ctrl Pts',(-3.69103343471819,1.35821985841484,-38.0409830007653));
#17803=CARTESIAN_POINT('Ctrl Pts',(-3.65108579019771,1.46677966973685,-38.0468686381026));
#17804=CARTESIAN_POINT('Ctrl Pts',(-3.60628128121676,1.57374793813777,-38.0527542754398));
#17805=CARTESIAN_POINT('Ctrl Pts',(-3.55676669598073,1.67866008183978,-38.058639912777));
#17806=CARTESIAN_POINT('Ctrl Pts',(-3.50731417562142,1.78344072167815,-38.0645181726646));
#17807=CARTESIAN_POINT('Ctrl Pts',(-3.45316349549236,1.8861699941896,-38.0703964325523));
#17808=CARTESIAN_POINT('Ctrl Pts',(-3.39451045820645,1.98640070205561,-38.0762746924399));
#17809=CARTESIAN_POINT('Ctrl Pts',(-3.33591546662906,2.08653221706269,-38.0821471349347));
#17810=CARTESIAN_POINT('Ctrl Pts',(-3.27282718839415,2.18416973356207,-38.0880195774295));
#17811=CARTESIAN_POINT('Ctrl Pts',(-3.20548825147931,2.27888877956519,-38.0938920199243));
#17812=CARTESIAN_POINT('Ctrl Pts',(-3.13732024435269,2.37477399692662,-38.0998367633398));
#17813=CARTESIAN_POINT('Ctrl Pts',(-3.06479638493153,2.46766800685349,-38.1057815067554));
#17814=CARTESIAN_POINT('Ctrl Pts',(-2.98821500532626,2.55715859538336,-38.111726250171));
#17815=CARTESIAN_POINT('Ctrl Pts',(-2.91264702878933,2.64546495300133,-38.1175923266671));
#17816=CARTESIAN_POINT('Ctrl Pts',(-2.83312855279008,2.73045710576944,-38.1234584031633));
#17817=CARTESIAN_POINT('Ctrl Pts',(-2.74998758315251,2.81177120201964,-38.1293244796594));
#17818=CARTESIAN_POINT('Ctrl Pts',(-2.66685785092488,2.8930743077818,-38.1351897632913));
#17819=CARTESIAN_POINT('Ctrl Pts',(-2.58010689268395,2.97070005836383,-38.1410550469231));
#17820=CARTESIAN_POINT('Ctrl Pts',(-2.49009961654933,3.0443214185859,-38.146920330555));
#17821=CARTESIAN_POINT('Ctrl Pts',(-2.40008300349067,3.11795041593551,-38.1527862226233));
#17822=CARTESIAN_POINT('Ctrl Pts',(-2.30680971925093,3.18757393686283,-38.1586521146916));
#17823=CARTESIAN_POINT('Ctrl Pts',(-2.21067724698488,3.2529056410636,-38.1645180067599));
#17824=CARTESIAN_POINT('Ctrl Pts',(-2.11228160719673,3.31977539570273,-38.170521994688));
#17825=CARTESIAN_POINT('Ctrl Pts',(-2.01089084058811,3.38214846478323,-38.1765259826162));
#17826=CARTESIAN_POINT('Ctrl Pts',(-1.90696084634371,3.43976588309612,-38.1825299705443));
#17827=CARTESIAN_POINT('Ctrl Pts',(-1.80527349143156,3.4961400117363,-38.1884044022306));
#17828=CARTESIAN_POINT('Ctrl Pts',(-1.70115578424155,3.54796152023605,-38.1942788339168));
#17829=CARTESIAN_POINT('Ctrl Pts',(-1.59505694251843,3.59503579260677,-38.200153265603));
#17830=CARTESIAN_POINT('Ctrl Pts',(-1.48544820368334,3.64366734731872,-38.2062220316521));
#17831=CARTESIAN_POINT('Ctrl Pts',(-1.37372543203458,3.68723195741313,-38.2122907977013));
#17832=CARTESIAN_POINT('Ctrl Pts',(-1.26040190601216,3.72557056507066,-38.2183595637504));
#17833=CARTESIAN_POINT('Ctrl Pts',(-1.14707837998975,3.76390917272819,-38.2244283297995));
#17834=CARTESIAN_POINT('Ctrl Pts',(-1.03215457570478,3.79702170740404,-38.2304970958486));
#17835=CARTESIAN_POINT('Ctrl Pts',(-0.916155051025256,3.82480704382338,
-38.2365658618977));
#17836=CARTESIAN_POINT('Ctrl Pts',(-0.803651685067322,3.85175494624009,
-38.2424517188409));
#17837=CARTESIAN_POINT('Ctrl Pts',(-0.689780227077975,3.87377753991593,
-38.248337575784));
#17838=CARTESIAN_POINT('Ctrl Pts',(-0.575008792492617,3.89073950407325,
-38.2542234327272));
#17839=CARTESIAN_POINT('Ctrl Pts',(-0.460380857323033,3.90768026058465,
-38.260101930548));
#17840=CARTESIAN_POINT('Ctrl Pts',(-0.344855586843771,3.91957291266557,
-38.2659804283687));
#17841=CARTESIAN_POINT('Ctrl Pts',(-0.228913789094253,3.9263325734281,-38.2718589261895));
#17842=CARTESIAN_POINT('Ctrl Pts',(-0.113086377458502,3.93308556522965,
-38.277731624389));
#17843=CARTESIAN_POINT('Ctrl Pts',(0.00315633580555784,3.93471561623088,
-38.2836043225884));
#17844=CARTESIAN_POINT('Ctrl Pts',(0.119326508151583,3.93118941091018,-38.2894770207879));
#17845=CARTESIAN_POINT('Ctrl Pts',(0.2369200718725,3.92762000026287,-38.295421675048));
#17846=CARTESIAN_POINT('Ctrl Pts',(0.354438882306982,3.91876706389708,-38.3013663293081));
#17847=CARTESIAN_POINT('Ctrl Pts',(0.471374519808667,3.904650440446,-38.3073109835682));
#17848=CARTESIAN_POINT('Ctrl Pts',(0.586770322034666,3.89071970792798,-38.3131773572585));
#17849=CARTESIAN_POINT('Ctrl Pts',(0.701597799363148,3.87166314337651,-38.3190437309488));
#17850=CARTESIAN_POINT('Ctrl Pts',(0.815372247446922,3.84755209166729,-38.3249101046391));
#17851=CARTESIAN_POINT('Ctrl Pts',(0.929131607419284,3.82344423742675,-38.3307757003648));
#17852=CARTESIAN_POINT('Ctrl Pts',(1.041837813855,3.79428331435358,-38.3366412960904));
#17853=CARTESIAN_POINT('Ctrl Pts',(1.15301635419074,3.76019178858854,-38.3425068918161));
#17854=CARTESIAN_POINT('Ctrl Pts',(1.2642067012028,3.72609664245208,-38.3483731104424));
#17855=CARTESIAN_POINT('Ctrl Pts',(1.37386866660868,3.68706997321528,-38.3542393290688));
#17856=CARTESIAN_POINT('Ctrl Pts',(1.48154355541025,3.64328391611501,-38.3601055476951));
#17857=CARTESIAN_POINT('Ctrl Pts',(1.59174005204084,3.59847244570237,-38.3661091456397));
#17858=CARTESIAN_POINT('Ctrl Pts',(1.69985482087368,3.54867605575534,-38.3721127435843));
#17859=CARTESIAN_POINT('Ctrl Pts',(1.80541974179486,3.49413058656046,-38.3781163415289));
#17860=CARTESIAN_POINT('Ctrl Pts',(1.90871976619197,3.44075539099915,-38.3839911322144));
#17861=CARTESIAN_POINT('Ctrl Pts',(2.00957792592519,3.38283310951248,-38.3898659228999));
#17862=CARTESIAN_POINT('Ctrl Pts',(2.10758319170174,3.32062977310876,-38.3957407135854));
#17863=CARTESIAN_POINT('Ctrl Pts',(2.20881166754664,3.25638068519777,-38.4018087151595));
#17864=CARTESIAN_POINT('Ctrl Pts',(2.30699596806504,3.18756437599956,-38.4078767167337));
#17865=CARTESIAN_POINT('Ctrl Pts',(2.40171937904222,3.11451971005692,-38.4139447183078));
#17866=CARTESIAN_POINT('Ctrl Pts',(2.49644279001939,3.04147504411429,-38.4200127198819));
#17867=CARTESIAN_POINT('Ctrl Pts',(2.5877049892177,2.96420237824787,-38.426080721456));
#17868=CARTESIAN_POINT('Ctrl Pts',(2.67513119754383,2.88308204460569,-38.4321487230301));
#17869=CARTESIAN_POINT('Ctrl Pts',(2.75860512206978,2.8056289245675,-38.4379424079573));
#17870=CARTESIAN_POINT('Ctrl Pts',(2.83886598245247,2.72440488468828,-38.4437360928845));
#17871=CARTESIAN_POINT('Ctrl Pts',(2.91554707754647,2.63971101422301,-38.4495297778117));
#17872=CARTESIAN_POINT('Ctrl Pts',(2.99213073461557,2.55512476354914,-38.455316100752));
#17873=CARTESIAN_POINT('Ctrl Pts',(3.06514338501152,2.46707775853196,-38.4611024236923));
#17874=CARTESIAN_POINT('Ctrl Pts',(3.13425271576831,2.37591012323677,-38.4668887466326));
#17875=CARTESIAN_POINT('Ctrl Pts',(3.20328640624917,2.28484227106803,-38.472668736433));
#17876=CARTESIAN_POINT('Ctrl Pts',(3.26842502046197,2.19066092033031,-38.4784487262333));
#17877=CARTESIAN_POINT('Ctrl Pts',(3.32937499763355,2.09374094031057,-38.4842287160337));
#17878=CARTESIAN_POINT('Ctrl Pts',(3.39028834502291,1.9968792073637,-38.4900052321696));
#17879=CARTESIAN_POINT('Ctrl Pts',(3.44701783152,1.89728247437855,-38.4957817483056));
#17880=CARTESIAN_POINT('Ctrl Pts',(3.49931221790545,1.79535595401514,-38.5015582644415));
#17881=CARTESIAN_POINT('Ctrl Pts',(3.55158863562845,1.69346445621088,-38.5073327957321));
#17882=CARTESIAN_POINT('Ctrl Pts',(3.59943278871211,1.58924514041807,-38.5131073270227));
#17883=CARTESIAN_POINT('Ctrl Pts',(3.64263899416319,1.4831285036037,-38.5188818583133));
#17884=CARTESIAN_POINT('Ctrl Pts',(3.68584147265992,1.37702102037868,-38.5246558914945));
#17885=CARTESIAN_POINT('Ctrl Pts',(3.72440664034969,1.26901693610166,-38.5304299246758));
#17886=CARTESIAN_POINT('Ctrl Pts',(3.75817698400003,1.15956662461992,-38.536203957857));
#17887=CARTESIAN_POINT('Ctrl Pts',(3.79196743080534,1.05005115843927,-38.5419814282637));
#17888=CARTESIAN_POINT('Ctrl Pts',(3.8209572275429,0.939088152567181,-38.5477588986704));
#17889=CARTESIAN_POINT('Ctrl Pts',(3.84503885974989,0.827142773052661,-38.5535363690771));
#17890=CARTESIAN_POINT('Ctrl Pts',(3.86912863085394,0.715159559228866,-38.5593157921021));
#17891=CARTESIAN_POINT('Ctrl Pts',(3.88830686104604,0.602193729592473,-38.5650952151271));
#17892=CARTESIAN_POINT('Ctrl Pts',(3.90251752942964,0.488718663951327,-38.5708746381522));
#17893=CARTESIAN_POINT('Ctrl Pts',(3.91674398053681,0.375117570065492,-38.5766604799489));
#17894=CARTESIAN_POINT('Ctrl Pts',(3.92599182103187,0.261006534640592,-38.5824463217456));
#17895=CARTESIAN_POINT('Ctrl Pts',(3.93025706314013,0.146861899882653,-38.5882321635423));
#17896=CARTESIAN_POINT('Ctrl Pts',(3.9321256614196,0.0968552501530872,-38.5907669350166));
#17897=CARTESIAN_POINT('Ctrl Pts',(3.93303862096152,0.0468421311809369,
-38.5933017064908));
#17898=CARTESIAN_POINT('Ctrl Pts',(3.93299874843716,-0.00313764111372402,
-38.595836477965));
#17899=CARTESIAN_POINT('Origin',(0.,0.,-41.3107734492731));
#17900=CARTESIAN_POINT('',(-0.0655702737400695,-3.22208288250033,-31.));
#17901=CARTESIAN_POINT('Ctrl Pts',(2.26878022305635,-2.28883242330415,-32.0941031001172));
#17902=CARTESIAN_POINT('Ctrl Pts',(2.30269587212703,-2.25521390537326,-32.0913860187157));
#17903=CARTESIAN_POINT('Ctrl Pts',(2.3358768770722,-2.22082908129709,-32.0886515262801));
#17904=CARTESIAN_POINT('Ctrl Pts',(2.42800183076779,-2.12100791224114,-32.080811535697));
#17905=CARTESIAN_POINT('Ctrl Pts',(2.48502712952621,-2.05390013857292,-32.075654741596));
#17906=CARTESIAN_POINT('Ctrl Pts',(2.56922013911977,-1.94617499834573,-32.0674804372658));
#17907=CARTESIAN_POINT('Ctrl Pts',(2.59833431977136,-1.90713073244486,-32.0645377956117));
#17908=CARTESIAN_POINT('Ctrl Pts',(2.65220736995442,-1.83135850178335,-32.0588554205981));
#17909=CARTESIAN_POINT('Ctrl Pts',(2.67711578430642,-1.79475030915057,-32.0561221581938));
#17910=CARTESIAN_POINT('Ctrl Pts',(2.73439706965908,-1.7067166145575,-32.0495718775103));
#17911=CARTESIAN_POINT('Ctrl Pts',(2.76608429868254,-1.65486731084621,-32.0457314351963));
#17912=CARTESIAN_POINT('Ctrl Pts',(2.88793183107832,-1.44220356192964,-32.0300387521813));
#17913=CARTESIAN_POINT('Ctrl Pts',(2.96567304885764,-1.27470322518631,-32.0177849534717));
#17914=CARTESIAN_POINT('Ctrl Pts',(3.09331620330717,-0.92373781956942,-31.9926617500646));
#17915=CARTESIAN_POINT('Ctrl Pts',(3.14219487871066,-0.740619039081715,
-31.9798357952823));
#17916=CARTESIAN_POINT('Ctrl Pts',(3.18160946083803,-0.514858005776426,
-31.9650076082526));
#17917=CARTESIAN_POINT('Ctrl Pts',(3.187754919486,-0.47532770888958,-31.9624479761529));
#17918=CARTESIAN_POINT('Ctrl Pts',(3.1965876061699,-0.410593318744866,-31.9583269425027));
#17919=CARTESIAN_POINT('Ctrl Pts',(3.19971625413538,-0.385454612938542,
-31.9567440216313));
#17920=CARTESIAN_POINT('Ctrl Pts',(3.20580697930199,-0.331313765153808,
-31.9533751303039));
#17921=CARTESIAN_POINT('Ctrl Pts',(3.20867257801835,-0.302303866281698,
-31.9515940349341));
#17922=CARTESIAN_POINT('Ctrl Pts',(3.2162103680128,-0.213724791241191,-31.946218100288));
#17923=CARTESIAN_POINT('Ctrl Pts',(3.21962021866489,-0.154058392539949,
-31.942682792648));
#17924=CARTESIAN_POINT('Ctrl Pts',(3.22399641357307,-0.00460818804654803,
-31.933967563008));
#17925=CARTESIAN_POINT('Ctrl Pts',(3.22287433168171,0.0851871518327197,
-31.9288565421208));
#17926=CARTESIAN_POINT('Ctrl Pts',(3.2046632018971,0.420403909893013,-31.9098902301207));
#17927=CARTESIAN_POINT('Ctrl Pts',(3.16325636419336,0.663632865041635,-31.8962881436646));
#17928=CARTESIAN_POINT('Ctrl Pts',(3.07709233789193,0.959973655136131,-31.8781473582528));
#17929=CARTESIAN_POINT('Ctrl Pts',(3.05784011597213,1.0196370668197,-31.8744161814322));
#17930=CARTESIAN_POINT('Ctrl Pts',(3.0219427872718,1.12069886589051,-31.8679379879319));
#17931=CARTESIAN_POINT('Ctrl Pts',(3.00615508434449,1.16238352830986,-31.8652188469219));
#17932=CARTESIAN_POINT('Ctrl Pts',(2.97156368826825,1.24829285180367,-31.8595096973298));
#17933=CARTESIAN_POINT('Ctrl Pts',(2.95262524849007,1.29245098684563,-31.8565158170679));
#17934=CARTESIAN_POINT('Ctrl Pts',(2.89794265830359,1.41247190050719,-31.8482076961596));
#17935=CARTESIAN_POINT('Ctrl Pts',(2.86021568274914,1.4873845560476,-31.8428297275885));
#17936=CARTESIAN_POINT('Ctrl Pts',(2.76453808458551,1.660234932916,-31.8299589198227));
#17937=CARTESIAN_POINT('Ctrl Pts',(2.7042386826883,1.75674145185515,-31.8224025883023));
#17938=CARTESIAN_POINT('Ctrl Pts',(2.51835046277141,2.02192649814793,-31.8006806392809));
#17939=CARTESIAN_POINT('Ctrl Pts',(2.38118727065392,2.18179513333603,-31.7863673364536));
#17940=CARTESIAN_POINT('Ctrl Pts',(2.19910212015222,2.35623250327597,-31.7700197899927));
#17941=CARTESIAN_POINT('Ctrl Pts',(2.16820519540113,2.38469460311477,-31.7673272032451));
#17942=CARTESIAN_POINT('Ctrl Pts',(2.1192441238804,2.42805875671053,-31.7631965030385));
#17943=CARTESIAN_POINT('Ctrl Pts',(2.10155990629271,2.44338106947639,-31.7617312102999));
#17944=CARTESIAN_POINT('Ctrl Pts',(2.062636805982,2.4763703300216,-31.7585665859691));
#17945=CARTESIAN_POINT('Ctrl Pts',(2.04133452434316,2.49395951995371,-31.7568726621206));
#17946=CARTESIAN_POINT('Ctrl Pts',(1.98016617939621,2.54315699397321,-31.7521071192955));
#17947=CARTESIAN_POINT('Ctrl Pts',(1.93977274742268,2.57409943223772,-31.7490763838719));
#17948=CARTESIAN_POINT('Ctrl Pts',(1.68799945715152,2.75767031803509,-31.7307714439952));
#17949=CARTESIAN_POINT('Ctrl Pts',(1.45946248703766,2.88514861247454,-31.716552284361));
#17950=CARTESIAN_POINT('Ctrl Pts',(1.11508615136928,3.02573419869209,-31.6953322758645));
#17951=CARTESIAN_POINT('Ctrl Pts',(1.01002941456809,3.06240460224482,-31.6888950791099));
#17952=CARTESIAN_POINT('Ctrl Pts',(0.851906628966527,3.10857498452044,-31.6791138783058));
#17953=CARTESIAN_POINT('Ctrl Pts',(0.800155972205574,3.12229615346054,-31.6758990856793));
#17954=CARTESIAN_POINT('Ctrl Pts',(0.705447768261373,3.14489791590229,-31.6699781646605));
#17955=CARTESIAN_POINT('Ctrl Pts',(0.662604332069828,3.15420269890428,-31.6672859744977));
#17956=CARTESIAN_POINT('Ctrl Pts',(0.566881153817695,3.17295567740038,-31.6612346210127));
#17957=CARTESIAN_POINT('Ctrl Pts',(0.513929102191623,3.18196139420478,-31.6578626683127));
#17958=CARTESIAN_POINT('Ctrl Pts',(0.338186920964142,3.20734931902271,-31.6465827152656));
#17959=CARTESIAN_POINT('Ctrl Pts',(0.214688733257574,3.21797498435541,-31.6385086451206));
#17960=CARTESIAN_POINT('Ctrl Pts',(-0.164398127653997,3.22867126088657,
-31.6133465045129));
#17961=CARTESIAN_POINT('Ctrl Pts',(-0.419630197333096,3.20550307952549,
-31.5958110542406));
#17962=CARTESIAN_POINT('Ctrl Pts',(-0.715661544293251,3.14263875912357,
-31.5760935929661));
#17963=CARTESIAN_POINT('Ctrl Pts',(-0.761659009348888,3.13180872361144,
-31.573051191581));
#17964=CARTESIAN_POINT('Ctrl Pts',(-0.833431711139318,3.11323496455642,
-31.5683542780195));
#17965=CARTESIAN_POINT('Ctrl Pts',(-0.859374979166682,3.10617371097775,
-31.5666669691321));
#17966=CARTESIAN_POINT('Ctrl Pts',(-0.911158601851891,3.09138073372402,
-31.5633241894602));
#17967=CARTESIAN_POINT('Ctrl Pts',(-0.936996283277776,3.08364766297524,
-31.5616690316654));
#17968=CARTESIAN_POINT('Ctrl Pts',(-1.00880741785217,3.06116903065983,-31.5570967016156));
#17969=CARTESIAN_POINT('Ctrl Pts',(-1.05455284652535,3.0457128996373,-31.5542161352676));
#17970=CARTESIAN_POINT('Ctrl Pts',(-1.32227346001728,2.94850165182541,-31.5374550333712));
#17971=CARTESIAN_POINT('Ctrl Pts',(-1.53506666740538,2.84352973759563,-31.5244859336924));
#17972=CARTESIAN_POINT('Ctrl Pts',(-1.8486230714047,2.64330393188778,-31.503442160978));
#17973=CARTESIAN_POINT('Ctrl Pts',(-1.95805997802934,2.5632906514834,-31.4956768753677));
#17974=CARTESIAN_POINT('Ctrl Pts',(-2.10495182836704,2.4409833879626,-31.4843667723144));
#17975=CARTESIAN_POINT('Ctrl Pts',(-2.14683672580388,2.40422828016424,-31.481031037112));
#17976=CARTESIAN_POINT('Ctrl Pts',(-2.21973917301845,2.33682989497028,-31.4750084337969));
#17977=CARTESIAN_POINT('Ctrl Pts',(-2.25112785249876,2.30660769562419,-31.4723393004983));
#17978=CARTESIAN_POINT('Ctrl Pts',(-2.317892180431,2.23966342732664,-31.4664879098487));
#17979=CARTESIAN_POINT('Ctrl Pts',(-2.35302801223078,2.202719940847,-31.4632964038722));
#17980=CARTESIAN_POINT('Ctrl Pts',(-2.45722597128624,2.0878223097116,-31.4534750989155));
#17981=CARTESIAN_POINT('Ctrl Pts',(-2.52339422669504,2.00734636645594,-31.4467340633678));
#17982=CARTESIAN_POINT('Ctrl Pts',(-2.68520786206053,1.78987402617002,-31.4288816559198));
#17983=CARTESIAN_POINT('Ctrl Pts',(-2.77430483842334,1.648397997535,-31.4176029251084));
#17984=CARTESIAN_POINT('Ctrl Pts',(-2.91043134972012,1.38968839206108,-31.397928445544));
#17985=CARTESIAN_POINT('Ctrl Pts',(-2.96230373536414,1.27538452830868,-31.389534996897));
#17986=CARTESIAN_POINT('Ctrl Pts',(-3.02236140857858,1.11945758137157,-31.3787011399939));
#17987=CARTESIAN_POINT('Ctrl Pts',(-3.03658318505253,1.08028546676466,-31.3760297322998));
#17988=CARTESIAN_POINT('Ctrl Pts',(-3.05755513936169,1.01883035529114,-31.3719281059413));
#17989=CARTESIAN_POINT('Ctrl Pts',(-3.06483007944046,0.996732371151817,
-31.3704710348326));
#17990=CARTESIAN_POINT('Ctrl Pts',(-3.08019773835946,0.948292502860615,
-31.367318589169));
#17991=CARTESIAN_POINT('Ctrl Pts',(-3.08819316807161,0.921921828038814,
-31.3656286564869));
#17992=CARTESIAN_POINT('Ctrl Pts',(-3.10991403963639,0.846826073182173,
-31.3608820573509));
#17993=CARTESIAN_POINT('Ctrl Pts',(-3.12283166864551,0.797873862074177,
-31.3578658852015));
#17994=CARTESIAN_POINT('Ctrl Pts',(-3.15080775411709,0.68073585731148,-31.3507895851501));
#17995=CARTESIAN_POINT('Ctrl Pts',(-3.16481450273892,0.61232424050743,-31.3467688140367));
#17996=CARTESIAN_POINT('Ctrl Pts',(-3.19910731805787,0.411896488304255,
-31.3351797423718));
#17997=CARTESIAN_POINT('Ctrl Pts',(-3.21342524759083,0.279009445096801,
-31.3277297440384));
#17998=CARTESIAN_POINT('Ctrl Pts',(-3.22617513392283,-0.00288311090345444,
-31.3118281237634));
#17999=CARTESIAN_POINT('Ctrl Pts',(-3.22260910205966,-0.151655446097844,
-31.3033745228977));
#18000=CARTESIAN_POINT('Ctrl Pts',(-3.20296404878469,-0.362028737096515,
-31.2909499679528));
#18001=CARTESIAN_POINT('Ctrl Pts',(-3.19532051171561,-0.424228219590455,
-31.2872189729755));
#18002=CARTESIAN_POINT('Ctrl Pts',(-3.17912239871893,-0.530375980310534,
-31.2807310808168));
#18003=CARTESIAN_POINT('Ctrl Pts',(-3.17145607016934,-0.574442338233476,
-31.2780017416837));
#18004=CARTESIAN_POINT('Ctrl Pts',(-3.15359270007901,-0.665816384975227,
-31.2722606617297));
#18005=CARTESIAN_POINT('Ctrl Pts',(-3.14324221796188,-0.713082283954703,
-31.2692448158096));
#18006=CARTESIAN_POINT('Ctrl Pts',(-3.11176594421387,-0.842774434622913,
-31.2608354659203));
#18007=CARTESIAN_POINT('Ctrl Pts',(-3.08843516383748,-0.924620061884636,
-31.2553763052914));
#18008=CARTESIAN_POINT('Ctrl Pts',(-3.02558624848566,-1.11601539650809,
-31.2422465991681));
#18009=CARTESIAN_POINT('Ctrl Pts',(-2.98331645446263,-1.2245333145831,-31.2345092128059));
#18010=CARTESIAN_POINT('Ctrl Pts',(-2.84683434058708,-1.52562782989232,
-31.2123349254712));
#18011=CARTESIAN_POINT('Ctrl Pts',(-2.73915864165989,-1.71143953051354,
-31.1977602821704));
#18012=CARTESIAN_POINT('Ctrl Pts',(-2.59200322478139,-1.91547121703878,
-31.1815462251745));
#18013=CARTESIAN_POINT('Ctrl Pts',(-2.56964415841414,-1.94536368647978,
-31.179166091185));
#18014=CARTESIAN_POINT('Ctrl Pts',(-2.53109526381668,-1.99507609176752,
-31.1752088826466));
#18015=CARTESIAN_POINT('Ctrl Pts',(-2.51518061578726,-2.01510259144709,
-31.1736154309618));
#18016=CARTESIAN_POINT('Ctrl Pts',(-2.47892010326292,-2.05963267355287,
-31.1700746107593));
#18017=CARTESIAN_POINT('Ctrl Pts',(-2.45844685070412,-2.08402756333465,
-31.168135528056));
#18018=CARTESIAN_POINT('Ctrl Pts',(-2.38849551672843,-2.16491228950299,
-31.1616931827404));
#18019=CARTESIAN_POINT('Ctrl Pts',(-2.33740288336412,-2.21997870014927,
-31.1572851492136));
#18020=CARTESIAN_POINT('Ctrl Pts',(-2.19097751449322,-2.3671265401398,-31.1452814776906));
#18021=CARTESIAN_POINT('Ctrl Pts',(-2.09181904310293,-2.45519179676638,
-31.1378321512879));
#18022=CARTESIAN_POINT('Ctrl Pts',(-1.85325953013115,-2.64208918767056,
-31.1207230777363));
#18023=CARTESIAN_POINT('Ctrl Pts',(-1.71087525839875,-2.7364402932757,-31.1110608474382));
#18024=CARTESIAN_POINT('Ctrl Pts',(-1.50651259155632,-2.84965223764059,
-31.0973114263493));
#18025=CARTESIAN_POINT('Ctrl Pts',(-1.45044094734478,-2.87859659783319,
-31.093552525306));
#18026=CARTESIAN_POINT('Ctrl Pts',(-1.35288614956159,-2.92538054189175,
-31.0870124948111));
#18027=CARTESIAN_POINT('Ctrl Pts',(-1.31181042617959,-2.94402876150796,
-31.084258834697));
#18028=CARTESIAN_POINT('Ctrl Pts',(-1.22533804724394,-2.9811178989734,-31.078454839349));
#18029=CARTESIAN_POINT('Ctrl Pts',(-1.17988536754214,-2.99939783501842,
-31.0754001215773));
#18030=CARTESIAN_POINT('Ctrl Pts',(-1.05268546505144,-3.04721577114661,
-31.0668333619798));
#18031=CARTESIAN_POINT('Ctrl Pts',(-0.97013804256901,-3.07449193760006,
-31.0612525060389));
#18032=CARTESIAN_POINT('Ctrl Pts',(-0.771583036524189,-3.13130771240993,
-31.0477775922899));
#18033=CARTESIAN_POINT('Ctrl Pts',(-0.654836372250052,-3.15778621998811,
-31.0398119698717));
#18034=CARTESIAN_POINT('Ctrl Pts',(-0.381070158534853,-3.2040408954779,
-31.0211616860773));
#18035=CARTESIAN_POINT('Ctrl Pts',(-0.223536725865423,-3.21886822170937,
-31.0104465088182));
#18036=CARTESIAN_POINT('Ctrl Pts',(-0.0655702737400695,-3.22208288250033,
-31.));
#18037=CARTESIAN_POINT('',(-3.05625919777041,-1.02244671183577,-31.));
#18038=CARTESIAN_POINT('Origin',(0.,0.,-31.));
#18039=CARTESIAN_POINT('Ctrl Pts',(-3.05625919777041,-1.02244671183577,
-31.));
#18040=CARTESIAN_POINT('Ctrl Pts',(-3.06368966725375,-1.00023583234511,
-31.0014457916658));
#18041=CARTESIAN_POINT('Ctrl Pts',(-3.07087800392366,-0.977943988332985,
-31.002880504093));
#18042=CARTESIAN_POINT('Ctrl Pts',(-3.08701830394628,-0.925957511541264,
-31.0061922236022));
#18043=CARTESIAN_POINT('Ctrl Pts',(-3.09578601304777,-0.896207788930303,
-31.0080617128447));
#18044=CARTESIAN_POINT('Ctrl Pts',(-3.1589685710295,-0.66982147584979,-31.0221223008988));
#18045=CARTESIAN_POINT('Ctrl Pts',(-3.19503326635304,-0.468528200778728,
-31.0336998688189));
#18046=CARTESIAN_POINT('Ctrl Pts',(-3.22382371044213,-0.119802007364771,
-31.0538520637253));
#18047=CARTESIAN_POINT('Ctrl Pts',(-3.225941836979,0.0261969329579913,-31.0623149907551));
#18048=CARTESIAN_POINT('Ctrl Pts',(-3.2150766966268,0.229687745429387,-31.0744904123262));
#18049=CARTESIAN_POINT('Ctrl Pts',(-3.21042786623023,0.287449115648635,
-31.0779882507207));
#18050=CARTESIAN_POINT('Ctrl Pts',(-3.1990117194526,0.39346197962638,-31.0845041375768));
#18051=CARTESIAN_POINT('Ctrl Pts',(-3.19270235691127,0.441746090229753,
-31.0875087640725));
#18052=CARTESIAN_POINT('Ctrl Pts',(-3.17598813756868,0.55042832070649,-31.0943654185429));
#18053=CARTESIAN_POINT('Ctrl Pts',(-3.16494966697735,0.610708475448756,
-31.0982344076252));
#18054=CARTESIAN_POINT('Ctrl Pts',(-3.11743162289897,0.834058741912733,
-31.1128358535922));
#18055=CARTESIAN_POINT('Ctrl Pts',(-3.07001141816015,0.994510294080951,
-31.1238758879573));
#18056=CARTESIAN_POINT('Ctrl Pts',(-2.94714504766617,1.31598743195748,-31.1470409037298));
#18057=CARTESIAN_POINT('Ctrl Pts',(-2.87038463933554,1.4759330295311,-31.1591527075447));
#18058=CARTESIAN_POINT('Ctrl Pts',(-2.74962979707509,1.68210439534145,-31.1751409476614));
#18059=CARTESIAN_POINT('Ctrl Pts',(-2.71685642060489,1.73454063375296,-31.1792406023768));
#18060=CARTESIAN_POINT('Ctrl Pts',(-2.65662281659608,1.82501201368435,-31.186337945505));
#18061=CARTESIAN_POINT('Ctrl Pts',(-2.62980306552993,1.86345109653001,-31.1893613441493));
#18062=CARTESIAN_POINT('Ctrl Pts',(-2.58623635035271,1.9230774748852,-31.1940486022615));
#18063=CARTESIAN_POINT('Ctrl Pts',(-2.57004619167942,1.94466144229419,-31.195744757829));
#18064=CARTESIAN_POINT('Ctrl Pts',(-2.53956426353007,1.98425281189865,-31.1988513756385));
#18065=CARTESIAN_POINT('Ctrl Pts',(-2.52534787880142,2.00231465682156,-31.2002664296262));
#18066=CARTESIAN_POINT('Ctrl Pts',(-2.48449699589171,2.05308829189956,-31.2042423177796));
#18067=CARTESIAN_POINT('Ctrl Pts',(-2.45741070761794,2.0854327744636,-31.2067730287731));
#18068=CARTESIAN_POINT('Ctrl Pts',(-2.29511517705172,2.27167957011959,-31.2213978453259));
#18069=CARTESIAN_POINT('Ctrl Pts',(-2.14610099964124,2.41295476041724,-31.2327303683791));
#18070=CARTESIAN_POINT('Ctrl Pts',(-1.86011285301185,2.63649192477108,-31.2531034964869));
#18071=CARTESIAN_POINT('Ctrl Pts',(-1.728572126257,2.72454428744957,-31.2620448358675));
#18072=CARTESIAN_POINT('Ctrl Pts',(-1.53847462413816,2.83246837849274,-31.274878888015));
#18073=CARTESIAN_POINT('Ctrl Pts',(-1.48500867909494,2.86086172410591,-31.2784777954861));
#18074=CARTESIAN_POINT('Ctrl Pts',(-1.39258807477507,2.90665313853114,-31.2847013887399));
#18075=CARTESIAN_POINT('Ctrl Pts',(-1.35402868087581,2.9248145364131,-31.2872986236609));
#18076=CARTESIAN_POINT('Ctrl Pts',(-1.27376644301661,2.96069055920054,-31.2927122448261));
#18077=CARTESIAN_POINT('Ctrl Pts',(-1.23202769743837,2.97830101775068,-31.2955315294312));
#18078=CARTESIAN_POINT('Ctrl Pts',(-1.11916203578566,3.02314291374768,-31.3031718607527));
#18079=CARTESIAN_POINT('Ctrl Pts',(-1.04742167105526,3.04874121795445,-31.3080463126545));
#18080=CARTESIAN_POINT('Ctrl Pts',(-0.722510290549048,3.15185389725355,
-31.330210741756));
#18081=CARTESIAN_POINT('Ctrl Pts',(-0.46128815079424,3.20052802961832,-31.3483791259836));
#18082=CARTESIAN_POINT('Ctrl Pts',(-0.127446697404474,3.22098540369439,
-31.3708753888323));
#18083=CARTESIAN_POINT('Ctrl Pts',(-0.0576529010695713,3.22299035606959,
-31.3755313199506));
#18084=CARTESIAN_POINT('Ctrl Pts',(0.0623773136828261,3.2225376660785,-31.3834024835212));
#18085=CARTESIAN_POINT('Ctrl Pts',(0.112592210636624,3.22117425371005,-31.386654333067));
#18086=CARTESIAN_POINT('Ctrl Pts',(0.189303426318992,3.21729517610779,-31.3915388576666));
#18087=CARTESIAN_POINT('Ctrl Pts',(0.215833062098524,3.21562440419861,-31.3932127962895));
#18088=CARTESIAN_POINT('Ctrl Pts',(0.268190723828241,3.21167609133527,-31.396482340816));
#18089=CARTESIAN_POINT('Ctrl Pts',(0.294017176982475,3.20941483523529,-31.3980790765947));
#18090=CARTESIAN_POINT('Ctrl Pts',(0.361997564615379,3.20263523238189,-31.4022462306662));
#18091=CARTESIAN_POINT('Ctrl Pts',(0.404095715928131,3.19759623734473,-31.4047904924148));
#18092=CARTESIAN_POINT('Ctrl Pts',(0.60860659234301,3.16901325569792,-31.4170253917112));
#18093=CARTESIAN_POINT('Ctrl Pts',(0.769172918918247,3.13391614655204,-31.4262542217489));
#18094=CARTESIAN_POINT('Ctrl Pts',(1.06241237340047,3.04591024737248,-31.4434607677009));
#18095=CARTESIAN_POINT('Ctrl Pts',(1.19559428055507,2.99613773100335,-31.4514208837747));
#18096=CARTESIAN_POINT('Ctrl Pts',(1.41269034876644,2.89821775327242,-31.4651117496847));
#18097=CARTESIAN_POINT('Ctrl Pts',(1.49850783341695,2.85479108607176,-31.4707228556424));
#18098=CARTESIAN_POINT('Ctrl Pts',(1.62620156623365,2.78282790186384,-31.4794690676037));
#18099=CARTESIAN_POINT('Ctrl Pts',(1.66956217675269,2.75703180770333,-31.4825120780828));
#18100=CARTESIAN_POINT('Ctrl Pts',(1.75017032253303,2.70647739744948,-31.4883189821727));
#18101=CARTESIAN_POINT('Ctrl Pts',(1.78754300763295,2.6819406690684,-31.491074558226));
#18102=CARTESIAN_POINT('Ctrl Pts',(1.87277349881676,2.62341031381723,-31.4975127638752));
#18103=CARTESIAN_POINT('Ctrl Pts',(1.92023587157573,2.58887152363114,-31.5012145268787));
#18104=CARTESIAN_POINT('Ctrl Pts',(2.151877929996,2.41042801712911,-31.5198836809907));
#18105=CARTESIAN_POINT('Ctrl Pts',(2.32094072454142,2.248098242461,-31.5355387515505));
#18106=CARTESIAN_POINT('Ctrl Pts',(2.53282185524368,1.99504928356514,-31.5576717531323));
#18107=CARTESIAN_POINT('Ctrl Pts',(2.59135730808181,1.9184048147051,-31.5641166666995));
#18108=CARTESIAN_POINT('Ctrl Pts',(2.68203956004036,1.7879282463809,-31.5745573751123));
#18109=CARTESIAN_POINT('Ctrl Pts',(2.71620988307163,1.735577282764,-31.5786149286894));
#18110=CARTESIAN_POINT('Ctrl Pts',(2.76448768556705,1.65669074393811,-31.5845030371213));
#18111=CARTESIAN_POINT('Ctrl Pts',(2.77978038810149,1.63090083366546,-31.5863934382334));
#18112=CARTESIAN_POINT('Ctrl Pts',(2.80752340019051,1.5825902181051,-31.5898656822868));
#18113=CARTESIAN_POINT('Ctrl Pts',(2.82006683015137,1.56012901686155,-31.5914523496926));
#18114=CARTESIAN_POINT('Ctrl Pts',(2.85177300000097,1.50172145041604,-31.5955115941272));
#18115=CARTESIAN_POINT('Ctrl Pts',(2.87052556326866,1.46555787469823,-31.5979611657829));
#18116=CARTESIAN_POINT('Ctrl Pts',(2.96951586831282,1.26546487276322,-31.6112206540704));
#18117=CARTESIAN_POINT('Ctrl Pts',(3.03641006742162,1.09528688862761,-31.6214442160957));
#18118=CARTESIAN_POINT('Ctrl Pts',(3.12589044186297,0.795004422728859,-31.6390740870646));
#18119=CARTESIAN_POINT('Ctrl Pts',(3.15557468942645,0.66750968059083,-31.6464383820955));
#18120=CARTESIAN_POINT('Ctrl Pts',(3.19268269695692,0.448581385771919,-31.659241738571));
#18121=CARTESIAN_POINT('Ctrl Pts',(3.20410480734677,0.357992238509676,-31.6645829008062));
#18122=CARTESIAN_POINT('Ctrl Pts',(3.21575888037754,0.217832593882884,-31.6729882330568));
#18123=CARTESIAN_POINT('Ctrl Pts',(3.21871900304368,0.168534277721682,-31.6759710652802));
#18124=CARTESIAN_POINT('Ctrl Pts',(3.2221876273703,0.0748105921557126,-31.6817018316883));
#18125=CARTESIAN_POINT('Ctrl Pts',(3.22291250222038,0.0304044745985394,
-31.6844425394197));
#18126=CARTESIAN_POINT('Ctrl Pts',(3.22245805109125,-0.0742015105409391,
-31.6909645857511));
#18127=CARTESIAN_POINT('Ctrl Pts',(3.22050975858975,-0.134379685467865,
-31.6947681564767));
#18128=CARTESIAN_POINT('Ctrl Pts',(3.20098917367345,-0.45729290420798,-31.7154690395089));
#18129=CARTESIAN_POINT('Ctrl Pts',(3.15295114961931,-0.717150366740733,
-31.7332802961136));
#18130=CARTESIAN_POINT('Ctrl Pts',(3.04863743216703,-1.04832299439081,-31.7566078811022));
#18131=CARTESIAN_POINT('Ctrl Pts',(3.02028215730451,-1.12741666957471,-31.7622183823982));
#18132=CARTESIAN_POINT('Ctrl Pts',(2.96744270566311,-1.2584447131418,-31.7714948272407));
#18133=CARTESIAN_POINT('Ctrl Pts',(2.94460319285558,-1.31099663952812,-31.7752100388339));
#18134=CARTESIAN_POINT('Ctrl Pts',(2.90820949774069,-1.3889788952928,-31.7806870682699));
#18135=CARTESIAN_POINT('Ctrl Pts',(2.8956967382222,-1.41487999232281,-31.7825000701201));
#18136=CARTESIAN_POINT('Ctrl Pts',(2.87147338060518,-1.46335388131127,-31.7858767548139));
#18137=CARTESIAN_POINT('Ctrl Pts',(2.85983970098786,-1.48596126225074,-31.7874442407776));
#18138=CARTESIAN_POINT('Ctrl Pts',(2.82879287135425,-1.54457819228725,-31.7914942835404));
#18139=CARTESIAN_POINT('Ctrl Pts',(2.80895881611487,-1.58036122910465,-31.7939528305251));
#18140=CARTESIAN_POINT('Ctrl Pts',(2.70191715950857,-1.7650918279723,-31.8066229361826));
#18141=CARTESIAN_POINT('Ctrl Pts',(2.60352100332794,-1.90724827281157,-31.8163069293231));
#18142=CARTESIAN_POINT('Ctrl Pts',(2.42340092316841,-2.12738003006174,-31.832286277038));
#18143=CARTESIAN_POINT('Ctrl Pts',(2.34815673343164,-2.21015132447384,-31.8385591031073));
#18144=CARTESIAN_POINT('Ctrl Pts',(2.26878017977789,-2.28883246620346,-31.8449383693487));
#18145=CARTESIAN_POINT('Ctrl Pts',(-0.500000469481151,-0.249903141543597,
-18.9999974608925));
#18146=CARTESIAN_POINT('Ctrl Pts',(-0.499985698708809,-0.249901829883283,
-18.9999972921557));
#18147=CARTESIAN_POINT('Ctrl Pts',(-0.499943925311476,-0.225581277443933,
-18.9999914184955));
#18148=CARTESIAN_POINT('Ctrl Pts',(-0.49990522080778,-0.0968325121338559,
-18.9999912742066));
#18149=CARTESIAN_POINT('Ctrl Pts',(-0.49990535449692,0.0576086556106972,
-18.9999912543048));
#18150=CARTESIAN_POINT('Ctrl Pts',(-0.499924487061938,0.161824257995483,
-18.9999913623149));
#18151=CARTESIAN_POINT('Ctrl Pts',(-0.49995797003322,0.233166202229003,
-18.9999933695672));
#18152=CARTESIAN_POINT('Ctrl Pts',(-0.499985738345136,0.249901825054466,
-18.999997299666));
#18153=CARTESIAN_POINT('Ctrl Pts',(-0.500000469481151,0.249903141543597,
-18.9999974608925));
#18154=CARTESIAN_POINT('Ctrl Pts',(-0.500005798667243,-1.0727321416819,
-18.9999686389119));
#18155=CARTESIAN_POINT('Ctrl Pts',(-0.617767115371394,-1.05838542886533,
-19.0222827327148));
#18156=CARTESIAN_POINT('Ctrl Pts',(-0.961750910786003,-0.9263461965772,
-19.0706508378555));
#18157=CARTESIAN_POINT('Ctrl Pts',(-1.28046409080139,-0.399643500127231,
-19.0718389690549));
#18158=CARTESIAN_POINT('Ctrl Pts',(-1.27936322016631,0.237312703455417,
-19.0720028526044));
#18159=CARTESIAN_POINT('Ctrl Pts',(-1.12181565277689,0.665712549520801,
-19.071113446577));
#18160=CARTESIAN_POINT('Ctrl Pts',(-0.846099392010201,0.968022332176519,
-19.0545842535533));
#18161=CARTESIAN_POINT('Ctrl Pts',(-0.617440729391164,1.05842519205801,
-19.0222208872159));
#18162=CARTESIAN_POINT('Ctrl Pts',(-0.500005798667244,1.0727321416819,-18.9999686389119));
#18163=CARTESIAN_POINT('Ctrl Pts',(-0.374652368818645,-2.49810309995234,
-19.6779209672235));
#18164=CARTESIAN_POINT('Ctrl Pts',(-0.709305686727837,-2.46080605400923,
-19.7142757163881));
#18165=CARTESIAN_POINT('Ctrl Pts',(-1.68368326934235,-2.14240101116334,
-19.7931584654386));
#18166=CARTESIAN_POINT('Ctrl Pts',(-2.57589728694922,-0.923785230808655,
-19.797316584276));
#18167=CARTESIAN_POINT('Ctrl Pts',(-2.57299505475586,0.5493050318438,-19.7976926645488));
#18168=CARTESIAN_POINT('Ctrl Pts',(-2.1316902523392,1.54026532815555,-19.7949687092533));
#18169=CARTESIAN_POINT('Ctrl Pts',(-1.35624613497006,2.24246988768653,-19.767059280983));
#18170=CARTESIAN_POINT('Ctrl Pts',(-0.708378165244041,2.46090942609474,
-19.7141749559621));
#18171=CARTESIAN_POINT('Ctrl Pts',(-0.374652368818646,2.49810309995235,
-19.6779209672235));
#18172=CARTESIAN_POINT('Ctrl Pts',(-0.112199737628206,-3.,-21.0973505959298));
#18173=CARTESIAN_POINT('Ctrl Pts',(-0.545411427143743,-2.98330034061038,
-21.1128737181934));
#18174=CARTESIAN_POINT('Ctrl Pts',(-1.8433426587387,-2.65791691005246,-21.1489665252715));
#18175=CARTESIAN_POINT('Ctrl Pts',(-3.03119195141778,-1.14304648239468,
-21.1569911263128));
#18176=CARTESIAN_POINT('Ctrl Pts',(-3.02358946238589,0.679679924198355,
-21.1570610940823));
#18177=CARTESIAN_POINT('Ctrl Pts',(-2.44325522122211,1.90810624850608,-21.152940585479));
#18178=CARTESIAN_POINT('Ctrl Pts',(-1.40427919869758,2.75990650054913,-21.1369518532818));
#18179=CARTESIAN_POINT('Ctrl Pts',(-0.544210742352787,2.98334662520411,
-21.1128306944771));
#18180=CARTESIAN_POINT('Ctrl Pts',(-0.112199737628208,3.,-21.0973505959298));
#18181=CARTESIAN_POINT('Ctrl Pts',(1.23694807792704E-15,-3.,-21.704163456598));
#18182=CARTESIAN_POINT('Ctrl Pts',(-0.443076803624563,-3.,-21.7109905340956));
#18183=CARTESIAN_POINT('Ctrl Pts',(-1.79348272300302,-2.70799641386265,
-21.7291868478869));
#18184=CARTESIAN_POINT('Ctrl Pts',(-3.03256791313562,-1.16243137143974,
-21.7388525256077));
#18185=CARTESIAN_POINT('Ctrl Pts',(-3.02252425451967,0.691565714094212,
-21.7387856518469));
#18186=CARTESIAN_POINT('Ctrl Pts',(-2.42127475768073,1.9426253115599,-21.7340800035291));
#18187=CARTESIAN_POINT('Ctrl Pts',(-1.33503228345836,2.79906518555955,-21.7230542680391));
#18188=CARTESIAN_POINT('Ctrl Pts',(-0.441848776791001,3.,-21.7109716122421));
#18189=CARTESIAN_POINT('Ctrl Pts',(-1.51085184250722E-15,3.,-21.704163456598));
#18190=CARTESIAN_POINT('',(-0.500000234886957,0.250003172328595,-18.999998729662));
#18191=CARTESIAN_POINT('',(-0.499951156893989,2.95746669263463,-21.7115242851505));
#18192=CARTESIAN_POINT('Ctrl Pts',(-0.500000469773915,0.250006344657191,
-18.9999974593239));
#18193=CARTESIAN_POINT('Ctrl Pts',(-0.500000469773915,0.267897220596353,
-18.9999975513786));
#18194=CARTESIAN_POINT('Ctrl Pts',(-0.5,0.285781297776546,-19.0001870446818));
#18195=CARTESIAN_POINT('Ctrl Pts',(-0.5,0.647589705255165,-19.007829931103));
#18196=CARTESIAN_POINT('Ctrl Pts',(-0.500000000105581,0.988814386378878,
-19.0846439716327));
#18197=CARTESIAN_POINT('Ctrl Pts',(-0.500000000105581,1.62420230789884,
-19.3558232592152));
#18198=CARTESIAN_POINT('Ctrl Pts',(-0.500000000128244,1.9184553255922,-19.5513503907418));
#18199=CARTESIAN_POINT('Ctrl Pts',(-0.500000000128245,2.44455222346988,
-20.0714825223491));
#18200=CARTESIAN_POINT('Ctrl Pts',(-0.499999999835989,2.62277718310116,
-20.3702706616735));
#18201=CARTESIAN_POINT('Ctrl Pts',(-0.499999999835989,2.81085194241867,
-20.8142013992923));
#18202=CARTESIAN_POINT('Ctrl Pts',(-0.499999999999019,2.86545769478055,
-20.9898894108025));
#18203=CARTESIAN_POINT('Ctrl Pts',(-0.499999999999019,2.93869922770866,
-21.3474407116196));
#18204=CARTESIAN_POINT('Ctrl Pts',(-0.500000000000001,2.95754616741604,
-21.5294711463845));
#18205=CARTESIAN_POINT('Ctrl Pts',(-0.500000000000001,2.95745837384903,
-21.7115232284929));
#18206=CARTESIAN_POINT('',(-0.500115915134107,-2.95873777012636,-21.7115199198582));
#18207=CARTESIAN_POINT('Ctrl Pts',(-0.499951156893989,2.95746669263463,
-21.7115242851505));
#18208=CARTESIAN_POINT('Ctrl Pts',(-0.77304186182352,2.91095244475281,-21.7153647174257));
#18209=CARTESIAN_POINT('Ctrl Pts',(-1.47173376114598,2.69128391286519,-21.7244418351522));
#18210=CARTESIAN_POINT('Ctrl Pts',(-2.42127475768073,1.9426253115599,-21.7340800035291));
#18211=CARTESIAN_POINT('Ctrl Pts',(-3.02252425451967,0.691565714094212,
-21.7387856518469));
#18212=CARTESIAN_POINT('Ctrl Pts',(-3.03256791313562,-1.16243137143974,
-21.7388525256077));
#18213=CARTESIAN_POINT('Ctrl Pts',(-1.91000215743889,-2.56265663733954,
-21.7300957759497));
#18214=CARTESIAN_POINT('Ctrl Pts',(-0.775090713331855,-2.91314336467866,
-21.7153814269834));
#18215=CARTESIAN_POINT('Ctrl Pts',(-0.500115915134107,-2.95873777012636,
-21.7115199198582));
#18216=CARTESIAN_POINT('',(-0.500000234886961,-0.250003167767838,-18.9999987296619));
#18217=CARTESIAN_POINT('Ctrl Pts',(-0.499999999999999,-2.95875698808065,
-21.7115182923403));
#18218=CARTESIAN_POINT('Ctrl Pts',(-0.499999999999999,-2.95871464996716,
-21.5295301198306));
#18219=CARTESIAN_POINT('Ctrl Pts',(-0.499999999998966,-2.93976151442474,
-21.3475736692592));
#18220=CARTESIAN_POINT('Ctrl Pts',(-0.499999999998966,-2.86636109777345,
-20.9901733930264));
#18221=CARTESIAN_POINT('Ctrl Pts',(-0.499999999825091,-2.81169983008533,
-20.8145582299835));
#18222=CARTESIAN_POINT('Ctrl Pts',(-0.499999999825091,-2.62343698647115,
-20.3705392694364));
#18223=CARTESIAN_POINT('Ctrl Pts',(-0.500000000056254,-2.44498872388035,
-20.0715359155249));
#18224=CARTESIAN_POINT('Ctrl Pts',(-0.500000000056255,-1.91832221676201,
-19.5511146046992));
#18225=CARTESIAN_POINT('Ctrl Pts',(-0.500000000109656,-1.62379237768017,
-19.3555089426616));
#18226=CARTESIAN_POINT('Ctrl Pts',(-0.500000000109656,-0.988284848212895,
-19.0845211957907));
#18227=CARTESIAN_POINT('Ctrl Pts',(-0.5,-0.647287344063983,-19.0078130433352));
#18228=CARTESIAN_POINT('Ctrl Pts',(-0.5,-0.285729446825272,-19.000186495383));
#18229=CARTESIAN_POINT('Ctrl Pts',(-0.500000469773922,-0.267871294986009,
-18.9999975511487));
#18230=CARTESIAN_POINT('Ctrl Pts',(-0.500000469773922,-0.250006335535676,
-18.9999974593238));
#18231=CARTESIAN_POINT('',(-0.5,-5.55111512312578E-17,-19.));
#18232=CARTESIAN_POINT('Origin',(-0.5,0.,0.));
#18233=CARTESIAN_POINT('',(-0.499999999999999,-2.95803989154981,-24.3207730140306));
#18234=CARTESIAN_POINT('',(-0.499999999999999,-2.95803989154981,-39.));
#18235=CARTESIAN_POINT('',(-0.500000000000001,2.95803989154981,-24.3207730140306));
#18236=CARTESIAN_POINT('Origin',(-0.5,0.,0.));
#18237=CARTESIAN_POINT('',(-0.500000000000001,2.95803989154981,-39.));
#18238=CARTESIAN_POINT('Origin',(0.,0.,-39.));
#18239=CARTESIAN_POINT('',(0.499940272430435,-2.95804998673149,-21.711522214267));
#18240=CARTESIAN_POINT('',(2.99999997687933,-0.000372456737699808,-21.7386095076915));
#18241=CARTESIAN_POINT('Ctrl Pts',(0.499940272430435,-2.95804998673149,
-21.711522214267));
#18242=CARTESIAN_POINT('Ctrl Pts',(0.590943823703178,-2.94266946901898,
-21.7128013793572));
#18243=CARTESIAN_POINT('Ctrl Pts',(0.681385576598305,-2.92306001474672,
-21.7140408866948));
#18244=CARTESIAN_POINT('Ctrl Pts',(0.770831732736946,-2.89927895170605,
-21.7152369587624));
#18245=CARTESIAN_POINT('Ctrl Pts',(0.860461624499595,-2.87544903884728,
-21.7164354877387));
#18246=CARTESIAN_POINT('Ctrl Pts',(0.949091358165715,-2.8474304009286,-21.7175904028168));
#18247=CARTESIAN_POINT('Ctrl Pts',(1.03629244274752,-2.81533265762758,-21.7186979031526));
#18248=CARTESIAN_POINT('Ctrl Pts',(1.12349352732932,-2.78323491432656,-21.7198054034884));
#18249=CARTESIAN_POINT('Ctrl Pts',(1.20926550868456,-2.74705819021273,-21.7208654890818));
#18250=CARTESIAN_POINT('Ctrl Pts',(1.29319479444907,-2.70696273036956,-21.7218743590889));
#18251=CARTESIAN_POINT('Ctrl Pts',(1.38514345926628,-2.66303618000959,-21.7229796258535));
#18252=CARTESIAN_POINT('Ctrl Pts',(1.47489868199608,-2.61439858546958,-21.7240234222307));
#18253=CARTESIAN_POINT('Ctrl Pts',(1.56199112027725,-2.56128556396491,-21.7250074208905));
#18254=CARTESIAN_POINT('Ctrl Pts',(1.64895180070953,-2.50825289452753,-21.7259899309072));
#18255=CARTESIAN_POINT('Ctrl Pts',(1.73325744965887,-2.45075848007837,-21.7269128239996));
#18256=CARTESIAN_POINT('Ctrl Pts',(1.81446485280803,-2.38908294077965,-21.7277777652573));
#18257=CARTESIAN_POINT('Ctrl Pts',(1.89558419876958,-2.3274742793064,-21.7286417686166));
#18258=CARTESIAN_POINT('Ctrl Pts',(1.97361172962793,-2.26169373032095,-21.7294479457531));
#18259=CARTESIAN_POINT('Ctrl Pts',(2.04813400568942,-2.19206457357866,-21.7301979563459));
#18260=CARTESIAN_POINT('Ctrl Pts',(2.12254107022213,-2.12254306359679,-21.7309468074213));
#18261=CARTESIAN_POINT('Ctrl Pts',(2.19345344471056,-2.04918503990753,-21.7316396654859));
#18262=CARTESIAN_POINT('Ctrl Pts',(2.26049198244141,-1.9723529089182,-21.7322781825327));
#18263=CARTESIAN_POINT('Ctrl Pts',(2.28763948139665,-1.94123945885854,-21.7325367523263));
#18264=CARTESIAN_POINT('Ctrl Pts',(2.31415211222994,-1.90955674624072,-21.7327864108756));
#18265=CARTESIAN_POINT('Ctrl Pts',(2.34000635954708,-1.87733061480369,-21.7330272678849));
#18266=CARTESIAN_POINT('Ctrl Pts',(2.39854660163678,-1.80436289260329,-21.7335726261566));
#18267=CARTESIAN_POINT('Ctrl Pts',(2.45373712959435,-1.72857119950941,-21.7340728608125));
#18268=CARTESIAN_POINT('Ctrl Pts',(2.50529507107785,-1.65030197443773,-21.7345302491155));
#18269=CARTESIAN_POINT('Ctrl Pts',(2.55682398716703,-1.57207681231841,-21.7349873799241));
#18270=CARTESIAN_POINT('Ctrl Pts',(2.60472412694322,-1.49137726307369,-21.7354017126085));
#18271=CARTESIAN_POINT('Ctrl Pts',(2.64875443563976,-1.40858082468799,-21.7357755205876));
#18272=CARTESIAN_POINT('Ctrl Pts',(2.69276900633143,-1.32581398070645,-21.7361491949543));
#18273=CARTESIAN_POINT('Ctrl Pts',(2.73291628446364,-1.24095213736414,-21.7364823735806));
#18274=CARTESIAN_POINT('Ctrl Pts',(2.76900059729431,-1.1543984113744,-21.7367773274486));
#18275=CARTESIAN_POINT('Ctrl Pts',(2.805096072164,-1.06781791153224,-21.7370723725553));
#18276=CARTESIAN_POINT('Ctrl Pts',(2.83712589208258,-0.979544899685551,
-21.7373291692517));
#18277=CARTESIAN_POINT('Ctrl Pts',(2.86494239747023,-0.890002842230036,
-21.737549990628));
#18278=CARTESIAN_POINT('Ctrl Pts',(2.88763517731577,-0.816954191134653,
-21.7377301373003));
#18279=CARTESIAN_POINT('Ctrl Pts',(2.90752472746022,-0.74306142296919,-21.737886341173));
#18280=CARTESIAN_POINT('Ctrl Pts',(2.92455565394967,-0.668561311287938,
-21.738019836408));
#18281=CARTESIAN_POINT('Ctrl Pts',(2.94760303630648,-0.567742805576745,
-21.738200491038));
#18282=CARTESIAN_POINT('Ctrl Pts',(2.96542043503695,-0.465786149542869,
-21.7383395586531));
#18283=CARTESIAN_POINT('Ctrl Pts',(2.97792997673742,-0.363225898923373,
-21.7384371460061));
#18284=CARTESIAN_POINT('Ctrl Pts',(2.99045332846363,-0.260552425954423,
-21.7385348410916));
#18285=CARTESIAN_POINT('Ctrl Pts',(2.99765708173621,-0.157274332776194,
-21.7385909642795));
#18286=CARTESIAN_POINT('Ctrl Pts',(2.99951519319889,-0.0539314914409496,
-21.7386056226765));
#18287=CARTESIAN_POINT('Ctrl Pts',(2.9998361735633,-0.0360794822708074,
-21.7386081548484));
#18288=CARTESIAN_POINT('Ctrl Pts',(2.99999776037856,-0.0182255429702799,
-21.7386094496693));
#18289=CARTESIAN_POINT('Ctrl Pts',(2.99999997687933,-0.000372456737699808,
-21.7386095076915));
#18290=CARTESIAN_POINT('',(0.500000000000001,-2.95803989154981,-24.3207730140306));
#18291=CARTESIAN_POINT('',(0.500000000000001,-2.95803989154981,-39.));
#18292=CARTESIAN_POINT('Ctrl Pts',(0.5,-2.95803989154981,-24.3207730140306));
#18293=CARTESIAN_POINT('Ctrl Pts',(0.331796881873696,-2.98647140773842,
-24.3173150006272));
#18294=CARTESIAN_POINT('Ctrl Pts',(0.163503365753253,-3.,-24.3156328315757));
#18295=CARTESIAN_POINT('Ctrl Pts',(6.93889390390723E-16,-3.,-24.3156328315757));
#18296=CARTESIAN_POINT('Ctrl Pts',(-0.163503365753251,-3.,-24.3156328315757));
#18297=CARTESIAN_POINT('Ctrl Pts',(-0.331796881873694,-2.98647140773842,
-24.3173150006272));
#18298=CARTESIAN_POINT('Ctrl Pts',(-0.499999999999998,-2.95803989154981,
-24.3207730140306));
#18299=CARTESIAN_POINT('',(0.499999999999999,2.95803989154981,-24.3207730140306));
#18300=CARTESIAN_POINT('Ctrl Pts',(-0.500000000000001,2.95803989154981,
-24.3207730140306));
#18301=CARTESIAN_POINT('Ctrl Pts',(-0.331796881873696,2.98647140773842,
-24.3173150006272));
#18302=CARTESIAN_POINT('Ctrl Pts',(-0.163503365753253,3.,-24.3156328315757));
#18303=CARTESIAN_POINT('Ctrl Pts',(0.163503365753251,3.,-24.3156328315757));
#18304=CARTESIAN_POINT('Ctrl Pts',(0.331796881873695,2.98647140773842,-24.3173150006272));
#18305=CARTESIAN_POINT('Ctrl Pts',(0.499999999999999,2.95803989154981,-24.3207730140306));
#18306=CARTESIAN_POINT('',(0.50001018530813,2.95803816990047,-21.711526659174));
#18307=CARTESIAN_POINT('',(0.499999999999999,2.95803989154981,-39.));
#18308=CARTESIAN_POINT('Ctrl Pts',(2.99999997687942,-0.00037245602236802,
-21.7386095076915));
#18309=CARTESIAN_POINT('Ctrl Pts',(3.0000127845348,0.102788624854442,-21.7386098429627));
#18310=CARTESIAN_POINT('Ctrl Pts',(2.99470015339322,0.205905039166103,-21.7385688825926));
#18311=CARTESIAN_POINT('Ctrl Pts',(2.984101926097,0.308440747412134,-21.7384867331043));
#18312=CARTESIAN_POINT('Ctrl Pts',(2.9734946788889,0.411063721483705,-21.7384045137005));
#18313=CARTESIAN_POINT('Ctrl Pts',(2.95759288398216,0.513104691368237,-21.7382810350385));
#18314=CARTESIAN_POINT('Ctrl Pts',(2.93648812652496,0.614033779834593,-21.7381164039139));
#18315=CARTESIAN_POINT('Ctrl Pts',(2.93249970587827,0.633107567396801,-21.7380852915841));
#18316=CARTESIAN_POINT('Ctrl Pts',(2.92832561220341,0.652141674306716,-21.738052709526));
#18317=CARTESIAN_POINT('Ctrl Pts',(2.92396666800349,0.671132568427846,-21.7380186584606));
#18318=CARTESIAN_POINT('Ctrl Pts',(2.90131380514578,0.769825761169153,-21.7378416995278));
#18319=CARTESIAN_POINT('Ctrl Pts',(2.87365847471177,0.867377264682175,-21.7376250664534));
#18320=CARTESIAN_POINT('Ctrl Pts',(2.84113991255455,0.963288117485888,-21.7373656504818));
#18321=CARTESIAN_POINT('Ctrl Pts',(2.80862455432068,1.05918952057843,-21.7371062600695));
#18322=CARTESIAN_POINT('Ctrl Pts',(2.77124703002945,1.1534502658333,-21.73680409519));
#18323=CARTESIAN_POINT('Ctrl Pts',(2.72919602839704,1.24558782852989,-21.7364560480066));
#18324=CARTESIAN_POINT('Ctrl Pts',(2.68715453496819,1.33770455788917,-21.7361080795205));
#18325=CARTESIAN_POINT('Ctrl Pts',(2.64044181798012,1.42769874705926,-21.735714249477));
#18326=CARTESIAN_POINT('Ctrl Pts',(2.58929405009832,1.51510934329026,-21.7352714521471));
#18327=CARTESIAN_POINT('Ctrl Pts',(2.53815579233109,1.60250368691006,-21.7348287371483));
#18328=CARTESIAN_POINT('Ctrl Pts',(2.48258430377546,1.68731509589525,-21.7343370730706));
#18329=CARTESIAN_POINT('Ctrl Pts',(2.42286088774972,1.7691085660899,-21.733793355917));
#18330=CARTESIAN_POINT('Ctrl Pts',(2.3964348284965,1.80530005066537,-21.7335527752088));
#18331=CARTESIAN_POINT('Ctrl Pts',(2.36919646981116,1.84090103915332,-21.7333020033804));
#18332=CARTESIAN_POINT('Ctrl Pts',(2.34117286728839,1.87587569030377,-21.7330407715356));
#18333=CARTESIAN_POINT('Ctrl Pts',(2.28254921400658,1.94904050988863,-21.7324942905796));
#18334=CARTESIAN_POINT('Ctrl Pts',(2.22046791995484,2.01948508884061,-21.7319020344294));
#18335=CARTESIAN_POINT('Ctrl Pts',(2.15522082010883,2.08686923801407,-21.7312628877286));
#18336=CARTESIAN_POINT('Ctrl Pts',(2.08995164894374,2.15427618141227,-21.7306235248219));
#18337=CARTESIAN_POINT('Ctrl Pts',(2.02151484114231,2.21862029555148,-21.7299372396356));
#18338=CARTESIAN_POINT('Ctrl Pts',(1.95024012850979,2.2795972102874,-21.7292029156811));
#18339=CARTESIAN_POINT('Ctrl Pts',(1.87895512064779,2.3405829327941,-21.7284684856577));
#18340=CARTESIAN_POINT('Ctrl Pts',(1.80483174370816,2.39820020280533,-21.7276860029873));
#18341=CARTESIAN_POINT('Ctrl Pts',(1.72823246505674,2.45218525946225,-21.7268543506973));
#18342=CARTESIAN_POINT('Ctrl Pts',(1.65154865351808,2.50622989256409,-21.7260217806185));
#18343=CARTESIAN_POINT('Ctrl Pts',(1.57238386054189,2.55663405610847,-21.7251399323357));
#18344=CARTESIAN_POINT('Ctrl Pts',(1.4911288350491,2.60317782667361,-21.7242076851744));
#18345=CARTESIAN_POINT('Ctrl Pts',(1.42637349841828,2.64027039433615,-21.7234647406195));
#18346=CARTESIAN_POINT('Ctrl Pts',(1.36029123456075,2.67491201703164,-21.7226897871063));
#18347=CARTESIAN_POINT('Ctrl Pts',(1.29308953927524,2.70701301131283,-21.7218822574094));
#18348=CARTESIAN_POINT('Ctrl Pts',(1.20152615241017,2.75075113050215,-21.7207819852553));
#18349=CARTESIAN_POINT('Ctrl Pts',(1.10784733971323,2.78978932872495,-21.7196212370477));
#18350=CARTESIAN_POINT('Ctrl Pts',(1.01254488240596,2.82396049213042,-21.7184045040822));
#18351=CARTESIAN_POINT('Ctrl Pts',(0.91697196252464,2.8582286312181,-21.7171843181026));
#18352=CARTESIAN_POINT('Ctrl Pts',(0.819766510469706,2.88760200735712,-21.7159078291516));
#18353=CARTESIAN_POINT('Ctrl Pts',(0.721435405590029,2.91196341933774,-21.7145795668714));
#18354=CARTESIAN_POINT('Ctrl Pts',(0.648180881864355,2.93011213874966,-21.7135900405069));
#18355=CARTESIAN_POINT('Ctrl Pts',(0.574301882693173,2.94548031795849,-21.7125717803367));
#18356=CARTESIAN_POINT('Ctrl Pts',(0.50001018530813,2.95803816990047,-21.711526659174));
#18357=CARTESIAN_POINT('',(3.,-3.67394039744206E-16,-31.));
#18358=CARTESIAN_POINT('',(3.,3.67394039744206E-16,-39.));
#18359=CARTESIAN_POINT('Origin',(0.,0.,-31.));
#18360=CARTESIAN_POINT('Ctrl Pts',(0.500000469469733,0.249901395253279,
-18.9999974609542));
#18361=CARTESIAN_POINT('Ctrl Pts',(0.499985448741165,0.249900114038217,
-18.9999972448598));
#18362=CARTESIAN_POINT('Ctrl Pts',(0.499957241892024,0.233340007311912,
-18.9999932538032));
#18363=CARTESIAN_POINT('Ctrl Pts',(0.499923116192456,0.161617649106977,
-18.999991205498));
#18364=CARTESIAN_POINT('Ctrl Pts',(0.499903664329549,0.0578515636974027,
-18.9999911080249));
#18365=CARTESIAN_POINT('Ctrl Pts',(0.499903654156312,-0.0575152632728968,
-18.9999911064299));
#18366=CARTESIAN_POINT('Ctrl Pts',(0.499923182383946,-0.161934911996989,
-18.9999912099571));
#18367=CARTESIAN_POINT('Ctrl Pts',(0.499957222601439,-0.2331464309115,-18.9999932557911));
#18368=CARTESIAN_POINT('Ctrl Pts',(0.499985489070265,-0.249900109125001,
-18.9999972525014));
#18369=CARTESIAN_POINT('Ctrl Pts',(0.500000469469733,-0.249901395253278,
-18.9999974609542));
#18370=CARTESIAN_POINT('Ctrl Pts',(0.500005900016648,1.07273098925591,-18.9999680907812));
#18371=CARTESIAN_POINT('Ctrl Pts',(0.617767041361557,1.05838429499492,-19.022282173232));
#18372=CARTESIAN_POINT('Ctrl Pts',(0.846046576080114,0.968758311001584,
-19.0545829182515));
#18373=CARTESIAN_POINT('Ctrl Pts',(1.12222781977421,0.664689166031461,-19.0711604080831));
#18374=CARTESIAN_POINT('Ctrl Pts',(1.27965290692711,0.238169452169252,-19.0719492566763));
#18375=CARTESIAN_POINT('Ctrl Pts',(1.27973523736976,-0.237098271262147,
-19.0719621646337));
#18376=CARTESIAN_POINT('Ctrl Pts',(1.12169212850501,-0.666446847723124,
-19.0711243191322));
#18377=CARTESIAN_POINT('Ctrl Pts',(0.846202696406831,-0.968026558196811,
-19.0545668296603));
#18378=CARTESIAN_POINT('Ctrl Pts',(0.617440655867346,-1.05842405813617,
-19.0222203277647));
#18379=CARTESIAN_POINT('Ctrl Pts',(0.500005900016646,-1.07273098925591,
-18.9999680907812));
#18380=CARTESIAN_POINT('Ctrl Pts',(0.374652474916355,2.49810289705817,-19.6779203934124));
#18381=CARTESIAN_POINT('Ctrl Pts',(0.709305752982863,2.46080584278846,-19.7142751509983));
#18382=CARTESIAN_POINT('Ctrl Pts',(1.35615168283393,2.24374271780176,-19.7670860721376));
#18383=CARTESIAN_POINT('Ctrl Pts',(2.1329201530783,1.53847021337198,-19.7950950890783));
#18384=CARTESIAN_POINT('Ctrl Pts',(2.57376683871501,0.551282961402653,-19.7975916138405));
#18385=CARTESIAN_POINT('Ctrl Pts',(2.57408967206061,-0.547867981449944,
-19.7976642591583));
#18386=CARTESIAN_POINT('Ctrl Pts',(2.13140251423125,-1.54147604638236,-19.7950284546789));
#18387=CARTESIAN_POINT('Ctrl Pts',(1.35656907690939,-2.24213495858108,-19.7670579619609));
#18388=CARTESIAN_POINT('Ctrl Pts',(0.708378231609485,-2.46090921489704,
-19.714174390549));
#18389=CARTESIAN_POINT('Ctrl Pts',(0.374652474916349,-2.49810289705816,
-19.6779203934123));
#18390=CARTESIAN_POINT('Ctrl Pts',(0.112199737628205,3.,-21.0973505959298));
#18391=CARTESIAN_POINT('Ctrl Pts',(0.545411427143746,2.98330034061039,-21.1128737181934));
#18392=CARTESIAN_POINT('Ctrl Pts',(1.40427349900891,2.76191133949964,-21.1369675122343));
#18393=CARTESIAN_POINT('Ctrl Pts',(2.44430058904568,1.90558580922904,-21.1529929864137));
#18394=CARTESIAN_POINT('Ctrl Pts',(3.02549037952742,0.682395833387457,-21.157041989878));
#18395=CARTESIAN_POINT('Ctrl Pts',(3.0259004610393,-0.678602295043218,-21.1570750782405));
#18396=CARTESIAN_POINT('Ctrl Pts',(2.44234453420329,-1.90963524646961,-21.1529563713896));
#18397=CARTESIAN_POINT('Ctrl Pts',(1.40492007795907,-2.75971795905596,-21.1369594501161));
#18398=CARTESIAN_POINT('Ctrl Pts',(0.544210742352774,-2.9833466252041,-21.1128306944771));
#18399=CARTESIAN_POINT('Ctrl Pts',(0.112199737628197,-3.,-21.0973505959298));
#18400=CARTESIAN_POINT('Ctrl Pts',(-1.54352792291549E-15,3.,-21.704163456598));
#18401=CARTESIAN_POINT('Ctrl Pts',(0.443076803624565,3.,-21.7109905340956));
#18402=CARTESIAN_POINT('Ctrl Pts',(1.33511706912935,2.80117039424009,-21.7230605835255));
#18403=CARTESIAN_POINT('Ctrl Pts',(2.4220516933108,1.94015762628841,-21.734095700974));
#18404=CARTESIAN_POINT('Ctrl Pts',(3.0250024087078,0.694486097636399,-21.7388012417923));
#18405=CARTESIAN_POINT('Ctrl Pts',(3.02547331281169,-0.690449402995863,
-21.7388112826209));
#18406=CARTESIAN_POINT('Ctrl Pts',(2.42004703065636,-1.94396691644154,-21.7340726461722));
#18407=CARTESIAN_POINT('Ctrl Pts',(1.33584761178912,-2.79884667955486,-21.7230617399995));
#18408=CARTESIAN_POINT('Ctrl Pts',(0.441848776790988,-3.,-21.7109716122421));
#18409=CARTESIAN_POINT('Ctrl Pts',(-1.02690891338221E-14,-3.,-21.704163456598));
#18410=CARTESIAN_POINT('',(0.500000234886957,-0.250003172328592,-18.999998729662));
#18411=CARTESIAN_POINT('Ctrl Pts',(0.500000469773915,-0.250006344657184,
-18.9999974593239));
#18412=CARTESIAN_POINT('Ctrl Pts',(0.500000469773915,-0.267897220477188,
-18.9999975513786));
#18413=CARTESIAN_POINT('Ctrl Pts',(0.5,-0.285781297573261,-19.0001870446798));
#18414=CARTESIAN_POINT('Ctrl Pts',(0.5,-0.647592139377092,-19.0078299813172));
#18415=CARTESIAN_POINT('Ctrl Pts',(0.500000000107083,-0.988819809921417,
-19.0846450518276));
#18416=CARTESIAN_POINT('Ctrl Pts',(0.500000000107083,-1.62420594756027,
-19.3558259127742));
#18417=CARTESIAN_POINT('Ctrl Pts',(0.500000000134817,-1.91845500253887,
-19.5513515847871));
#18418=CARTESIAN_POINT('Ctrl Pts',(0.500000000134817,-2.44454481720606,
-20.0714810657466));
#18419=CARTESIAN_POINT('Ctrl Pts',(0.499999999833624,-2.62276820685551,
-20.3702686628235));
#18420=CARTESIAN_POINT('Ctrl Pts',(0.499999999833624,-2.8108434657848,-20.8141963403292));
#18421=CARTESIAN_POINT('Ctrl Pts',(0.499999999999008,-2.86545068011728,
-20.9898853131812));
#18422=CARTESIAN_POINT('Ctrl Pts',(0.499999999999008,-2.93869493016462,
-21.34743767588));
#18423=CARTESIAN_POINT('Ctrl Pts',(0.500000000000001,-2.95754307939312,
-21.52946525912));
#18424=CARTESIAN_POINT('Ctrl Pts',(0.500000000000001,-2.95745543349273,
-21.7115181370337));
#18425=CARTESIAN_POINT('',(0.500000234886961,0.250003167767864,-18.9999987296619));
#18426=CARTESIAN_POINT('Ctrl Pts',(0.499999999999999,2.957907651092,-21.7115138352691));
#18427=CARTESIAN_POINT('Ctrl Pts',(0.499999999999999,2.95794618991124,-21.5294887787061));
#18428=CARTESIAN_POINT('Ctrl Pts',(0.499999999999071,2.93905776709014,-21.3474868610508));
#18429=CARTESIAN_POINT('Ctrl Pts',(0.499999999999071,2.86575493753945,-20.9899915011559));
#18430=CARTESIAN_POINT('Ctrl Pts',(0.499999999845862,2.81112639164981,-20.814326068996));
#18431=CARTESIAN_POINT('Ctrl Pts',(0.499999999845862,2.62297984800933,-20.3703581369862));
#18432=CARTESIAN_POINT('Ctrl Pts',(0.500000000064459,2.44467766128549,-20.071497650565));
#18433=CARTESIAN_POINT('Ctrl Pts',(0.500000000064459,1.91840198171423,-19.5512716141705));
#18434=CARTESIAN_POINT('Ctrl Pts',(0.500000000096094,1.6240590615628,-19.3557175409153));
#18435=CARTESIAN_POINT('Ctrl Pts',(0.500000000096094,0.988617937234748,
-19.0845954286414));
#18436=CARTESIAN_POINT('Ctrl Pts',(0.5,0.647452490142017,-19.007816540113));
#18437=CARTESIAN_POINT('Ctrl Pts',(0.5,0.285729437884547,-19.0001864952732));
#18438=CARTESIAN_POINT('Ctrl Pts',(0.500000469773922,0.267871290073013,
-18.9999975511486));
#18439=CARTESIAN_POINT('Ctrl Pts',(0.500000469773922,0.250006335535729,
-18.9999974593238));
#18440=CARTESIAN_POINT('',(0.5,1.66533453693773E-16,-19.));
#18441=CARTESIAN_POINT('Origin',(0.5,2.22044604925031E-16,0.));
#18442=CARTESIAN_POINT('Origin',(0.5,2.22044604925031E-16,0.));
#18443=CARTESIAN_POINT('Origin',(-0.5,0.,0.));
#18444=CARTESIAN_POINT('Ctrl Pts',(1.43046189829788,-2.88176118076299,-39.4132320681314));
#18445=CARTESIAN_POINT('Ctrl Pts',(2.37482146118144,-2.41299562794209,-39.3480377810873));
#18446=CARTESIAN_POINT('Ctrl Pts',(3.75195145870749,-0.483252427376924,
-39.2176492069991));
#18447=CARTESIAN_POINT('Ctrl Pts',(2.48093138115386,2.86039701702348,-39.0220663458667));
#18448=CARTESIAN_POINT('Ctrl Pts',(-1.00431634631447,3.64773132007517,-38.8264834847344));
#18449=CARTESIAN_POINT('Ctrl Pts',(-3.59288022276291,1.18807557140504,-38.6309006236019));
#18450=CARTESIAN_POINT('Ctrl Pts',(-2.98062062312938,-2.33209228359478,
-38.4353177624696));
#18451=CARTESIAN_POINT('Ctrl Pts',(0.288167629773712,-3.77318109983691,
-38.2397349013372));
#18452=CARTESIAN_POINT('Ctrl Pts',(3.29994356574598,-1.85236689627126,-38.0441520402049));
#18453=CARTESIAN_POINT('Ctrl Pts',(3.37118335473764,1.71935931877143,-37.8485691790725));
#18454=CARTESIAN_POINT('Ctrl Pts',(0.438236617843253,3.75881325515087,-37.6529863179401));
#18455=CARTESIAN_POINT('Ctrl Pts',(-2.88520346695894,2.44877028859547,-37.4574034568077));
#18456=CARTESIAN_POINT('Ctrl Pts',(-3.63759395527955,-1.04345151662343,
-37.2618205956754));
#18457=CARTESIAN_POINT('Ctrl Pts',(-1.14844282939652,-3.60581742991611,
-37.066237734543));
#18458=CARTESIAN_POINT('Ctrl Pts',(2.36410557671837,-2.95497314639522,-36.8706548734106));
#18459=CARTESIAN_POINT('Ctrl Pts',(3.76995295045892,0.329111973093684,-36.6750720122782));
#18460=CARTESIAN_POINT('Ctrl Pts',(1.8163171711215,3.3199167664903,-36.4794891511459));
#18461=CARTESIAN_POINT('Ctrl Pts',(-1.75587554620208,3.35227674819956,-36.2839062900135));
#18462=CARTESIAN_POINT('Ctrl Pts',(-3.76337186360745,0.397353826106389,
-36.0883234288811));
#18463=CARTESIAN_POINT('Ctrl Pts',(-2.41725037419006,-2.91165897783182,
-35.8927405677487));
#18464=CARTESIAN_POINT('Ctrl Pts',(1.08293233547133,-3.6260329995702,-35.6971577066164));
#18465=CARTESIAN_POINT('Ctrl Pts',(3.61809190721629,-1.10917474504408,-35.501574845484));
#18466=CARTESIAN_POINT('Ctrl Pts',(2.92909571917959,2.39609179780073,-35.3059919843517));
#18467=CARTESIAN_POINT('Ctrl Pts',(-0.370077606085909,3.76615190892214,
-35.1104091232193));
#18468=CARTESIAN_POINT('Ctrl Pts',(-3.33946720062995,1.78011698492664,-34.9148262620869));
#18469=CARTESIAN_POINT('Ctrl Pts',(-3.33298923708603,-1.79221664500977,
-34.7192434009545));
#18470=CARTESIAN_POINT('Ctrl Pts',(-0.356416329777662,-3.76746927984535,
-34.5236605398222));
#18471=CARTESIAN_POINT('Ctrl Pts',(2.93776641840763,-2.38545306342213,-34.3280776786898));
#18472=CARTESIAN_POINT('Ctrl Pts',(3.61404547698157,1.12228945489961,-34.1324948175575));
#18473=CARTESIAN_POINT('Ctrl Pts',(1.06977446774459,3.629936361797,-33.9369119564251));
#18474=CARTESIAN_POINT('Ctrl Pts',(-2.42779410945176,2.90287369715232,-33.7413290952927));
#18475=CARTESIAN_POINT('Ctrl Pts',(-3.76190637086622,-0.411001132144213,
-33.5457462341603));
#18476=CARTESIAN_POINT('Ctrl Pts',(-1.74370548238732,-3.35862046992087,
-33.350163373028));
#18477=CARTESIAN_POINT('Ctrl Pts',(1.82834428848415,-3.3133122421223,-33.1545805118956));
#18478=CARTESIAN_POINT('Ctrl Pts',(3.77112451550319,-0.315428059358477,
-32.9589976507632));
#18479=CARTESIAN_POINT('Ctrl Pts',(2.35336766298509,2.96350958546327,-32.7634147896309));
#18480=CARTESIAN_POINT('Ctrl Pts',(-1.16150178032287,3.60166451694395,-32.5678319284985));
#18481=CARTESIAN_POINT('Ctrl Pts',(-3.64137583224079,1.03018090832754,-32.3722490673661));
#18482=CARTESIAN_POINT('Ctrl Pts',(-2.8762608737732,-2.45907697744851,-32.1766662062337));
#18483=CARTESIAN_POINT('Ctrl Pts',(0.451781530523055,-3.75747883119848,
-31.9810833451013));
#18484=CARTESIAN_POINT('Ctrl Pts',(3.37756428501257,-1.70656712704126,-31.785500483969));
#18485=CARTESIAN_POINT('Ctrl Pts',(3.29287076467101,1.86322227179335,-31.5899176228366));
#18486=CARTESIAN_POINT('Ctrl Pts',(0.275155398406671,3.77639790272669,-31.3943347617042));
#18487=CARTESIAN_POINT('Ctrl Pts',(-2.99125666928477,2.31641984474353,-31.1987098698809));
#18488=CARTESIAN_POINT('Ctrl Pts',(-3.3857956881288,-0.0223753480619818,
-31.0682792651016));
#18489=CARTESIAN_POINT('Ctrl Pts',(-3.05040623055311,-1.02263886777266,
-31.0030429473666));
#18490=CARTESIAN_POINT('Ctrl Pts',(1.53694905724646,-3.0962866856177,-39.2749561275222));
#18491=CARTESIAN_POINT('Ctrl Pts',(2.55160910628562,-2.59262505343092,-39.2097618404781));
#18492=CARTESIAN_POINT('Ctrl Pts',(4.03125610277118,-0.519226945892664,
-39.0793732663898));
#18493=CARTESIAN_POINT('Ctrl Pts',(2.66561811390768,3.07333212013268,-38.8837904052575));
#18494=CARTESIAN_POINT('Ctrl Pts',(-1.07908016528225,3.91927755653543,-38.6882075441251));
#18495=CARTESIAN_POINT('Ctrl Pts',(-3.86034320644659,1.27651888636902,-38.4926246829927));
#18496=CARTESIAN_POINT('Ctrl Pts',(-3.20250547195918,-2.5056990619238,-38.2970418218604));
#18497=CARTESIAN_POINT('Ctrl Pts',(0.309619548368721,-4.05406613144679,
-38.1014589607279));
#18498=CARTESIAN_POINT('Ctrl Pts',(3.54559961252715,-1.99026171776147,-37.9058760995957));
#18499=CARTESIAN_POINT('Ctrl Pts',(3.62214266946524,1.84735272375873,-37.7102932384632));
#18500=CARTESIAN_POINT('Ctrl Pts',(0.47086004698659,4.03862870849191,-37.5147103773309));
#18501=CARTESIAN_POINT('Ctrl Pts',(-3.09998522420157,2.6310628692371,-37.3191275161985));
#18502=CARTESIAN_POINT('Ctrl Pts',(-3.9083855409675,-1.12112865548188,-37.1235446550661));
#18503=CARTESIAN_POINT('Ctrl Pts',(-1.2339357839889,-3.87424349163502,-36.9279617939337));
#18504=CARTESIAN_POINT('Ctrl Pts',(2.54009550460026,-3.17494873295464,-36.7323789328014));
#18505=CARTESIAN_POINT('Ctrl Pts',(4.05059767056079,0.353611890940086,-36.536796071669));
#18506=CARTESIAN_POINT('Ctrl Pts',(1.95152836097032,3.5670596682551,-36.3412132105366));
#18507=CARTESIAN_POINT('Ctrl Pts',(-1.88658731042651,3.60182860788203,-36.1456303494043));
#18508=CARTESIAN_POINT('Ctrl Pts',(-4.0435266711556,0.42693383805202,-35.9500474882719));
#18509=CARTESIAN_POINT('Ctrl Pts',(-2.59719653362373,-3.12841014942569,
-35.7544646271396));
#18510=CARTESIAN_POINT('Ctrl Pts',(1.1635485251616,-3.89596395882014,-35.5588817660071));
#18511=CARTESIAN_POINT('Ctrl Pts',(3.88743171170376,-1.19174448529219,-35.3632989048749));
#18512=CARTESIAN_POINT('Ctrl Pts',(3.14714492538008,2.57446285992508,-35.1677160437424));
#18513=CARTESIAN_POINT('Ctrl Pts',(-0.39762710804012,4.04651366999184,-34.9721331826101));
#18514=CARTESIAN_POINT('Ctrl Pts',(-3.58806548557568,1.91263334243781,-34.7765503214776));
#18515=CARTESIAN_POINT('Ctrl Pts',(-3.58110528623479,-1.92563373145894,
-34.5809674603453));
#18516=CARTESIAN_POINT('Ctrl Pts',(-0.382948852179039,-4.04792910929916,
-34.3853845992129));
#18517=CARTESIAN_POINT('Ctrl Pts',(3.15646109312986,-2.56303215156931,-34.1898017380806));
#18518=CARTESIAN_POINT('Ctrl Pts',(3.88308405508889,1.20583548692774,-33.9942188769482));
#18519=CARTESIAN_POINT('Ctrl Pts',(1.14941115287504,3.90015789708702,-33.7986360158158));
#18520=CARTESIAN_POINT('Ctrl Pts',(-2.6085251708909,3.11897087049483,-33.6030531546835));
#18521=CARTESIAN_POINT('Ctrl Pts',(-4.04195208347193,-0.44159708366083,
-33.4074702935511));
#18522=CARTESIAN_POINT('Ctrl Pts',(-1.873511276644,-3.60864457210354,-33.2118874324187));
#18523=CARTESIAN_POINT('Ctrl Pts',(1.96445080700954,-3.55996348658607,-33.0163045712863));
#18524=CARTESIAN_POINT('Ctrl Pts',(4.05185644983512,-0.338909312465405,
-32.820721710154));
#18525=CARTESIAN_POINT('Ctrl Pts',(2.52855823373077,3.18412064588255,-32.6251388490216));
#18526=CARTESIAN_POINT('Ctrl Pts',(-1.24796687586121,3.86978142544159,-32.4295559878892));
#18527=CARTESIAN_POINT('Ctrl Pts',(-3.912448950302,1.10687014993642,-32.2339731267569));
#18528=CARTESIAN_POINT('Ctrl Pts',(-3.09037692202834,-2.64213681376848,
-32.0383902656245));
#18529=CARTESIAN_POINT('Ctrl Pts',(0.485413276819888,-4.03719494668529,
-31.8428074044921));
#18530=CARTESIAN_POINT('Ctrl Pts',(3.62899861213807,-1.83360824930386,-31.6472245433597));
#18531=CARTESIAN_POINT('Ctrl Pts',(3.53800029446268,2.00192519456892,-31.4516416822274));
#18532=CARTESIAN_POINT('Ctrl Pts',(0.295638653976472,4.05752240118364,-31.256058821095));
#18533=CARTESIAN_POINT('Ctrl Pts',(-3.21393329197368,2.48885992755341,-31.0604339292716));
#18534=CARTESIAN_POINT('Ctrl Pts',(-3.63784278147551,-0.0240410248957648,
-30.9300033244924));
#18535=CARTESIAN_POINT('Ctrl Pts',(-3.27748609441888,-1.09876666103236,
-30.8647670067574));
#18536=CARTESIAN_POINT('Ctrl Pts',(1.64343621619505,-3.3108121904724,-39.136680186913));
#18537=CARTESIAN_POINT('Ctrl Pts',(2.7283967513898,-2.77225447891975,-39.0714858998688));
#18538=CARTESIAN_POINT('Ctrl Pts',(4.31056074683487,-0.555201464408408,
-38.9410973257805));
#18539=CARTESIAN_POINT('Ctrl Pts',(2.8503048466615,3.28626722324188,-38.7455144646482));
#18540=CARTESIAN_POINT('Ctrl Pts',(-1.15384398425004,4.19082379299567,-38.5499316035159));
#18541=CARTESIAN_POINT('Ctrl Pts',(-4.12780619013028,1.36496220133301,-38.3543487423834));
#18542=CARTESIAN_POINT('Ctrl Pts',(-3.42439032078898,-2.67930584025284,
-38.1587658812511));
#18543=CARTESIAN_POINT('Ctrl Pts',(0.331071466963731,-4.33495116305667,
-37.9631830201187));
#18544=CARTESIAN_POINT('Ctrl Pts',(3.79125565930832,-2.12815653925168,-37.7676001589864));
#18545=CARTESIAN_POINT('Ctrl Pts',(3.87310198419283,1.97534612874602,-37.572017297854));
#18546=CARTESIAN_POINT('Ctrl Pts',(0.503483476129927,4.31844416183293,-37.3764344367216));
#18547=CARTESIAN_POINT('Ctrl Pts',(-3.31476698144421,2.81335544987872,-37.1808515755893));
#18548=CARTESIAN_POINT('Ctrl Pts',(-4.17917712665544,-1.19880579434034,
-36.9852687144569));
#18549=CARTESIAN_POINT('Ctrl Pts',(-1.31942873858128,-4.14266955335393,
-36.7896858533245));
#18550=CARTESIAN_POINT('Ctrl Pts',(2.71608543248216,-3.39492431951407,-36.5941029921921));
#18551=CARTESIAN_POINT('Ctrl Pts',(4.33124239066266,0.378111808786486,-36.3985201310598));
#18552=CARTESIAN_POINT('Ctrl Pts',(2.08673955081914,3.8142025700199,-36.2029372699274));
#18553=CARTESIAN_POINT('Ctrl Pts',(-2.01729907465095,3.85138046756452,-36.007354408795));
#18554=CARTESIAN_POINT('Ctrl Pts',(-4.32368147870374,0.456513849997653,
-35.8117715476627));
#18555=CARTESIAN_POINT('Ctrl Pts',(-2.7771426930574,-3.34516132101955,-35.6161886865303));
#18556=CARTESIAN_POINT('Ctrl Pts',(1.24416471485188,-4.16589491807009,-35.4206058253979));
#18557=CARTESIAN_POINT('Ctrl Pts',(4.15677151619123,-1.2743142255403,-35.2250229642655));
#18558=CARTESIAN_POINT('Ctrl Pts',(3.36519413158057,2.75283392204944,-35.0294401031332));
#18559=CARTESIAN_POINT('Ctrl Pts',(-0.42517660999433,4.32687543106154,-34.8338572420008));
#18560=CARTESIAN_POINT('Ctrl Pts',(-3.83666377052141,2.04514969994899,-34.6382743808684));
#18561=CARTESIAN_POINT('Ctrl Pts',(-3.82922133538355,-2.05905081790811,
-34.442691519736));
#18562=CARTESIAN_POINT('Ctrl Pts',(-0.409481374580417,-4.32838893875298,
-34.2471086586037));
#18563=CARTESIAN_POINT('Ctrl Pts',(3.37515576785208,-2.7406112397165,-34.0515257974713));
#18564=CARTESIAN_POINT('Ctrl Pts',(4.1521226331962,1.28938151895587,-33.855942936339));
#18565=CARTESIAN_POINT('Ctrl Pts',(1.22904783800549,4.17037943237703,-33.6603600752066));
#18566=CARTESIAN_POINT('Ctrl Pts',(-2.78925623233004,3.33506804383733,-33.4647772140742));
#18567=CARTESIAN_POINT('Ctrl Pts',(-4.32199779607761,-0.472193035177443,
-33.2691943529418));
#18568=CARTESIAN_POINT('Ctrl Pts',(-2.0033170709007,-3.8586686742862,-33.0736114918095));
#18569=CARTESIAN_POINT('Ctrl Pts',(2.10055732553492,-3.80661473104982,-32.8780286306771));
#18570=CARTESIAN_POINT('Ctrl Pts',(4.33258838416705,-0.362390565572336,
-32.6824457695447));
#18571=CARTESIAN_POINT('Ctrl Pts',(2.70374880447645,3.40473170630184,-32.4868629084123));
#18572=CARTESIAN_POINT('Ctrl Pts',(-1.33443197139957,4.13789833393923,-32.29128004728));
#18573=CARTESIAN_POINT('Ctrl Pts',(-4.1835220683632,1.18355939154531,-32.0956971861476));
#18574=CARTESIAN_POINT('Ctrl Pts',(-3.30449297028347,-2.82519665008844,
-31.9001143250153));
#18575=CARTESIAN_POINT('Ctrl Pts',(0.519045023116724,-4.31691106217212,
-31.7045314638828));
#18576=CARTESIAN_POINT('Ctrl Pts',(3.88043293926357,-1.96064937156648,-31.5089486027505));
#18577=CARTESIAN_POINT('Ctrl Pts',(3.78312982425436,2.14062811734448,-31.3133657416181));
#18578=CARTESIAN_POINT('Ctrl Pts',(0.316121909546268,4.33864689964057,-31.1177828804858));
#18579=CARTESIAN_POINT('Ctrl Pts',(-3.43660991466259,2.66130001036329,-30.9221579886624));
#18580=CARTESIAN_POINT('Ctrl Pts',(-3.88988987482222,-0.0257067017295483,
-30.7917273838832));
#18581=CARTESIAN_POINT('Ctrl Pts',(-3.50456595828466,-1.17489445429207,
-30.7264910661481));
#18582=CARTESIAN_POINT('Ctrl Pts',(1.74992337514364,-3.52533769532709,-38.9984042463037));
#18583=CARTESIAN_POINT('Ctrl Pts',(2.90518439649398,-2.95188390440858,-38.9332099592596));
#18584=CARTESIAN_POINT('Ctrl Pts',(4.58986539089856,-0.591175982924146,
-38.8028213851713));
#18585=CARTESIAN_POINT('Ctrl Pts',(3.03499157941532,3.49920232635108,-38.607238524039));
#18586=CARTESIAN_POINT('Ctrl Pts',(-1.22860780321782,4.46237002945592,-38.4116556629066));
#18587=CARTESIAN_POINT('Ctrl Pts',(-4.39526917381396,1.45340551629699,-38.2160728017742));
#18588=CARTESIAN_POINT('Ctrl Pts',(-3.64627516961878,-2.85291261858187,
-38.0204899406419));
#18589=CARTESIAN_POINT('Ctrl Pts',(0.352523385558738,-4.61583619466654,
-37.8249070795095));
#18590=CARTESIAN_POINT('Ctrl Pts',(4.0369117060895,-2.26605136074189,-37.6293242183772));
#18591=CARTESIAN_POINT('Ctrl Pts',(4.12406129892043,2.10333953373333,-37.4337413572447));
#18592=CARTESIAN_POINT('Ctrl Pts',(0.536106905273268,4.59825961517397,-37.2381584961124));
#18593=CARTESIAN_POINT('Ctrl Pts',(-3.52954873868685,2.99564803052035,-37.04257563498));
#18594=CARTESIAN_POINT('Ctrl Pts',(-4.44996871234337,-1.2764829331988,-36.8469927738476));
#18595=CARTESIAN_POINT('Ctrl Pts',(-1.40492169317366,-4.41109561507284,
-36.6514099127152));
#18596=CARTESIAN_POINT('Ctrl Pts',(2.89207536036405,-3.6148999060735,-36.4558270515829));
#18597=CARTESIAN_POINT('Ctrl Pts',(4.61188711076453,0.402611726632887,-36.2602441904505));
#18598=CARTESIAN_POINT('Ctrl Pts',(2.22195074066797,4.06134547178471,-36.0646613293182));
#18599=CARTESIAN_POINT('Ctrl Pts',(-2.14801083887538,4.100932327247,-35.8690784681858));
#18600=CARTESIAN_POINT('Ctrl Pts',(-4.60383628625188,0.486093861943285,
-35.6734956070534));
#18601=CARTESIAN_POINT('Ctrl Pts',(-2.95708885249107,-3.56191249261342,
-35.4779127459211));
#18602=CARTESIAN_POINT('Ctrl Pts',(1.32478090454216,-4.43582587732003,-35.2823298847886));
#18603=CARTESIAN_POINT('Ctrl Pts',(4.42611132067871,-1.3568839657884,-35.0867470236564));
#18604=CARTESIAN_POINT('Ctrl Pts',(3.58324333778105,2.93120498417377,-34.8911641625239));
#18605=CARTESIAN_POINT('Ctrl Pts',(-0.45272611194854,4.60723719213125,-34.6955813013916));
#18606=CARTESIAN_POINT('Ctrl Pts',(-4.08526205546715,2.17766605746016,-34.4999984402592));
#18607=CARTESIAN_POINT('Ctrl Pts',(-4.07733738453231,-2.19246790435728,
-34.3044155791268));
#18608=CARTESIAN_POINT('Ctrl Pts',(-0.436013896981797,-4.60884876820679,
-34.1088327179944));
#18609=CARTESIAN_POINT('Ctrl Pts',(3.5938504425743,-2.91819032786367,-33.913249856862));
#18610=CARTESIAN_POINT('Ctrl Pts',(4.42116121130352,1.37292755098399,-33.7176669957297));
#18611=CARTESIAN_POINT('Ctrl Pts',(1.30868452313593,4.44060096766705,-33.5220841345973));
#18612=CARTESIAN_POINT('Ctrl Pts',(-2.96998729376919,3.55116521717984,-33.326501273465));
#18613=CARTESIAN_POINT('Ctrl Pts',(-4.60204350868331,-0.502788986694056,
-33.1309184123326));
#18614=CARTESIAN_POINT('Ctrl Pts',(-2.1331228651574,-4.10869277646887,-32.9353355512002));
#18615=CARTESIAN_POINT('Ctrl Pts',(2.23666384406031,-4.05326597551358,-32.7397526900678));
#18616=CARTESIAN_POINT('Ctrl Pts',(4.61332031849898,-0.385871818679268,
-32.5441698289355));
#18617=CARTESIAN_POINT('Ctrl Pts',(2.87893937522212,3.62534276672113,-32.3485869678031));
#18618=CARTESIAN_POINT('Ctrl Pts',(-1.42089706693793,4.40601524243686,-32.1530041066707));
#18619=CARTESIAN_POINT('Ctrl Pts',(-4.45459518642441,1.26024863315421,-31.9574212455384));
#18620=CARTESIAN_POINT('Ctrl Pts',(-3.51860901853861,-3.00825648640842,
-31.761838384406));
#18621=CARTESIAN_POINT('Ctrl Pts',(0.552676769413556,-4.59662717765893,
-31.5662555232737));
#18622=CARTESIAN_POINT('Ctrl Pts',(4.13186726638907,-2.08769049382909,-31.3706726621412));
#18623=CARTESIAN_POINT('Ctrl Pts',(4.02825935404604,2.27933104012005,-31.1750898010089));
#18624=CARTESIAN_POINT('Ctrl Pts',(0.336605165116067,4.61977139809752,-30.9795069398765));
#18625=CARTESIAN_POINT('Ctrl Pts',(-3.6592865373515,2.83374009317316,-30.7838820480532));
#18626=CARTESIAN_POINT('Ctrl Pts',(-4.14193696816894,-0.0273723785633317,
-30.653451443274));
#18627=CARTESIAN_POINT('Ctrl Pts',(-3.73164582215044,-1.25102224755177,
-30.5882151255389));
#18628=CARTESIAN_POINT('Ctrl Pts',(0.65442808399584,3.88366537266789,-31.));
#18629=CARTESIAN_POINT('Ctrl Pts',(0.530799992980382,3.89427684154009,-31.));
#18630=CARTESIAN_POINT('Ctrl Pts',(0.407028067198408,3.89867666407562,-31.));
#18631=CARTESIAN_POINT('Ctrl Pts',(0.283462307316361,3.89662818837984,-31.));
#18632=CARTESIAN_POINT('Ctrl Pts',(0.162992985921285,3.89463104550466,-31.));
#18633=CARTESIAN_POINT('Ctrl Pts',(0.0427188591126211,3.8865043164729,-31.));
#18634=CARTESIAN_POINT('Ctrl Pts',(-0.076989455381779,3.87248877284768,
-31.));
#18635=CARTESIAN_POINT('Ctrl Pts',(-0.1982861832848,3.85828725653111,-31.));
#18636=CARTESIAN_POINT('Ctrl Pts',(-0.319002835924176,3.83803917771155,
-31.));
#18637=CARTESIAN_POINT('Ctrl Pts',(-0.438735032843909,3.81194478664408,
-31.));
#18638=CARTESIAN_POINT('Ctrl Pts',(-0.558467229763642,3.78585039557661,
-31.));
#18639=CARTESIAN_POINT('Ctrl Pts',(-0.677215788457317,3.75390915529031,
-31.));
#18640=CARTESIAN_POINT('Ctrl Pts',(-0.794545113588183,3.71627889103425,
-31.));
#18641=CARTESIAN_POINT('Ctrl Pts',(-0.814657844220622,3.70982826696592,
-31.));
#18642=CARTESIAN_POINT('Ctrl Pts',(-0.83473197297741,3.70320920941588,-31.));
#18643=CARTESIAN_POINT('Ctrl Pts',(-0.854740931745014,3.69643088850593,
-31.));
#18644=CARTESIAN_POINT('Ctrl Pts',(-0.968165833818036,3.65800658095652,
-31.));
#18645=CARTESIAN_POINT('Ctrl Pts',(-1.07965301146909,3.61442076053118,-31.));
#18646=CARTESIAN_POINT('Ctrl Pts',(-1.18884413184658,3.56590670523799,-31.));
#18647=CARTESIAN_POINT('Ctrl Pts',(-1.29790943786314,3.51744854977294,-31.));
#18648=CARTESIAN_POINT('Ctrl Pts',(-1.4046847353241,3.46407295073166,-31.));
#18649=CARTESIAN_POINT('Ctrl Pts',(-1.50878571903602,3.4059682136783,-31.));
#18650=CARTESIAN_POINT('Ctrl Pts',(-1.61069021754416,3.34908946115127,-31.));
#18651=CARTESIAN_POINT('Ctrl Pts',(-1.71003263238448,3.28767841965964,-31.));
#18652=CARTESIAN_POINT('Ctrl Pts',(-1.80641677157113,3.2218782094244,-31.));
#18653=CARTESIAN_POINT('Ctrl Pts',(-1.8932173104265,3.16262059968267,-31.));
#18654=CARTESIAN_POINT('Ctrl Pts',(-1.97761850464391,3.09980260999695,-31.));
#18655=CARTESIAN_POINT('Ctrl Pts',(-2.05929965551334,3.03351053092812,-31.));
#18656=CARTESIAN_POINT('Ctrl Pts',(-2.07743120272542,3.01879504334464,-31.));
#18657=CARTESIAN_POINT('Ctrl Pts',(-2.0954329855743,3.00390448148057,-31.));
#18658=CARTESIAN_POINT('Ctrl Pts',(-2.11327637207231,2.9888610591179,-31.));
#18659=CARTESIAN_POINT('Ctrl Pts',(-2.2012290911024,2.91470978181062,-31.));
#18660=CARTESIAN_POINT('Ctrl Pts',(-2.28543470612264,2.83677091891449,-31.));
#18661=CARTESIAN_POINT('Ctrl Pts',(-2.36554425549263,2.75521673120583,-31.));
#18662=CARTESIAN_POINT('Ctrl Pts',(-2.44359400126818,2.67575949211696,-31.));
#18663=CARTESIAN_POINT('Ctrl Pts',(-2.5177560405726,2.59286986985704,-31.));
#18664=CARTESIAN_POINT('Ctrl Pts',(-2.58766793658226,2.50667951356563,-31.));
#18665=CARTESIAN_POINT('Ctrl Pts',(-2.65718277945497,2.42097866125412,-31.));
#18666=CARTESIAN_POINT('Ctrl Pts',(-2.72249613097522,2.3320140186649,-31.));
#18667=CARTESIAN_POINT('Ctrl Pts',(-2.7832047862205,2.23989471833288,-31.));
#18668=CARTESIAN_POINT('Ctrl Pts',(-2.7947489485025,2.22237760898432,-31.));
#18669=CARTESIAN_POINT('Ctrl Pts',(-2.80612645692971,2.20474638032351,-31.));
#18670=CARTESIAN_POINT('Ctrl Pts',(-2.81733432202403,2.18700171933814,-31.));
#18671=CARTESIAN_POINT('Ctrl Pts',(-2.8680715957088,2.10667279734618,-31.));
#18672=CARTESIAN_POINT('Ctrl Pts',(-2.91533425130486,2.02401925455049,-31.));
#18673=CARTESIAN_POINT('Ctrl Pts',(-2.95906936290355,1.93927703870198,-31.));
#18674=CARTESIAN_POINT('Ctrl Pts',(-2.96640259530189,1.9250679892666,-31.));
#18675=CARTESIAN_POINT('Ctrl Pts',(-2.97363186370474,1.91080938650722,-31.));
#18676=CARTESIAN_POINT('Ctrl Pts',(-2.98075699694485,1.89650307013396,-31.));
#18677=CARTESIAN_POINT('Ctrl Pts',(-3.03037412840343,1.79687849382657,-31.));
#18678=CARTESIAN_POINT('Ctrl Pts',(-3.07495051482241,1.69493226765915,-31.));
#18679=CARTESIAN_POINT('Ctrl Pts',(-3.11450209358653,1.59107365622641,-31.));
#18680=CARTESIAN_POINT('Ctrl Pts',(-3.15440656891242,1.48628837263471,-31.));
#18681=CARTESIAN_POINT('Ctrl Pts',(-3.18919620871934,1.37955547585428,-31.));
#18682=CARTESIAN_POINT('Ctrl Pts',(-3.21883515641334,1.27128356748666,-31.));
#18683=CARTESIAN_POINT('Ctrl Pts',(-3.24825524174243,1.16381116948505,-31.));
#18684=CARTESIAN_POINT('Ctrl Pts',(-3.27260033027765,1.05482148127186,-31.));
#18685=CARTESIAN_POINT('Ctrl Pts',(-3.29178473526898,0.944716681198161,
-31.));
#18686=CARTESIAN_POINT('Ctrl Pts',(-3.30603349555463,0.862938961052112,
-31.));
#18687=CARTESIAN_POINT('Ctrl Pts',(-3.31743436418504,0.780546081363158,
-31.));
#18688=CARTESIAN_POINT('Ctrl Pts',(-3.32593436134209,0.697708237182895,
-31.));
#18689=CARTESIAN_POINT('Ctrl Pts',(-3.32858825065657,0.671844408590687,
-31.));
#18690=CARTESIAN_POINT('Ctrl Pts',(-3.33095964050156,0.645930844620501,
-31.));
#18691=CARTESIAN_POINT('Ctrl Pts',(-3.33304413859681,0.620008089466332,
-31.));
#18692=CARTESIAN_POINT('Ctrl Pts',(-3.34186404098015,0.510324050662291,
-31.));
#18693=CARTESIAN_POINT('Ctrl Pts',(-3.34556409252275,0.400379798786449,
-31.));
#18694=CARTESIAN_POINT('Ctrl Pts',(-3.34408794001819,0.290567571373062,
-31.));
#18695=CARTESIAN_POINT('Ctrl Pts',(-3.34264022976402,0.182871186908495,
-31.));
#18696=CARTESIAN_POINT('Ctrl Pts',(-3.33621365424332,0.0753010039520607,
-31.));
#18697=CARTESIAN_POINT('Ctrl Pts',(-3.3247077506334,-0.0317580568508979,
-31.));
#18698=CARTESIAN_POINT('Ctrl Pts',(-3.31869249632875,-0.0877282351333704,
-31.));
#18699=CARTESIAN_POINT('Ctrl Pts',(-3.3112882052149,-0.143558394636405,
-31.));
#18700=CARTESIAN_POINT('Ctrl Pts',(-3.30247549609232,-0.199190797499773,
-31.));
#18701=CARTESIAN_POINT('Ctrl Pts',(-3.29984045792571,-0.215825126717531,
-31.));
#18702=CARTESIAN_POINT('Ctrl Pts',(-3.29707959885014,-0.232440680412909,
-31.));
#18703=CARTESIAN_POINT('Ctrl Pts',(-3.29419424747565,-0.249026088786987,
-31.));
#18704=CARTESIAN_POINT('Ctrl Pts',(-3.27606532868822,-0.353233681709253,
-31.));
#18705=CARTESIAN_POINT('Ctrl Pts',(-3.2530091964803,-0.456358937838572,
-31.));
#18706=CARTESIAN_POINT('Ctrl Pts',(-3.22494481912661,-0.558036044516438,
-31.));
#18707=CARTESIAN_POINT('Ctrl Pts',(-3.1976427103111,-0.656951455878645,
-31.));
#18708=CARTESIAN_POINT('Ctrl Pts',(-3.16560046250666,-0.754496902145692,
-31.));
#18709=CARTESIAN_POINT('Ctrl Pts',(-3.12870144491393,-0.850310755848633,
-31.));
#18710=CARTESIAN_POINT('Ctrl Pts',(-3.10634825322454,-0.908354182965307,
-31.));
#18711=CARTESIAN_POINT('Ctrl Pts',(-3.08221189711736,-0.965761619215496,
-31.));
#18712=CARTESIAN_POINT('Ctrl Pts',(-3.05625919777042,-1.02244671183575,
-31.));
#18713=CARTESIAN_POINT('',(1.87402501333402,2.62458822954938,-39.0012934619393));
#18714=CARTESIAN_POINT('Ctrl Pts',(1.87544346703979,2.62635034242884,-39.));
#18715=CARTESIAN_POINT('Ctrl Pts',(1.96556023181235,2.57633844914819,-39.));
#18716=CARTESIAN_POINT('Ctrl Pts',(2.05286117778038,2.52194281889414,-39.));
#18717=CARTESIAN_POINT('Ctrl Pts',(2.13698205793886,2.46326372726737,-39.));
#18718=CARTESIAN_POINT('Ctrl Pts',(2.22110684510665,2.40458191027971,-39.));
#18719=CARTESIAN_POINT('Ctrl Pts',(2.30205267959337,2.34161687861634,-39.));
#18720=CARTESIAN_POINT('Ctrl Pts',(2.37974275969731,2.27476660503621,-39.));
#18721=CARTESIAN_POINT('Ctrl Pts',(2.45973180397527,2.20593813316127,-39.));
#18722=CARTESIAN_POINT('Ctrl Pts',(2.53627010144683,2.13299070404304,-39.));
#18723=CARTESIAN_POINT('Ctrl Pts',(2.60925066612413,2.05630756533797,-39.));
#18724=CARTESIAN_POINT('Ctrl Pts',(2.6744743326814,1.98777486089014,-39.));
#18725=CARTESIAN_POINT('Ctrl Pts',(2.73685627038916,1.91625734338406,-39.));
#18726=CARTESIAN_POINT('Ctrl Pts',(2.79629976611078,1.84199988886912,-39.));
#18727=CARTESIAN_POINT('Ctrl Pts',(2.80703184372368,1.82859326202935,-39.));
#18728=CARTESIAN_POINT('Ctrl Pts',(2.81766808406566,1.81509726340499,-39.));
#18729=CARTESIAN_POINT('Ctrl Pts',(2.82820784020875,1.80151325565358,-39.));
#18730=CARTESIAN_POINT('Ctrl Pts',(2.83770979103154,1.78926680783468,-39.));
#18731=CARTESIAN_POINT('Ctrl Pts',(2.84712744324627,1.77695639545417,-39.));
#18732=CARTESIAN_POINT('Ctrl Pts',(2.85645967612864,1.76458452012062,-39.));
#18733=CARTESIAN_POINT('Ctrl Pts',(2.92213524453377,1.67751747464407,-39.));
#18734=CARTESIAN_POINT('Ctrl Pts',(2.98359709732638,1.58739136414667,-39.));
#18735=CARTESIAN_POINT('Ctrl Pts',(3.04075842469254,1.49464028713778,-39.));
#18736=CARTESIAN_POINT('Ctrl Pts',(3.09884554061698,1.40038700768156,-39.));
#18737=CARTESIAN_POINT('Ctrl Pts',(3.15249224301479,1.30342243618241,-39.));
#18738=CARTESIAN_POINT('Ctrl Pts',(3.20157784681904,1.20415578313502,-39.));
#18739=CARTESIAN_POINT('Ctrl Pts',(3.25108154673065,1.10404360720491,-39.));
#18740=CARTESIAN_POINT('Ctrl Pts',(3.29594667342186,1.00158923234391,-39.));
#18741=CARTESIAN_POINT('Ctrl Pts',(3.33601128466594,0.89717595563536,-39.));
#18742=CARTESIAN_POINT('Ctrl Pts',(3.36918521344763,0.810720640137817,-39.));
#18743=CARTESIAN_POINT('Ctrl Pts',(3.39906735707174,0.722921418403139,-39.));
#18744=CARTESIAN_POINT('Ctrl Pts',(3.42554208875469,0.633982806809461,-39.));
#18745=CARTESIAN_POINT('Ctrl Pts',(3.42999792814444,0.619013961287074,-39.));
#18746=CARTESIAN_POINT('Ctrl Pts',(3.4343566153323,0.604014581578844,-39.));
#18747=CARTESIAN_POINT('Ctrl Pts',(3.4386145432116,0.588996991314884,-39.));
#18748=CARTESIAN_POINT('Ctrl Pts',(3.46996387338543,0.478428797361006,-39.));
#18749=CARTESIAN_POINT('Ctrl Pts',(3.49590482509719,0.366708654043199,-39.));
#18750=CARTESIAN_POINT('Ctrl Pts',(3.51631639386122,0.254269119245185,-39.));
#18751=CARTESIAN_POINT('Ctrl Pts',(3.53705216924863,0.140043654010752,-39.));
#18752=CARTESIAN_POINT('Ctrl Pts',(3.5520821545375,0.025074956185946,-39.));
#18753=CARTESIAN_POINT('Ctrl Pts',(3.56123498540351,-0.0902151504387328,
-39.));
#18754=CARTESIAN_POINT('Ctrl Pts',(3.57038781626952,-0.205505257063412,
-39.));
#18755=CARTESIAN_POINT('Ctrl Pts',(3.57366404579988,-0.321117698045253,
-39.));
#18756=CARTESIAN_POINT('Ctrl Pts',(3.57083933718373,-0.436648879008429,
-39.));
#18757=CARTESIAN_POINT('Ctrl Pts',(3.57067942988942,-0.443189121230482,
-39.));
#18758=CARTESIAN_POINT('Ctrl Pts',(3.57049995539871,-0.449729105665625,
-39.));
#18759=CARTESIAN_POINT('Ctrl Pts',(3.57030086735777,-0.456268759879904,
-39.));
#18760=CARTESIAN_POINT('Ctrl Pts',(3.56748577448715,-0.548739075365919,
-39.));
#18761=CARTESIAN_POINT('Ctrl Pts',(3.56075124083497,-0.641143385283898,
-39.));
#18762=CARTESIAN_POINT('Ctrl Pts',(3.55021768944235,-0.733320321140995,
-39.));
#18763=CARTESIAN_POINT('Ctrl Pts',(3.54828067526101,-0.75027073276307,-39.));
#18764=CARTESIAN_POINT('Ctrl Pts',(3.54621613084359,-0.767204492865389,
-39.));
#18765=CARTESIAN_POINT('Ctrl Pts',(3.54402575312891,-0.784116253844053,
-39.));
#18766=CARTESIAN_POINT('Ctrl Pts',(3.52956892168877,-0.895736490018808,
-39.));
#18767=CARTESIAN_POINT('Ctrl Pts',(3.50962805978994,-1.00645761926625,-39.));
#18768=CARTESIAN_POINT('Ctrl Pts',(3.48451903279364,-1.11598728492715,-39.));
#18769=CARTESIAN_POINT('Ctrl Pts',(3.45894659598721,-1.22753841966266,-39.));
#18770=CARTESIAN_POINT('Ctrl Pts',(3.42801334193673,-1.3378543461902,-39.));
#18771=CARTESIAN_POINT('Ctrl Pts',(3.3919981550628,-1.44663447817002,-39.));
#18772=CARTESIAN_POINT('Ctrl Pts',(3.35525611427244,-1.5576099969248,-39.));
#18773=CARTESIAN_POINT('Ctrl Pts',(3.31322480411686,-1.66698785775475,-39.));
#18774=CARTESIAN_POINT('Ctrl Pts',(3.26614584317667,-1.77444675519679,-39.));
#18775=CARTESIAN_POINT('Ctrl Pts',(3.22751572378073,-1.86262096200685,-39.));
#18776=CARTESIAN_POINT('Ctrl Pts',(3.18548600942944,-1.94950332129944,-39.));
#18777=CARTESIAN_POINT('Ctrl Pts',(3.14016485218617,-2.03490971596286,-39.));
#18778=CARTESIAN_POINT('Ctrl Pts',(3.13182152067277,-2.05063248006214,-39.));
#18779=CARTESIAN_POINT('Ctrl Pts',(3.1233665817419,-2.06630519897744,-39.));
#18780=CARTESIAN_POINT('Ctrl Pts',(3.11480063144269,-2.08192668848259,-39.));
#18781=CARTESIAN_POINT('Ctrl Pts',(3.10623133858838,-2.09755427371415,-39.));
#18782=CARTESIAN_POINT('Ctrl Pts',(3.09755504214375,-2.11312309191788,-39.));
#18783=CARTESIAN_POINT('Ctrl Pts',(3.08877426972652,-2.12862929451707,-39.));
#18784=CARTESIAN_POINT('Ctrl Pts',(3.02953329395956,-2.23324452980258,-39.));
#18785=CARTESIAN_POINT('Ctrl Pts',(2.96551860353768,-2.33505128318285,-39.));
#18786=CARTESIAN_POINT('Ctrl Pts',(2.89700764639407,-2.43371931800978,-39.));
#18787=CARTESIAN_POINT('Ctrl Pts',(2.82795254228743,-2.5331710218108,-39.));
#18788=CARTESIAN_POINT('Ctrl Pts',(2.75432915537798,-2.62943477948419,-39.));
#18789=CARTESIAN_POINT('Ctrl Pts',(2.67637106031584,-2.72215810254695,-39.));
#18790=CARTESIAN_POINT('Ctrl Pts',(2.64144532396051,-2.7636987575963,-39.));
#18791=CARTESIAN_POINT('Ctrl Pts',(2.60564892511554,-2.80452854603288,-39.));
#18792=CARTESIAN_POINT('Ctrl Pts',(2.56899987285092,-2.84461416378751,-39.));
#18793=CARTESIAN_POINT('Ctrl Pts',(2.55485781801488,-2.86008231287714,-39.));
#18794=CARTESIAN_POINT('Ctrl Pts',(2.54058712398963,-2.87544139331927,-39.));
#18795=CARTESIAN_POINT('Ctrl Pts',(2.52619415150278,-2.89068374218847,-39.));
#18796=CARTESIAN_POINT('Ctrl Pts',(2.44149799814195,-2.98037809257957,-39.));
#18797=CARTESIAN_POINT('Ctrl Pts',(2.35271110511445,-3.06588609255451,-39.));
#18798=CARTESIAN_POINT('Ctrl Pts',(2.26009625880497,-3.14685732724484,-39.));
#18799=CARTESIAN_POINT('Ctrl Pts',(2.16854211452571,-3.22690121220187,-39.));
#18800=CARTESIAN_POINT('Ctrl Pts',(2.0732467193182,-3.30251241448694,-39.));
#18801=CARTESIAN_POINT('Ctrl Pts',(1.97442050833738,-3.37332724884043,-39.));
#18802=CARTESIAN_POINT('Ctrl Pts',(1.90109880310675,-3.42586659400901,-39.));
#18803=CARTESIAN_POINT('Ctrl Pts',(1.8258326265828,-3.47576531076396,-39.));
#18804=CARTESIAN_POINT('Ctrl Pts',(1.74869447533105,-3.52286199445091,-39.));
#18805=CARTESIAN_POINT('Ctrl Pts',(1.87273482856638,2.62278131463042,-39.0012934619393));
#18806=CARTESIAN_POINT('Ctrl Pts',(1.86214992567493,2.63033921364061,-39.0008623079595));
#18807=CARTESIAN_POINT('Ctrl Pts',(1.85151926948493,2.6378330347527,-39.0004311539798));
#18808=CARTESIAN_POINT('Ctrl Pts',(1.84084363913124,2.64526222873462,-39.));
#18809=CARTESIAN_POINT('Ctrl Pts',(-2.28363142167593,3.20550397776343,-39.4117842388297));
#18810=CARTESIAN_POINT('Ctrl Pts',(-3.33480719872521,2.45671378832311,-39.3465479133207));
#18811=CARTESIAN_POINT('Ctrl Pts',(-4.6260492952095,-0.141677978900424,
-39.2161173007676));
#18812=CARTESIAN_POINT('Ctrl Pts',(-2.44311639859766,-3.9353202317016,-39.0204924011703));
#18813=CARTESIAN_POINT('Ctrl Pts',(1.91917397033554,-4.2117711101878,-38.824909540038));
#18814=CARTESIAN_POINT('Ctrl Pts',(4.56986349694134,-0.739671892207571,
-38.6293266789055));
#18815=CARTESIAN_POINT('Ctrl Pts',(3.14895438396229,3.39389291624858,-38.4337438177732));
#18816=CARTESIAN_POINT('Ctrl Pts',(-1.07840564522595,4.50191710105457,-38.2381609566408));
#18817=CARTESIAN_POINT('Ctrl Pts',(-4.3445982160595,1.59878229949656,-38.0425780955084));
#18818=CARTESIAN_POINT('Ctrl Pts',(-3.73932021527481,-2.72935836966409,
-37.8469952343761));
#18819=CARTESIAN_POINT('Ctrl Pts',(0.198187846293384,-4.62516155268335,
-37.6514123732437));
#18820=CARTESIAN_POINT('Ctrl Pts',(3.95906382568818,-2.39946444773747,-37.4558295121113));
#18821=CARTESIAN_POINT('Ctrl Pts',(4.19194851914756,1.96448277024395,-37.260246650979));
#18822=CARTESIAN_POINT('Ctrl Pts',(0.689296288855085,4.57781990637833,-37.0646637898466));
#18823=CARTESIAN_POINT('Ctrl Pts',(-3.42759904373314,3.11177775663152,-36.8690809287142));
#18824=CARTESIAN_POINT('Ctrl Pts',(-4.49009219582733,-1.12723813956051,
-36.6734980675819));
#18825=CARTESIAN_POINT('Ctrl Pts',(-1.55137155401476,-4.36174658783765,
-36.4779152064495));
#18826=CARTESIAN_POINT('Ctrl Pts',(2.76980765447308,-3.70941463084786,-36.2823323453171));
#18827=CARTESIAN_POINT('Ctrl Pts',(4.62275476464721,0.248453248376883,-36.0867494841847));
#18828=CARTESIAN_POINT('Ctrl Pts',(2.35627039986063,3.98491903692357,-35.8911666230524));
#18829=CARTESIAN_POINT('Ctrl Pts',(-2.00993469357045,4.170342075127,-35.69558376192));
#18830=CARTESIAN_POINT('Ctrl Pts',(-4.5850458702089,0.639487862475723,-35.5000009007876));
#18831=CARTESIAN_POINT('Ctrl Pts',(-3.07432882350545,-3.46122703685094,
-35.3044180396553));
#18832=CARTESIAN_POINT('Ctrl Pts',(1.1759855524789,-4.47757169635789,-35.1088351785229));
#18833=CARTESIAN_POINT('Ctrl Pts',(4.37835513438434,-1.50386059040847,-34.9132523173905));
#18834=CARTESIAN_POINT('Ctrl Pts',(3.67908285493235,2.80997150208605,-34.7176694562581));
#18835=CARTESIAN_POINT('Ctrl Pts',(-0.298695466335132,4.61978040024479,
-34.5220865951258));
#18836=CARTESIAN_POINT('Ctrl Pts',(-4.01030011550478,2.31280859871278,-34.3265037339934));
#18837=CARTESIAN_POINT('Ctrl Pts',(-4.14824431536964,-2.05515460399684,
-34.130920872861));
#18838=CARTESIAN_POINT('Ctrl Pts',(-0.589602992809679,-4.59172683268392,
-33.9353380117287));
#18839=CARTESIAN_POINT('Ctrl Pts',(3.49444539435696,-3.03651858814776,-33.7397551505963));
#18840=CARTESIAN_POINT('Ctrl Pts',(4.4645224279339,1.22459605655993,-33.5441722894639));
#18841=CARTESIAN_POINT('Ctrl Pts',(1.4561712544547,4.39444305307998,-33.3485894283316));
#18842=CARTESIAN_POINT('Ctrl Pts',(-2.84980213881879,3.64832190347186,-33.1530065671991));
#18843=CARTESIAN_POINT('Ctrl Pts',(-4.61626206619028,-0.348913381918043,
-32.9574237060669));
#18844=CARTESIAN_POINT('Ctrl Pts',(-2.2690693624265,-4.03518550246901,-32.7618408449344));
#18845=CARTESIAN_POINT('Ctrl Pts',(2.10012355103143,-4.12569919562993,-32.5662579838021));
#18846=CARTESIAN_POINT('Ctrl Pts',(4.59788102830434,-0.539563295388051,
-32.3706751226697));
#18847=CARTESIAN_POINT('Ctrl Pts',(2.99831780357273,3.52708189147934,-32.1750922615373));
#18848=CARTESIAN_POINT('Ctrl Pts',(-1.2729990573875,4.4512802921326,-31.979509400405));
#18849=CARTESIAN_POINT('Ctrl Pts',(-4.41013611933087,1.40764565774636,-31.7839265392726));
#18850=CARTESIAN_POINT('Ctrl Pts',(-3.61688161784874,-2.88797714248122,
-31.5883436781402));
#18851=CARTESIAN_POINT('Ctrl Pts',(0.398584418807236,-4.6148340733141,-31.3927608170078));
#18852=CARTESIAN_POINT('Ctrl Pts',(4.06075387717163,-2.21958879719896,-31.1971779558755));
#18853=CARTESIAN_POINT('Ctrl Pts',(4.08541618930864,0.680499503299397,-31.0667893817872));
#18854=CARTESIAN_POINT('Ctrl Pts',(3.48785824455754,1.82347842508433,-31.0015950947431));
#18855=CARTESIAN_POINT('Ctrl Pts',(-2.14466679415544,3.01044112214796,-39.2735083224912));
#18856=CARTESIAN_POINT('Ctrl Pts',(-3.13187592188922,2.30721667014621,-39.2082719969821));
#18857=CARTESIAN_POINT('Ctrl Pts',(-4.34454273898582,-0.13305652301272,
-39.0778413844289));
#18858=CARTESIAN_POINT('Ctrl Pts',(-2.29444671526008,-3.69584624961263,
-38.8822164848317));
#18859=CARTESIAN_POINT('Ctrl Pts',(1.80238748132369,-3.95547440750044,-38.6866336236993));
#18860=CARTESIAN_POINT('Ctrl Pts',(4.29177598568882,-0.694661025737465,
-38.4910507625669));
#18861=CARTESIAN_POINT('Ctrl Pts',(2.95733271117712,3.18736612717297,-38.2954679014345));
#18862=CARTESIAN_POINT('Ctrl Pts',(-1.01278199099596,4.22796429626393,-38.0998850403022));
#18863=CARTESIAN_POINT('Ctrl Pts',(-4.08021865502781,1.50149243711901,-37.9043021791698));
#18864=CARTESIAN_POINT('Ctrl Pts',(-3.51177331958788,-2.56327015349656,
-37.7087193180375));
#18865=CARTESIAN_POINT('Ctrl Pts',(0.1861276250257,-4.34370901779091,-37.513136456905));
#18866=CARTESIAN_POINT('Ctrl Pts',(3.71814498710309,-2.25345109371567,-37.3175535957727));
#18867=CARTESIAN_POINT('Ctrl Pts',(3.9368580702165,1.84493912854848,-37.1219707346403));
#18868=CARTESIAN_POINT('Ctrl Pts',(0.647350902606326,4.29924822790718,-36.926387873508));
#18869=CARTESIAN_POINT('Ctrl Pts',(-3.21902115332542,2.92241837368895,-36.7308050123756));
#18870=CARTESIAN_POINT('Ctrl Pts',(-4.21685896580465,-1.05864290711448,
-36.5352221512432));
#18871=CARTESIAN_POINT('Ctrl Pts',(-1.45696675291454,-4.09632350591459,
-36.3396392901108));
#18872=CARTESIAN_POINT('Ctrl Pts',(2.60125799915053,-3.48368756403579,-36.1440564289785));
#18873=CARTESIAN_POINT('Ctrl Pts',(4.34144868876728,0.233334252907989,-35.9484735678461));
#18874=CARTESIAN_POINT('Ctrl Pts',(2.21288551062404,3.74242684470326,-35.7528907067137));
#18875=CARTESIAN_POINT('Ctrl Pts',(-1.88762518977692,3.91656643182389,-35.5573078455814));
#18876=CARTESIAN_POINT('Ctrl Pts',(-4.30603447394324,0.600573442324858,
-35.361724984449));
#18877=CARTESIAN_POINT('Ctrl Pts',(-2.88724830088749,-3.25060279978084,
-35.1661421233167));
#18878=CARTESIAN_POINT('Ctrl Pts',(1.10442391923172,-4.20510036973548,-34.9705592621842));
#18879=CARTESIAN_POINT('Ctrl Pts',(4.11192138127212,-1.41234694910663,-34.7749764010519));
#18880=CARTESIAN_POINT('Ctrl Pts',(3.45520155180266,2.63897777716875,-34.5793935399195));
#18881=CARTESIAN_POINT('Ctrl Pts',(-0.280519107476459,4.3386553218049,-34.3838106787871));
#18882=CARTESIAN_POINT('Ctrl Pts',(-3.76626342179548,2.17206846771106,-34.1882278176548));
#18883=CARTESIAN_POINT('Ctrl Pts',(-3.8958133754738,-1.93009335666479,-33.9926449565224));
#18884=CARTESIAN_POINT('Ctrl Pts',(-0.55372419052002,-4.31230888330598,
-33.7970620953901));
#18885=CARTESIAN_POINT('Ctrl Pts',(3.28179973796592,-2.85173891198998,-33.6014792342576));
#18886=CARTESIAN_POINT('Ctrl Pts',(4.19284518161218,1.15007635375341,-33.4058963731253));
#18887=CARTESIAN_POINT('Ctrl Pts',(1.36755962735034,4.1270303102727,-33.2103135119929));
#18888=CARTESIAN_POINT('Ctrl Pts',(-2.67638462101401,3.42631248041938,-33.0147306508605));
#18889=CARTESIAN_POINT('Ctrl Pts',(-4.3353510870909,-0.327681138529325,
-32.8191477897282));
#18890=CARTESIAN_POINT('Ctrl Pts',(-2.13099087227491,-3.7896344713332,-32.6235649285958));
#18891=CARTESIAN_POINT('Ctrl Pts',(1.9723258319048,-3.87464018210422,-32.4279820674634));
#18892=CARTESIAN_POINT('Ctrl Pts',(4.31808858088176,-0.506729532611965,
-32.232399206331));
#18893=CARTESIAN_POINT('Ctrl Pts',(2.81586273976224,3.31245022341271,-32.0368163451987));
#18894=CARTESIAN_POINT('Ctrl Pts',(-1.19553391210851,4.1804088625691,-31.8412334840663));
#18895=CARTESIAN_POINT('Ctrl Pts',(-4.14176841457767,1.32198693337744,-31.645650622934));
#18896=CARTESIAN_POINT('Ctrl Pts',(-3.39678541403965,-2.71223658116154,
-31.4500677618016));
#18897=CARTESIAN_POINT('Ctrl Pts',(0.374329569811351,-4.33400999111772,
-31.2544849006692));
#18898=CARTESIAN_POINT('Ctrl Pts',(3.81364694711398,-2.08452132198221,-31.0589020395368));
#18899=CARTESIAN_POINT('Ctrl Pts',(3.83680849648018,0.639089423237321,-30.9285134654486));
#18900=CARTESIAN_POINT('Ctrl Pts',(3.27561343254516,1.71251524699515,-30.8633191784045));
#18901=CARTESIAN_POINT('Ctrl Pts',(-2.00570216663496,2.81537826653249,-39.1352324061526));
#18902=CARTESIAN_POINT('Ctrl Pts',(-2.92894464505323,2.15771955196932,-39.0699960806435));
#18903=CARTESIAN_POINT('Ctrl Pts',(-4.06303618276213,-0.124435067125018,
-38.9395654680904));
#18904=CARTESIAN_POINT('Ctrl Pts',(-2.1457770319225,-3.45637226752366,-38.7439405684931));
#18905=CARTESIAN_POINT('Ctrl Pts',(1.68560099231183,-3.69917770481307,-38.5483577073607));
#18906=CARTESIAN_POINT('Ctrl Pts',(4.0136884744363,-0.649650159267356,-38.3527748462284));
#18907=CARTESIAN_POINT('Ctrl Pts',(2.76571103839194,2.98083933809737,-38.157191985096));
#18908=CARTESIAN_POINT('Ctrl Pts',(-0.94715833676596,3.95401149147329,-37.9616091239636));
#18909=CARTESIAN_POINT('Ctrl Pts',(-3.81583909399612,1.40420257474148,-37.7660262628312));
#18910=CARTESIAN_POINT('Ctrl Pts',(-3.28422642390096,-2.39718193732903,
-37.5704434016989));
#18911=CARTESIAN_POINT('Ctrl Pts',(0.174067403758018,-4.06225648289848,
-37.3748605405665));
#18912=CARTESIAN_POINT('Ctrl Pts',(3.477226148518,-2.10743773969387,-37.1792776794341));
#18913=CARTESIAN_POINT('Ctrl Pts',(3.68176762128544,1.72539548685299,-36.9836948183018));
#18914=CARTESIAN_POINT('Ctrl Pts',(0.605405516357568,4.02067654943603,-36.7881119571694));
#18915=CARTESIAN_POINT('Ctrl Pts',(-3.01044326291771,2.73305899074637,-36.592529096037));
#18916=CARTESIAN_POINT('Ctrl Pts',(-3.94362573578198,-0.990047674668459,
-36.3969462349047));
#18917=CARTESIAN_POINT('Ctrl Pts',(-1.36256195181432,-3.8309004239915,-36.2013633737723));
#18918=CARTESIAN_POINT('Ctrl Pts',(2.43270834382797,-3.2579604972237,-36.00578051264));
#18919=CARTESIAN_POINT('Ctrl Pts',(4.06014261288736,0.218215257439091,-35.8101976515075));
#18920=CARTESIAN_POINT('Ctrl Pts',(2.06950062138747,3.49993465248296,-35.6146147903752));
#18921=CARTESIAN_POINT('Ctrl Pts',(-1.76531568598338,3.66279078852076,-35.4190319292428));
#18922=CARTESIAN_POINT('Ctrl Pts',(-4.02702307767759,0.561659022173995,
-35.2234490681104));
#18923=CARTESIAN_POINT('Ctrl Pts',(-2.70016777826954,-3.03997856271072,
-35.0278662069781));
#18924=CARTESIAN_POINT('Ctrl Pts',(1.03286228598455,-3.93262904311309,-34.8322833458457));
#18925=CARTESIAN_POINT('Ctrl Pts',(3.8454876281599,-1.32083330780479,-34.6367004847133));
#18926=CARTESIAN_POINT('Ctrl Pts',(3.23132024867299,2.46798405225144,-34.4411176235809));
#18927=CARTESIAN_POINT('Ctrl Pts',(-0.262342748617795,4.05753024336501,
-34.2455347624486));
#18928=CARTESIAN_POINT('Ctrl Pts',(-3.52222672808616,2.03132833670935,-34.0499519013162));
#18929=CARTESIAN_POINT('Ctrl Pts',(-3.64338243557798,-1.80503210933276,
-33.8543690401839));
#18930=CARTESIAN_POINT('Ctrl Pts',(-0.517845388230359,-4.03289093392803,
-33.6587861790514));
#18931=CARTESIAN_POINT('Ctrl Pts',(3.06915408157487,-2.66695923583222,-33.4632033179192));
#18932=CARTESIAN_POINT('Ctrl Pts',(3.92116793529046,1.07555665094691,-33.2676204567867));
#18933=CARTESIAN_POINT('Ctrl Pts',(1.27894800024599,3.85961756746542,-33.0720375956544));
#18934=CARTESIAN_POINT('Ctrl Pts',(-2.50296710320924,3.2043030573669,-32.8764547345219));
#18935=CARTESIAN_POINT('Ctrl Pts',(-4.05444010799154,-0.306448895140604,
-32.6808718733897));
#18936=CARTESIAN_POINT('Ctrl Pts',(-1.99291238212331,-3.54408344019739,
-32.4852890122572));
#18937=CARTESIAN_POINT('Ctrl Pts',(1.84452811277818,-3.62358116857851,-32.2897061511249));
#18938=CARTESIAN_POINT('Ctrl Pts',(4.03829613345918,-0.473895769835876,
-32.0941232899925));
#18939=CARTESIAN_POINT('Ctrl Pts',(2.63340767595175,3.09781855534609,-31.8985404288602));
#18940=CARTESIAN_POINT('Ctrl Pts',(-1.11806876682953,3.90953743300561,-31.7029575677278));
#18941=CARTESIAN_POINT('Ctrl Pts',(-3.87340070982448,1.23632820900851,-31.5073747065954));
#18942=CARTESIAN_POINT('Ctrl Pts',(-3.17668921023055,-2.53649601984187,
-31.311791845463));
#18943=CARTESIAN_POINT('Ctrl Pts',(0.350074720815462,-4.05318590892136,
-31.1162089843306));
#18944=CARTESIAN_POINT('Ctrl Pts',(3.56654001705634,-1.94945384676547,-30.9206261231983));
#18945=CARTESIAN_POINT('Ctrl Pts',(3.58820080365172,0.597679343175246,-30.79023754911));
#18946=CARTESIAN_POINT('Ctrl Pts',(3.06336862053276,1.60155206890597,-30.7250432620659));
#18947=CARTESIAN_POINT('Ctrl Pts',(-1.86673753911448,2.62031541091702,-38.996956489814));
#18948=CARTESIAN_POINT('Ctrl Pts',(-2.72601336821725,2.00822243379242,-38.9317201643049));
#18949=CARTESIAN_POINT('Ctrl Pts',(-3.78152962653845,-0.115813611237318,
-38.8012895517517));
#18950=CARTESIAN_POINT('Ctrl Pts',(-1.99710734858491,-3.21689828543468,
-38.6056646521545));
#18951=CARTESIAN_POINT('Ctrl Pts',(1.56881450329997,-3.44288100212573,-38.4100817910221));
#18952=CARTESIAN_POINT('Ctrl Pts',(3.73560096318379,-0.604639292797246,
-38.2144989298897));
#18953=CARTESIAN_POINT('Ctrl Pts',(2.57408936560678,2.77431254902176,-38.0189160687574));
#18954=CARTESIAN_POINT('Ctrl Pts',(-0.881534682535969,3.68005868668266,
-37.823333207625));
#18955=CARTESIAN_POINT('Ctrl Pts',(-3.55145953296442,1.30691271236393,-37.6277503464926));
#18956=CARTESIAN_POINT('Ctrl Pts',(-3.05667952821403,-2.23109372116149,
-37.4321674853603));
#18957=CARTESIAN_POINT('Ctrl Pts',(0.162007182490337,-3.78080394800605,
-37.2365846242278));
#18958=CARTESIAN_POINT('Ctrl Pts',(3.23630730993291,-1.96142438567206,-37.0410017630955));
#18959=CARTESIAN_POINT('Ctrl Pts',(3.42667717235439,1.60585184515752,-36.8454189019631));
#18960=CARTESIAN_POINT('Ctrl Pts',(0.563460130108804,3.74210487096489,-36.6498360408308));
#18961=CARTESIAN_POINT('Ctrl Pts',(-2.80186537250999,2.5436996078038,-36.4542531796984));
#18962=CARTESIAN_POINT('Ctrl Pts',(-3.67039250575931,-0.921452442222433,
-36.258670318566));
#18963=CARTESIAN_POINT('Ctrl Pts',(-1.2681571507141,-3.56547734206843,-36.0630874574336));
#18964=CARTESIAN_POINT('Ctrl Pts',(2.26415868850542,-3.03223343041163,-35.8675045963013));
#18965=CARTESIAN_POINT('Ctrl Pts',(3.77883653700745,0.203096261970197,-35.6719217351689));
#18966=CARTESIAN_POINT('Ctrl Pts',(1.92611573215089,3.25744246026265,-35.4763388740365));
#18967=CARTESIAN_POINT('Ctrl Pts',(-1.64300618218985,3.40901514521765,-35.2807560129042));
#18968=CARTESIAN_POINT('Ctrl Pts',(-3.74801168141193,0.522744602023131,
-35.0851731517718));
#18969=CARTESIAN_POINT('Ctrl Pts',(-2.51308725565157,-2.82935432564062,
-34.8895902906395));
#18970=CARTESIAN_POINT('Ctrl Pts',(0.961300652737371,-3.66015771649069,
-34.6940074295071));
#18971=CARTESIAN_POINT('Ctrl Pts',(3.57905387504768,-1.22931966650296,-34.4984245683747));
#18972=CARTESIAN_POINT('Ctrl Pts',(3.00743894554333,2.29699032733414,-34.3028417072423));
#18973=CARTESIAN_POINT('Ctrl Pts',(-0.24416638975912,3.77640516492511,-34.1072588461099));
#18974=CARTESIAN_POINT('Ctrl Pts',(-3.27819003437687,1.89058820570765,-33.9116759849776));
#18975=CARTESIAN_POINT('Ctrl Pts',(-3.39095149568214,-1.67997086200072,
-33.7160931238452));
#18976=CARTESIAN_POINT('Ctrl Pts',(-0.481966585940703,-3.75347298455009,
-33.5205102627128));
#18977=CARTESIAN_POINT('Ctrl Pts',(2.85650842518383,-2.48217955967445,-33.3249274015805));
#18978=CARTESIAN_POINT('Ctrl Pts',(3.64949068896873,1.0010369481404,-33.1293445404481));
#18979=CARTESIAN_POINT('Ctrl Pts',(1.19033637314163,3.59220482465815,-32.9337616793157));
#18980=CARTESIAN_POINT('Ctrl Pts',(-2.32954958540446,2.98229363431442,-32.7381788181833));
#18981=CARTESIAN_POINT('Ctrl Pts',(-3.77352912889216,-0.285216651751885,
-32.542595957051));
#18982=CARTESIAN_POINT('Ctrl Pts',(-1.85483389197172,-3.29853240906158,
-32.3470130959186));
#18983=CARTESIAN_POINT('Ctrl Pts',(1.71673039365155,-3.37252215505281,-32.1514302347862));
#18984=CARTESIAN_POINT('Ctrl Pts',(3.75850368603659,-0.441062007059785,
-31.9558473736539));
#18985=CARTESIAN_POINT('Ctrl Pts',(2.45095261214126,2.88318688727946,-31.7602645125215));
#18986=CARTESIAN_POINT('Ctrl Pts',(-1.04060362155055,3.63866600344211,-31.5646816513891));
#18987=CARTESIAN_POINT('Ctrl Pts',(-3.60503300507128,1.15066948463959,-31.3690987902567));
#18988=CARTESIAN_POINT('Ctrl Pts',(-2.95659300642146,-2.36075545852219,
-31.1735159291244));
#18989=CARTESIAN_POINT('Ctrl Pts',(0.325819871819575,-3.772361826725,-30.977933067992));
#18990=CARTESIAN_POINT('Ctrl Pts',(3.3194330869987,-1.81438637154873,-30.7823502068597));
#18991=CARTESIAN_POINT('Ctrl Pts',(3.33959311082326,0.556269263113169,-30.6519616327714));
#18992=CARTESIAN_POINT('Ctrl Pts',(2.85112380852038,1.49058889081678,-30.5867673457273));
#18993=CARTESIAN_POINT('',(-0.026575674920773,-3.22485156263098,-30.9987013393169));
#18994=CARTESIAN_POINT('Ctrl Pts',(-0.0264634121681443,-3.22711996923596,
-31.));
#18995=CARTESIAN_POINT('Ctrl Pts',(0.0758388090705951,-3.23962881840859,
-31.));
#18996=CARTESIAN_POINT('Ctrl Pts',(0.178439658895469,-3.24693606621664,
-31.));
#18997=CARTESIAN_POINT('Ctrl Pts',(0.280985511217878,-3.24890874069818,
-31.));
#18998=CARTESIAN_POINT('Ctrl Pts',(0.383279979523717,-3.2508765793056,-31.));
#18999=CARTESIAN_POINT('Ctrl Pts',(0.485520482367711,-3.24753728876359,
-31.));
#19000=CARTESIAN_POINT('Ctrl Pts',(0.587413164141851,-3.23916568357852,
-31.));
#19001=CARTESIAN_POINT('Ctrl Pts',(0.692190255801988,-3.23055709237702,
-31.));
#19002=CARTESIAN_POINT('Ctrl Pts',(0.796600205213911,-3.21662724834392,
-31.));
#19003=CARTESIAN_POINT('Ctrl Pts',(0.900334660288271,-3.19762078169955,
-31.));
#19004=CARTESIAN_POINT('Ctrl Pts',(0.956443167896035,-3.18734045123898,
-31.));
#19005=CARTESIAN_POINT('Ctrl Pts',(1.012354186777,-3.1755739904251,-31.));
#19006=CARTESIAN_POINT('Ctrl Pts',(1.06801915047778,-3.16235380686495,-31.));
#19007=CARTESIAN_POINT('Ctrl Pts',(1.10531324032011,-3.15349662488465,-31.));
#19008=CARTESIAN_POINT('Ctrl Pts',(1.14249688454736,-3.14398682690968,-31.));
#19009=CARTESIAN_POINT('Ctrl Pts',(1.17955536555834,-3.13383309957192,-31.));
#19010=CARTESIAN_POINT('Ctrl Pts',(1.19611854884196,-3.12929491985383,-31.));
#19011=CARTESIAN_POINT('Ctrl Pts',(1.21265672752102,-3.12462809653692,-31.));
#19012=CARTESIAN_POINT('Ctrl Pts',(1.22916857715676,-3.11983335183728,-31.));
#19013=CARTESIAN_POINT('Ctrl Pts',(1.24405309889832,-3.11551115394295,-31.));
#19014=CARTESIAN_POINT('Ctrl Pts',(1.2589070195229,-3.11108767246599,-31.));
#19015=CARTESIAN_POINT('Ctrl Pts',(1.2737279671354,-3.10656427085961,-31.));
#19016=CARTESIAN_POINT('Ctrl Pts',(1.37803722183118,-3.07472874572406,-31.));
#19017=CARTESIAN_POINT('Ctrl Pts',(1.48073557027737,-3.03794162316132,-31.));
#19018=CARTESIAN_POINT('Ctrl Pts',(1.58149763038563,-2.99650306755549,-31.));
#19019=CARTESIAN_POINT('Ctrl Pts',(1.68389159427881,-2.95439338895295,-31.));
#19020=CARTESIAN_POINT('Ctrl Pts',(1.78428684038955,-2.90748021838541,-31.));
#19021=CARTESIAN_POINT('Ctrl Pts',(1.88234521022483,-2.85602367353166,-31.));
#19022=CARTESIAN_POINT('Ctrl Pts',(1.98123876893857,-2.80412885977686,-31.));
#19023=CARTESIAN_POINT('Ctrl Pts',(2.07775635551852,-2.7476126815164,-31.));
#19024=CARTESIAN_POINT('Ctrl Pts',(2.17154166571046,-2.6866900413243,-31.));
#19025=CARTESIAN_POINT('Ctrl Pts',(2.24919685881724,-2.63624547405667,-31.));
#19026=CARTESIAN_POINT('Ctrl Pts',(2.32497887842971,-2.58277880173925,-31.));
#19027=CARTESIAN_POINT('Ctrl Pts',(2.398673972733,-2.52638751539726,-31.));
#19028=CARTESIAN_POINT('Ctrl Pts',(2.41107729107925,-2.51689652982941,-31.));
#19029=CARTESIAN_POINT('Ctrl Pts',(2.42341995870474,-2.50732373674807,-31.));
#19030=CARTESIAN_POINT('Ctrl Pts',(2.43569181428942,-2.49767698557919,-31.));
#19031=CARTESIAN_POINT('Ctrl Pts',(2.52604411377092,-2.42665218051856,-31.));
#19032=CARTESIAN_POINT('Ctrl Pts',(2.61269805739617,-2.35151645309661,-31.));
#19033=CARTESIAN_POINT('Ctrl Pts',(2.69530150548317,-2.27254862134861,-31.));
#19034=CARTESIAN_POINT('Ctrl Pts',(2.77921691691963,-2.19232656954756,-31.));
#19035=CARTESIAN_POINT('Ctrl Pts',(2.85895313717407,-2.10814944182442,-31.));
#19036=CARTESIAN_POINT('Ctrl Pts',(2.93412359511511,-2.02025777063396,-31.));
#19037=CARTESIAN_POINT('Ctrl Pts',(3.00929405305615,-1.93236609944351,-31.));
#19038=CARTESIAN_POINT('Ctrl Pts',(3.07989974015383,-1.84075946109991,-31.));
#19039=CARTESIAN_POINT('Ctrl Pts',(3.14552194485315,-1.74563250373385,-31.));
#19040=CARTESIAN_POINT('Ctrl Pts',(3.14923670751426,-1.74024752663795,-31.));
#19041=CARTESIAN_POINT('Ctrl Pts',(3.15293548965499,-1.73485125747499,-31.));
#19042=CARTESIAN_POINT('Ctrl Pts',(3.15661821120802,-1.72944372759524,-31.));
#19043=CARTESIAN_POINT('Ctrl Pts',(3.19985700463249,-1.6659539784952,-31.));
#19044=CARTESIAN_POINT('Ctrl Pts',(3.24088262168145,-1.60091250612483,-31.));
#19045=CARTESIAN_POINT('Ctrl Pts',(3.27969752040755,-1.53443522991608,-31.));
#19046=CARTESIAN_POINT('Ctrl Pts',(3.28816156612781,-1.5199390770558,-31.));
#19047=CARTESIAN_POINT('Ctrl Pts',(3.29652094980811,-1.50537374488921,-31.));
#19048=CARTESIAN_POINT('Ctrl Pts',(3.3047740963749,-1.49074312709972,-31.));
#19049=CARTESIAN_POINT('Ctrl Pts',(3.31263779296697,-1.47680289977913,-31.));
#19050=CARTESIAN_POINT('Ctrl Pts',(3.32040197057988,-1.46280884199712,-31.));
#19051=CARTESIAN_POINT('Ctrl Pts',(3.32806517242938,-1.44876535269138,-31.));
#19052=CARTESIAN_POINT('Ctrl Pts',(3.38197815672864,-1.34996508182343,-31.));
#19053=CARTESIAN_POINT('Ctrl Pts',(3.43092600979739,-1.24866875081712,-31.));
#19054=CARTESIAN_POINT('Ctrl Pts',(3.4749924224499,-1.14529854716208,-31.));
#19055=CARTESIAN_POINT('Ctrl Pts',(3.51987212649102,-1.04002053909523,-31.));
#19056=CARTESIAN_POINT('Ctrl Pts',(3.55968881815558,-0.932590809276557,
-31.));
#19057=CARTESIAN_POINT('Ctrl Pts',(3.59449143272375,-0.823416466411623,
-31.));
#19058=CARTESIAN_POINT('Ctrl Pts',(3.62999642302698,-0.712038800311621,
-31.));
#19059=CARTESIAN_POINT('Ctrl Pts',(3.66028323731959,-0.598844700472671,
-31.));
#19060=CARTESIAN_POINT('Ctrl Pts',(3.68535848353317,-0.484236133285269,
-31.));
#19061=CARTESIAN_POINT('Ctrl Pts',(3.70593368219157,-0.390195420075543,
-31.));
#19062=CARTESIAN_POINT('Ctrl Pts',(3.72299923124982,-0.295201598735365,
-31.));
#19063=CARTESIAN_POINT('Ctrl Pts',(3.73653440245394,-0.199467195515414,
-31.));
#19064=CARTESIAN_POINT('Ctrl Pts',(3.73902614120766,-0.18184310203554,-31.));
#19065=CARTESIAN_POINT('Ctrl Pts',(3.74139817189912,-0.164193894712116,
-31.));
#19066=CARTESIAN_POINT('Ctrl Pts',(3.74365028064763,-0.146520881969029,
-31.));
#19067=CARTESIAN_POINT('Ctrl Pts',(3.745903251544,-0.128841103677876,-31.));
#19068=CARTESIAN_POINT('Ctrl Pts',(3.7480351141005,-0.111145974267687,-31.));
#19069=CARTESIAN_POINT('Ctrl Pts',(3.75004565109281,-0.0934400925234178,
-31.));
#19070=CARTESIAN_POINT('Ctrl Pts',(3.76361018597104,0.0260165757139654,
-31.));
#19071=CARTESIAN_POINT('Ctrl Pts',(3.77166191629321,0.146007054496315,-31.));
#19072=CARTESIAN_POINT('Ctrl Pts',(3.77423118674206,0.26610109164289,-31.));
#19073=CARTESIAN_POINT('Ctrl Pts',(3.7768208619918,0.387148899505717,-31.));
#19074=CARTESIAN_POINT('Ctrl Pts',(3.77384088651866,0.508302769592539,-31.));
#19075=CARTESIAN_POINT('Ctrl Pts',(3.76527303135289,0.629140236416144,-31.));
#19076=CARTESIAN_POINT('Ctrl Pts',(3.76143457294323,0.683276257830769,-31.));
#19077=CARTESIAN_POINT('Ctrl Pts',(3.75647389257586,0.737348936727639,-31.));
#19078=CARTESIAN_POINT('Ctrl Pts',(3.75038598358214,0.791320743572583,-31.));
#19079=CARTESIAN_POINT('Ctrl Pts',(3.74803679376988,0.812147273489508,-31.));
#19080=CARTESIAN_POINT('Ctrl Pts',(3.74551942283083,0.832961176947892,-31.));
#19081=CARTESIAN_POINT('Ctrl Pts',(3.74283451253955,0.853752515419332,-31.));
#19082=CARTESIAN_POINT('Ctrl Pts',(3.72703504525638,0.976100019177537,-31.));
#19083=CARTESIAN_POINT('Ctrl Pts',(3.70546540675222,1.09746515777843,-31.));
#19084=CARTESIAN_POINT('Ctrl Pts',(3.6781322195357,1.21740997293571,-31.));
#19085=CARTESIAN_POINT('Ctrl Pts',(3.65111210442695,1.33598094991597,-31.));
#19086=CARTESIAN_POINT('Ctrl Pts',(3.61845977551099,1.45316484915809,-31.));
#19087=CARTESIAN_POINT('Ctrl Pts',(3.58013170248686,1.56854374917087,-31.));
#19088=CARTESIAN_POINT('Ctrl Pts',(3.55169508562206,1.65414642405306,-31.));
#19089=CARTESIAN_POINT('Ctrl Pts',(3.52013321748227,1.73875570516642,-31.));
#19090=CARTESIAN_POINT('Ctrl Pts',(3.48540987471234,1.82219839898341,-31.));
#19091=CARTESIAN_POINT('Ctrl Pts',(-0.065570273740064,-3.22208288250033,
-31.));
#19092=CARTESIAN_POINT('Ctrl Pts',(-0.0525672847650432,-3.22234749690587,
-30.9995671131056));
#19093=CARTESIAN_POINT('Ctrl Pts',(-0.0395626939642705,-3.22253339835127,
-30.9991342262113));
#19094=CARTESIAN_POINT('Ctrl Pts',(-0.026557454381041,-3.22264057321272,
-30.9987013393169));
#19095=CARTESIAN_POINT('Ctrl Pts',(-1.75281221119047,-3.52691927538468,
-39.));
#19096=CARTESIAN_POINT('Ctrl Pts',(-1.85924677934811,-3.46275184993558,
-39.));
#19097=CARTESIAN_POINT('Ctrl Pts',(-1.96213599398535,-3.3934582774933,-39.));
#19098=CARTESIAN_POINT('Ctrl Pts',(-2.06105560704088,-3.31905293948038,
-39.));
#19099=CARTESIAN_POINT('Ctrl Pts',(-2.15734339103454,-3.24662721021129,
-39.));
#19100=CARTESIAN_POINT('Ctrl Pts',(-2.24987036069143,-3.16935730201866,
-39.));
#19101=CARTESIAN_POINT('Ctrl Pts',(-2.33847820579006,-3.08765584052718,
-39.));
#19102=CARTESIAN_POINT('Ctrl Pts',(-2.42826178589376,-3.00487028464052,
-39.));
#19103=CARTESIAN_POINT('Ctrl Pts',(-2.51402198065837,-2.91753393939187,
-39.));
#19104=CARTESIAN_POINT('Ctrl Pts',(-2.59554934753375,-2.82604649297915,
-39.));
#19105=CARTESIAN_POINT('Ctrl Pts',(-2.67707671440914,-2.73455904656643,
-39.));
#19106=CARTESIAN_POINT('Ctrl Pts',(-2.75437159913114,-2.6389195840714,-39.));
#19107=CARTESIAN_POINT('Ctrl Pts',(-2.82717436902469,-2.53951181872049,
-39.));
#19108=CARTESIAN_POINT('Ctrl Pts',(-2.83965430798123,-2.52247121923232,
-39.));
#19109=CARTESIAN_POINT('Ctrl Pts',(-2.8520040143943,-2.5053170440578,-39.));
#19110=CARTESIAN_POINT('Ctrl Pts',(-2.86420738431601,-2.4880723282558,-39.));
#19111=CARTESIAN_POINT('Ctrl Pts',(-2.93338468399664,-2.39031712779931,
-39.));
#19112=CARTESIAN_POINT('Ctrl Pts',(-2.99796046584097,-2.28952514865008,
-39.));
#19113=CARTESIAN_POINT('Ctrl Pts',(-3.05778195366412,-2.18609573317179,
-39.));
#19114=CARTESIAN_POINT('Ctrl Pts',(-3.11753452619717,-2.08278546999867,
-39.));
#19115=CARTESIAN_POINT('Ctrl Pts',(-3.17254403905503,-1.97684294431477,
-39.));
#19116=CARTESIAN_POINT('Ctrl Pts',(-3.22261026970107,-1.86864638142994,
-39.));
#19117=CARTESIAN_POINT('Ctrl Pts',(-3.271620158212,-1.76273264644676,-39.));
#19118=CARTESIAN_POINT('Ctrl Pts',(-3.31589325903411,-1.65465815862718,
-39.));
#19119=CARTESIAN_POINT('Ctrl Pts',(-3.35519317305696,-1.54477157537668,
-39.));
#19120=CARTESIAN_POINT('Ctrl Pts',(-3.39058551444191,-1.44581096529071,
-39.));
#19121=CARTESIAN_POINT('Ctrl Pts',(-3.4219439883879,-1.34538022953061,-39.));
#19122=CARTESIAN_POINT('Ctrl Pts',(-3.44905986541963,-1.24373767821722,
-39.));
#19123=CARTESIAN_POINT('Ctrl Pts',(-3.45507889936618,-1.22117562108541,
-39.));
#19124=CARTESIAN_POINT('Ctrl Pts',(-3.46089005423046,-1.19854820161701,
-39.));
#19125=CARTESIAN_POINT('Ctrl Pts',(-3.46648322368768,-1.17589021910338,
-39.));
#19126=CARTESIAN_POINT('Ctrl Pts',(-3.49403430178266,-1.06428054046186,
-39.));
#19127=CARTESIAN_POINT('Ctrl Pts',(-3.51633488607024,-0.951810304057931,
-39.));
#19128=CARTESIAN_POINT('Ctrl Pts',(-3.53320430915353,-0.838823268609796,
-39.));
#19129=CARTESIAN_POINT('Ctrl Pts',(-3.54982973534889,-0.727470461249351,
-39.));
#19130=CARTESIAN_POINT('Ctrl Pts',(-3.5611800757903,-0.615614942649066,
-39.));
#19131=CARTESIAN_POINT('Ctrl Pts',(-3.56703215600623,-0.503586796080013,
-39.));
#19132=CARTESIAN_POINT('Ctrl Pts',(-3.57272988890964,-0.394513366929766,
-39.));
#19133=CARTESIAN_POINT('Ctrl Pts',(-3.57321554812162,-0.285275688187582,
-39.));
#19134=CARTESIAN_POINT('Ctrl Pts',(-3.56823476358766,-0.176189271538187,
-39.));
#19135=CARTESIAN_POINT('Ctrl Pts',(-3.56727789656693,-0.155232493787625,
-39.));
#19136=CARTESIAN_POINT('Ctrl Pts',(-3.56611913357304,-0.134281346867122,
-39.));
#19137=CARTESIAN_POINT('Ctrl Pts',(-3.56475645999484,-0.113338143574554,
-39.));
#19138=CARTESIAN_POINT('Ctrl Pts',(-3.56024904482747,-0.0440627766162007,
-39.));
#19139=CARTESIAN_POINT('Ctrl Pts',(-3.55351098219617,0.0251259798909786,
-39.));
#19140=CARTESIAN_POINT('Ctrl Pts',(-3.54458068183499,0.0941423097710962,
-39.));
#19141=CARTESIAN_POINT('Ctrl Pts',(-3.54202177207861,0.113918415023707,
-39.));
#19142=CARTESIAN_POINT('Ctrl Pts',(-3.53928283006026,0.133680337115747,
-39.));
#19143=CARTESIAN_POINT('Ctrl Pts',(-3.53636467707845,0.15342599149552,-39.));
#19144=CARTESIAN_POINT('Ctrl Pts',(-3.53393720844056,0.16985143493198,-39.));
#19145=CARTESIAN_POINT('Ctrl Pts',(-3.53138560410875,0.186265940392125,
-39.));
#19146=CARTESIAN_POINT('Ctrl Pts',(-3.52871303514421,0.202652981912964,
-39.));
#19147=CARTESIAN_POINT('Ctrl Pts',(-3.52789260432643,0.207683510237725,
-39.));
#19148=CARTESIAN_POINT('Ctrl Pts',(-3.52706072562481,0.21271179145904,-39.));
#19149=CARTESIAN_POINT('Ctrl Pts',(-3.5262174297509,0.217737774115531,-39.));
#19150=CARTESIAN_POINT('Ctrl Pts',(-3.50784848795626,0.327215343891981,
-39.));
#19151=CARTESIAN_POINT('Ctrl Pts',(-3.48406506021569,0.435613933294974,
-39.));
#19152=CARTESIAN_POINT('Ctrl Pts',(-3.45511869430776,0.542614318777618,
-39.));
#19153=CARTESIAN_POINT('Ctrl Pts',(-3.42583968563334,0.650844319900267,
-39.));
#19154=CARTESIAN_POINT('Ctrl Pts',(-3.39127789178026,0.757644593911477,
-39.));
#19155=CARTESIAN_POINT('Ctrl Pts',(-3.35164455227839,0.862663619089397,
-39.));
#19156=CARTESIAN_POINT('Ctrl Pts',(-3.31212647970358,0.967377214029349,
-39.));
#19157=CARTESIAN_POINT('Ctrl Pts',(-3.26756572112307,1.07032063431149,-39.));
#19158=CARTESIAN_POINT('Ctrl Pts',(-3.21813160441969,1.17111310733081,-39.));
#19159=CARTESIAN_POINT('Ctrl Pts',(-3.19429583585514,1.21971245976496,-39.));
#19160=CARTESIAN_POINT('Ctrl Pts',(-3.16932651798421,1.26781118858304,-39.));
#19161=CARTESIAN_POINT('Ctrl Pts',(-3.14323990782853,1.31536315285873,-39.));
#19162=CARTESIAN_POINT('Ctrl Pts',(-3.12740697868958,1.3442241998212,-39.));
#19163=CARTESIAN_POINT('Ctrl Pts',(-3.11116300262372,1.3728828286187,-39.));
#19164=CARTESIAN_POINT('Ctrl Pts',(-3.09450947007563,1.401331437924,-39.));
#19165=CARTESIAN_POINT('Ctrl Pts',(-3.08121617070089,1.42403988606846,-39.));
#19166=CARTESIAN_POINT('Ctrl Pts',(-3.06766332150694,1.44661163127224,-39.));
#19167=CARTESIAN_POINT('Ctrl Pts',(-3.05386840941538,1.46901669000711,-39.));
#19168=CARTESIAN_POINT('Ctrl Pts',(-2.99619963659367,1.56267964586087,-39.));
#19169=CARTESIAN_POINT('Ctrl Pts',(-2.93424670289176,1.65353184103952,-39.));
#19170=CARTESIAN_POINT('Ctrl Pts',(-2.86819294799962,1.74122159681554,-39.));
#19171=CARTESIAN_POINT('Ctrl Pts',(-2.80342392707767,1.82720580219149,-39.));
#19172=CARTESIAN_POINT('Ctrl Pts',(-2.73471142703462,1.91014989765233,-39.));
#19173=CARTESIAN_POINT('Ctrl Pts',(-2.66219917441839,1.98968213489971,-39.));
#19174=CARTESIAN_POINT('Ctrl Pts',(-2.62723747571619,2.02802851106971,-39.));
#19175=CARTESIAN_POINT('Ctrl Pts',(-2.59139207824707,2.06558109012876,-39.));
#19176=CARTESIAN_POINT('Ctrl Pts',(-2.55467723691739,2.102294244759,-39.));
#19177=CARTESIAN_POINT('Ctrl Pts',(-2.54276804759259,2.11420288696928,-39.));
#19178=CARTESIAN_POINT('Ctrl Pts',(-2.53076810266377,2.1260223834559,-39.));
#19179=CARTESIAN_POINT('Ctrl Pts',(-2.51868516007585,2.13774431665332,-39.));
#19180=CARTESIAN_POINT('Ctrl Pts',(-2.44276707797251,2.21139414825824,-39.));
#19181=CARTESIAN_POINT('Ctrl Pts',(-2.36349897831715,2.28127220136821,-39.));
#19182=CARTESIAN_POINT('Ctrl Pts',(-2.28103031984326,2.34703489324668,-39.));
#19183=CARTESIAN_POINT('Ctrl Pts',(-2.20080167582135,2.41101133828986,-39.));
#19184=CARTESIAN_POINT('Ctrl Pts',(-2.11754342366811,2.4710932686734,-39.));
#19185=CARTESIAN_POINT('Ctrl Pts',(-2.03137376194493,2.52691956397708,-39.));
#19186=CARTESIAN_POINT('Ctrl Pts',(-1.97917218845064,2.56073912876277,-39.));
#19187=CARTESIAN_POINT('Ctrl Pts',(-1.92590180692628,2.59299601272173,-39.));
#19188=CARTESIAN_POINT('Ctrl Pts',(-1.87158653173895,2.62360084935064,-39.));
#19189=CARTESIAN_POINT('Origin',(0.,0.,-31.));
#19190=CARTESIAN_POINT('Origin',(0.,0.,-39.));
#19191=CARTESIAN_POINT('',(0.,0.,0.));
#19192=CARTESIAN_POINT('Origin',(-9.35406549764863E-15,0.,41.4527091182931));
#19193=CARTESIAN_POINT('',(-0.490582094004581,-3.18519179509525,59.6160848123881));
#19194=CARTESIAN_POINT('',(-0.490582094296225,-3.18519179505033,59.8598970253053));
#19195=CARTESIAN_POINT('',(-0.490582094296226,-3.18519179505033,41.4527091182931));
#19196=CARTESIAN_POINT('',(1.13209532136445,3.01736271366979,60.1999356690201));
#19197=CARTESIAN_POINT('Ctrl Pts',(-0.490582094004581,-3.18519179509525,
59.6160848123881));
#19198=CARTESIAN_POINT('Ctrl Pts',(-0.466375895170159,-3.18892002512848,
59.6176608165468));
#19199=CARTESIAN_POINT('Ctrl Pts',(-0.44212674100936,-3.19237238887795,
59.6192250328061));
#19200=CARTESIAN_POINT('Ctrl Pts',(-0.396256821284568,-3.19837018876251,
59.6221535062883));
#19201=CARTESIAN_POINT('Ctrl Pts',(-0.374645516026424,-3.20097362267201,
59.6235205400371));
#19202=CARTESIAN_POINT('Ctrl Pts',(-0.333052645145843,-3.20555714064656,
59.6261250060645));
#19203=CARTESIAN_POINT('Ctrl Pts',(-0.313076378368531,-3.20756977232229,
59.6273639259856));
#19204=CARTESIAN_POINT('Ctrl Pts',(-0.262072309293849,-3.21222746711234,
59.6304992915734));
#19205=CARTESIAN_POINT('Ctrl Pts',(-0.231021674373692,-3.21460982794318,
59.6323819053628));
#19206=CARTESIAN_POINT('Ctrl Pts',(-0.0805560152715602,-3.22396276634906,
59.6413991700732));
#19207=CARTESIAN_POINT('Ctrl Pts',(0.0391609941865398,-3.22473212080751,
59.6482541382956));
#19208=CARTESIAN_POINT('Ctrl Pts',(0.43886979987491,-3.20503081182403,59.6708602154157));
#19209=CARTESIAN_POINT('Ctrl Pts',(0.716061572440631,-3.15469193878349,
59.6861891204382));
#19210=CARTESIAN_POINT('Ctrl Pts',(1.03301637608063,-3.05315038340598,59.7058218783413));
#19211=CARTESIAN_POINT('Ctrl Pts',(1.08240011258963,-3.03599401084699,59.7089401750122));
#19212=CARTESIAN_POINT('Ctrl Pts',(1.16121272272251,-3.00644643952529,59.7140246722272));
#19213=CARTESIAN_POINT('Ctrl Pts',(1.19091385650328,-2.99480537843232,59.7159659508861));
#19214=CARTESIAN_POINT('Ctrl Pts',(1.25303898938089,-2.96938574951514,59.7200822291794));
#19215=CARTESIAN_POINT('Ctrl Pts',(1.28541949756136,-2.95551264542692,59.7222602062979));
#19216=CARTESIAN_POINT('Ctrl Pts',(1.36418413392361,-2.92022750926507,59.7276411218214));
#19217=CARTESIAN_POINT('Ctrl Pts',(1.41029773245226,-2.89823858354922,59.7308633404735));
#19218=CARTESIAN_POINT('Ctrl Pts',(1.63893656584088,-2.78246508563171,59.7472128487559));
#19219=CARTESIAN_POINT('Ctrl Pts',(1.81270655083574,-2.67250743335119,59.7608970333487));
#19220=CARTESIAN_POINT('Ctrl Pts',(2.12096735680935,-2.43347809547221,59.7872362977809));
#19221=CARTESIAN_POINT('Ctrl Pts',(2.25709670507903,-2.30777854232686,59.7998004278076));
#19222=CARTESIAN_POINT('Ctrl Pts',(2.40647463047983,-2.14390996659559,59.8141619193305));
#19223=CARTESIAN_POINT('Ctrl Pts',(2.43078442458745,-2.11630750052144,59.8165189672957));
#19224=CARTESIAN_POINT('Ctrl Pts',(2.46836942512819,-2.0721294217034,59.8201868595273));
#19225=CARTESIAN_POINT('Ctrl Pts',(2.48196177180597,-2.05582921992575,59.8215184242811));
#19226=CARTESIAN_POINT('Ctrl Pts',(2.50838504765398,-2.02349785094601,59.8241150723412));
#19227=CARTESIAN_POINT('Ctrl Pts',(2.52122566236738,-2.00747610250023,59.8253807760125));
#19228=CARTESIAN_POINT('Ctrl Pts',(2.5542877803926,-1.96540551653022,59.8286530477838));
#19229=CARTESIAN_POINT('Ctrl Pts',(2.57426472204498,-1.93916637770799,59.8306435928132));
#19230=CARTESIAN_POINT('Ctrl Pts',(2.61808593901863,-1.87973752235793,59.8350519563479));
#19231=CARTESIAN_POINT('Ctrl Pts',(2.64170902997236,-1.84639129742178,59.8374577640492));
#19232=CARTESIAN_POINT('Ctrl Pts',(2.71612113110418,-1.73699871641069,59.8451645108149));
#19233=CARTESIAN_POINT('Ctrl Pts',(2.76431174415411,-1.65923506117146,59.8503605265539));
#19234=CARTESIAN_POINT('Ctrl Pts',(2.93297905210031,-1.35926558431107,59.8697510245403));
#19235=CARTESIAN_POINT('Ctrl Pts',(3.03048391545008,-1.12522434000235,59.8836647266481));
#19236=CARTESIAN_POINT('Ctrl Pts',(3.11555328128316,-0.826329071483372,
59.901918998409));
#19237=CARTESIAN_POINT('Ctrl Pts',(3.12994056709405,-0.770041180393835,
59.9053722827996));
#19238=CARTESIAN_POINT('Ctrl Pts',(3.15094484383266,-0.677509049131582,
59.9110913581827));
#19239=CARTESIAN_POINT('Ctrl Pts',(3.15847575578115,-0.641484723233521,
59.9133281255906));
#19240=CARTESIAN_POINT('Ctrl Pts',(3.17205235309447,-0.570491287869983,
59.9177598819685));
#19241=CARTESIAN_POINT('Ctrl Pts',(3.17814063409056,-0.535535612651706,
59.9199531817326));
#19242=CARTESIAN_POINT('Ctrl Pts',(3.19154663989022,-0.450258705028328,
59.9253339451069));
#19243=CARTESIAN_POINT('Ctrl Pts',(3.19825272073982,-0.399852381390727,
59.9285398504902));
#19244=CARTESIAN_POINT('Ctrl Pts',(3.22400176597381,-0.163690560424752,
59.9436861980883));
#19245=CARTESIAN_POINT('Ctrl Pts',(3.2280675827124,0.0233108727131432,59.956072016989));
#19246=CARTESIAN_POINT('Ctrl Pts',(3.20247622072898,0.415987853826625,59.9825671308802));
#19247=CARTESIAN_POINT('Ctrl Pts',(3.16918513870429,0.620624948438658,59.996658636168));
#19248=CARTESIAN_POINT('Ctrl Pts',(3.10760221945617,0.854487606245626,60.0122770652714));
#19249=CARTESIAN_POINT('Ctrl Pts',(3.09814625203067,0.888161388407426,60.0145128509176));
#19250=CARTESIAN_POINT('Ctrl Pts',(3.08212434475082,0.941843968345828,60.0180489549775));
#19251=CARTESIAN_POINT('Ctrl Pts',(3.07590742140784,0.96195330177375,60.0193671516632));
#19252=CARTESIAN_POINT('Ctrl Pts',(3.06294421370395,1.00247309036875,60.0220083455839));
#19253=CARTESIAN_POINT('Ctrl Pts',(3.05618995538499,1.02287954771957,60.0233309268158));
#19254=CARTESIAN_POINT('Ctrl Pts',(3.03746359697704,1.07761502246025,60.0268618253843));
#19255=CARTESIAN_POINT('Ctrl Pts',(3.02511362905335,1.11181249018656,60.0290501400996));
#19256=CARTESIAN_POINT('Ctrl Pts',(2.99566979811199,1.18921753426789,60.0339783334769));
#19257=CARTESIAN_POINT('Ctrl Pts',(2.97821477328465,1.23227960679994,60.0367019836912));
#19258=CARTESIAN_POINT('Ctrl Pts',(2.91459243148628,1.37998062975321,60.0460295075257));
#19259=CARTESIAN_POINT('Ctrl Pts',(2.86378998912396,1.48253337704519,60.0524823778576));
#19260=CARTESIAN_POINT('Ctrl Pts',(2.70497413440088,1.76435964979148,60.0706896566574));
#19261=CARTESIAN_POINT('Ctrl Pts',(2.58482820751392,1.93610549366955,60.0823948713236));
#19262=CARTESIAN_POINT('Ctrl Pts',(2.41214944726657,2.13795423692312,60.0980315056522));
#19263=CARTESIAN_POINT('Ctrl Pts',(2.37427869853996,2.17993426077273,60.1013975765543));
#19264=CARTESIAN_POINT('Ctrl Pts',(2.31004064640055,2.24748213765211,60.1070220496124));
#19265=CARTESIAN_POINT('Ctrl Pts',(2.28430482472564,2.27363476560337,60.1092541670205));
#19266=CARTESIAN_POINT('Ctrl Pts',(2.2324062628475,2.32460311483087,60.1137179329303));
#19267=CARTESIAN_POINT('Ctrl Pts',(2.20626240307468,2.3494304433298,60.1159485948593));
#19268=CARTESIAN_POINT('Ctrl Pts',(2.14068633235918,2.4096444098886,60.1215033095447));
#19269=CARTESIAN_POINT('Ctrl Pts',(2.10078869149829,2.44450618879101,60.1248482219604));
#19270=CARTESIAN_POINT('Ctrl Pts',(1.90786010743347,2.60487098737753,60.1408718581635));
#19271=CARTESIAN_POINT('Ctrl Pts',(1.74436168343103,2.71706901506309,60.1540525438222));
#19272=CARTESIAN_POINT('Ctrl Pts',(1.43042747819915,2.89243075262105,60.1783204117256));
#19273=CARTESIAN_POINT('Ctrl Pts',(1.28349855475448,2.96055718234145,60.1893044281946));
#19274=CARTESIAN_POINT('Ctrl Pts',(1.13209532136445,3.01736271366979,60.1999356690201));
#19275=CARTESIAN_POINT('',(3.22243683749933,-0.0449265047301805,60.1999356690201));
#19276=CARTESIAN_POINT('Origin',(-1.16499385964724E-14,0.,60.1999356690201));
#19277=CARTESIAN_POINT('Ctrl Pts',(3.22243683749933,-0.0449265047301373,
60.1999356690201));
#19278=CARTESIAN_POINT('Ctrl Pts',(3.22101092976798,-0.147202380139736,
60.1936214602585));
#19279=CARTESIAN_POINT('Ctrl Pts',(3.21471055926815,-0.249479982211946,
60.1873072514969));
#19280=CARTESIAN_POINT('Ctrl Pts',(3.20354864224502,-0.351274336196089,
60.1809930427352));
#19281=CARTESIAN_POINT('Ctrl Pts',(3.19239330626173,-0.453008672470304,
60.1746825568161));
#19282=CARTESIAN_POINT('Ctrl Pts',(3.17638217460513,-0.554259925593877,
60.168372070897));
#19283=CARTESIAN_POINT('Ctrl Pts',(3.15558010482072,-0.654546991865061,
60.1620615849779));
#19284=CARTESIAN_POINT('Ctrl Pts',(3.13478544122438,-0.754798352801083,
60.1557533457894));
#19285=CARTESIAN_POINT('Ctrl Pts',(3.10920331875166,-0.854085813901753,
60.1494451066008));
#19286=CARTESIAN_POINT('Ctrl Pts',(3.07894980895765,-0.951937832224118,
60.1431368674123));
#19287=CARTESIAN_POINT('Ctrl Pts',(3.04869173594916,-1.04980460981743,60.1368276767358));
#19288=CARTESIAN_POINT('Ctrl Pts',(3.01376098015525,-1.14623512221458,60.1305184860594));
#19289=CARTESIAN_POINT('Ctrl Pts',(2.97432361185473,-1.24077258773048,60.1242092953829));
#19290=CARTESIAN_POINT('Ctrl Pts',(2.93488064524815,-1.33532347325103,60.1178992090894));
#19291=CARTESIAN_POINT('Ctrl Pts',(2.89092994848673,-1.42798040218852,60.1115891227959));
#19292=CARTESIAN_POINT('Ctrl Pts',(2.8426855484529,-1.51830709512831,60.1052790365023));
#19293=CARTESIAN_POINT('Ctrl Pts',(2.79442405525234,-1.60866579114455,60.0989667145222));
#19294=CARTESIAN_POINT('Ctrl Pts',(2.74186602143725,-1.6966922496596,60.0926543925422));
#19295=CARTESIAN_POINT('Ctrl Pts',(2.68527085912993,-1.78197586280161,60.0863420705621));
#19296=CARTESIAN_POINT('Ctrl Pts',(2.62864362117743,-1.86730781093911,60.0800261710359));
#19297=CARTESIAN_POINT('Ctrl Pts',(2.56797492387656,-1.94989348117759,60.0737102715097));
#19298=CARTESIAN_POINT('Ctrl Pts',(2.5035664258784,-2.02935278197616,60.0673943719836));
#19299=CARTESIAN_POINT('Ctrl Pts',(2.43906397980174,-2.10892798438494,60.0610692599056));
#19300=CARTESIAN_POINT('Ctrl Pts',(2.37081109528922,-2.18536739509907,60.0547441478276));
#19301=CARTESIAN_POINT('Ctrl Pts',(2.29914871747955,-2.25832520630048,60.0484190357497));
#19302=CARTESIAN_POINT('Ctrl Pts',(2.22742777450882,-2.3313426413393,60.0420887545548));
#19303=CARTESIAN_POINT('Ctrl Pts',(2.15229208193654,-2.40087253046784,60.03575847336));
#19304=CARTESIAN_POINT('Ctrl Pts',(2.0741169120997,-2.4666083186112,60.0294281921651));
#19305=CARTESIAN_POINT('Ctrl Pts',(1.99580700126858,-2.53245740750558,60.0230870002376));
#19306=CARTESIAN_POINT('Ctrl Pts',(1.91444747085521,-2.59449908689812,60.01674580831));
#19307=CARTESIAN_POINT('Ctrl Pts',(1.83044415092502,-2.65246899564243,60.0104046163824));
#19308=CARTESIAN_POINT('Ctrl Pts',(1.79520837690052,-2.67678487513901,60.007744759534));
#19309=CARTESIAN_POINT('Ctrl Pts',(1.7595077589201,-2.70038489766776,60.0050849026856));
#19310=CARTESIAN_POINT('Ctrl Pts',(1.72337351315524,-2.72325197083467,60.0024250458372));
#19311=CARTESIAN_POINT('Ctrl Pts',(1.64020134900485,-2.7758863602572,59.9963027082671));
#19312=CARTESIAN_POINT('Ctrl Pts',(1.55444527987673,-2.82481460533337,59.9901803706971));
#19313=CARTESIAN_POINT('Ctrl Pts',(1.46647257452095,-2.86976928526979,59.984058033127));
#19314=CARTESIAN_POINT('Ctrl Pts',(1.37861964988799,-2.91466275640246,59.977944031529));
#19315=CARTESIAN_POINT('Ctrl Pts',(1.28855647077179,-2.95559320632361,59.9718300299311));
#19316=CARTESIAN_POINT('Ctrl Pts',(1.19667952715909,-2.99233615621278,59.9657160283331));
#19317=CARTESIAN_POINT('Ctrl Pts',(1.10490206849107,-3.0290393205998,59.9596086470154));
#19318=CARTESIAN_POINT('Ctrl Pts',(1.01131515358769,-3.0615638277795,59.9535012656977));
#19319=CARTESIAN_POINT('Ctrl Pts',(0.916339171499791,-3.08973139370966,
59.9473938843799));
#19320=CARTESIAN_POINT('Ctrl Pts',(0.821439567103826,-3.11787630787434,
59.9412914144901));
#19321=CARTESIAN_POINT('Ctrl Pts',(0.725153537258198,-3.14167111718934,
59.9351889446002));
#19322=CARTESIAN_POINT('Ctrl Pts',(0.627919684477241,-3.16098630688999,
59.9290864747104));
#19323=CARTESIAN_POINT('Ctrl Pts',(0.530722109627871,-3.18029429009711,
59.9229862816509));
#19324=CARTESIAN_POINT('Ctrl Pts',(0.432577846179468,-3.19512588160265,
59.9168860885914));
#19325=CARTESIAN_POINT('Ctrl Pts',(0.33393795614733,-3.20540215947144,59.9107858955319));
#19326=CARTESIAN_POINT('Ctrl Pts',(0.235322441552297,-3.21567589791358,
59.9046872099241));
#19327=CARTESIAN_POINT('Ctrl Pts',(0.136211984133432,-3.2213965184783,59.8985885243163));
#19328=CARTESIAN_POINT('Ctrl Pts',(0.0370637567284713,-3.22253686409282,
59.8924898387085));
#19329=CARTESIAN_POINT('Ctrl Pts',(-0.0621272755162565,-3.22367770202387,
59.8863885201413));
#19330=CARTESIAN_POINT('Ctrl Pts',(-0.161355667492033,-3.2202343090346,
59.8802872015741));
#19331=CARTESIAN_POINT('Ctrl Pts',(-0.260163824525399,-3.21223167702897,
59.8741858830069));
#19332=CARTESIAN_POINT('Ctrl Pts',(-0.337297735829324,-3.20598447714331,
59.8694229304397));
#19333=CARTESIAN_POINT('Ctrl Pts',(-0.414175491816498,-3.19695991247447,
59.8646599778725));
#19334=CARTESIAN_POINT('Ctrl Pts',(-0.490582094296224,-3.18519179505033,
59.8598970253053));
#19335=CARTESIAN_POINT('Origin',(-9.35406549764863E-15,0.,41.4527091182931));
#19336=CARTESIAN_POINT('',(-0.490581924382687,-3.18519182122035,58.3609184893942));
#19337=CARTESIAN_POINT('',(-0.491343452670647,-3.19000126486617,58.6097459619479));
#19338=CARTESIAN_POINT('',(-0.490582094296226,-3.18519179505033,41.4527091182931));
#19339=CARTESIAN_POINT('Ctrl Pts',(-0.490581924382689,-3.18519182122035,
58.3609184893942));
#19340=CARTESIAN_POINT('Ctrl Pts',(-0.313703096115372,-3.2124346250527,
58.372562612839));
#19341=CARTESIAN_POINT('Ctrl Pts',(-0.134819049917065,-3.22490326967685,
58.3846048681688));
#19342=CARTESIAN_POINT('Ctrl Pts',(0.213309713732562,-3.22012646871349,
58.4081231419546));
#19343=CARTESIAN_POINT('Ctrl Pts',(0.381972481551577,-3.20450027907013,
58.4195482726045));
#19344=CARTESIAN_POINT('Ctrl Pts',(0.581198292875902,-3.17008165946916,
58.4325854790762));
#19345=CARTESIAN_POINT('Ctrl Pts',(0.613668753933233,-3.16395639032679,
58.4346949780006));
#19346=CARTESIAN_POINT('Ctrl Pts',(0.666140544478564,-3.15321982369106,
58.4380728141072));
#19347=CARTESIAN_POINT('Ctrl Pts',(0.686201526583494,-3.14891505444317,
58.4393567997329));
#19348=CARTESIAN_POINT('Ctrl Pts',(0.726994056028932,-3.13975325387554,
58.4419506707305));
#19349=CARTESIAN_POINT('Ctrl Pts',(0.747721116497325,-3.13488182288204,
58.4432597536929));
#19350=CARTESIAN_POINT('Ctrl Pts',(0.804152273584797,-3.12102739914996,
58.4468033048302));
#19351=CARTESIAN_POINT('Ctrl Pts',(0.83975417535615,-3.11163720365094,58.4490163528802));
#19352=CARTESIAN_POINT('Ctrl Pts',(1.05406394661899,-3.05116543984785,58.4622441253629));
#19353=CARTESIAN_POINT('Ctrl Pts',(1.22825785813371,-2.98530722730326,58.4726122106591));
#19354=CARTESIAN_POINT('Ctrl Pts',(1.57976380370304,-2.81640072209273,58.4944567086959));
#19355=CARTESIAN_POINT('Ctrl Pts',(1.75487935639104,-2.71074790002801,58.5059088620402));
#19356=CARTESIAN_POINT('Ctrl Pts',(1.96004769788926,-2.55870346551206,58.5209938996047));
#19357=CARTESIAN_POINT('Ctrl Pts',(2.000535331318,-2.52717398632152,58.5240583963101));
#19358=CARTESIAN_POINT('Ctrl Pts',(2.06766872466423,-2.47226982710916,58.5293018773251));
#19359=CARTESIAN_POINT('Ctrl Pts',(2.09471359160369,-2.44939724587851,58.5314607942696));
#19360=CARTESIAN_POINT('Ctrl Pts',(2.14878115026405,-2.40212041392816,58.5358758510144));
#19361=CARTESIAN_POINT('Ctrl Pts',(2.175778143979,-2.37769472619929,58.538132698705));
#19362=CARTESIAN_POINT('Ctrl Pts',(2.24376084273435,-2.31405952963211,58.5439547307397));
#19363=CARTESIAN_POINT('Ctrl Pts',(2.28413438119453,-2.27421716445005,58.5475464012496));
#19364=CARTESIAN_POINT('Ctrl Pts',(2.47380812468861,-2.07689122462769,58.5650924324503));
#19365=CARTESIAN_POINT('Ctrl Pts',(2.60797711574984,-1.90568436478878,58.5796528804779));
#19366=CARTESIAN_POINT('Ctrl Pts',(2.81397497938702,-1.57989297976098,58.605690530354));
#19367=CARTESIAN_POINT('Ctrl Pts',(2.89273425250105,-1.43059952526935,58.617074753674));
#19368=CARTESIAN_POINT('Ctrl Pts',(2.9725637041962,-1.24542294069209,58.6300790631077));
#19369=CARTESIAN_POINT('Ctrl Pts',(2.98519943069331,-1.21482419831584,58.6321926584));
#19370=CARTESIAN_POINT('Ctrl Pts',(3.00490376937524,-1.16494303527081,58.6355752686292));
#19371=CARTESIAN_POINT('Ctrl Pts',(3.01226327023129,-1.14577877567449,58.6368600128917));
#19372=CARTESIAN_POINT('Ctrl Pts',(3.02687619020863,-1.10661226115654,58.6394536912039));
#19373=CARTESIAN_POINT('Ctrl Pts',(3.03411559754703,-1.08660607708896,58.6407618501997));
#19374=CARTESIAN_POINT('Ctrl Pts',(3.05331303451801,-1.03186550227272,58.6442996352647));
#19375=CARTESIAN_POINT('Ctrl Pts',(3.06487652096581,-0.996995019063621,
58.6465079617242));
#19376=CARTESIAN_POINT('Ctrl Pts',(3.13197827491077,-0.782432865897649,
58.6598637329304));
#19377=CARTESIAN_POINT('Ctrl Pts',(3.1723005566129,-0.598342716944537,58.6703478981932));
#19378=CARTESIAN_POINT('Ctrl Pts',(3.21360917368962,-0.277687063164398,
58.6884580376908));
#19379=CARTESIAN_POINT('Ctrl Pts',(3.22242778506983,-0.142655399222014,
58.6960374992979));
#19380=CARTESIAN_POINT('Ctrl Pts',(3.22288686970446,0.0552716915044153,
58.7074246911002));
#19381=CARTESIAN_POINT('Ctrl Pts',(3.22119986485595,0.118006423353004,58.7110735185706));
#19382=CARTESIAN_POINT('Ctrl Pts',(3.21470368769381,0.233714683625658,58.7179076176479));
#19383=CARTESIAN_POINT('Ctrl Pts',(3.21041235565451,0.286695625514143,58.7210773041909));
#19384=CARTESIAN_POINT('Ctrl Pts',(3.20104688015028,0.375092387262804,58.7264463301134));
#19385=CARTESIAN_POINT('Ctrl Pts',(3.19668952831531,0.410574389751162,58.7286232146917));
#19386=CARTESIAN_POINT('Ctrl Pts',(3.18676008106815,0.481637134299323,58.7330302380956));
#19387=CARTESIAN_POINT('Ctrl Pts',(3.18118000159674,0.517211537622918,58.73526033297));
#19388=CARTESIAN_POINT('Ctrl Pts',(3.16564581402951,0.606450845601025,58.7409178973475));
#19389=CARTESIAN_POINT('Ctrl Pts',(3.15492264806733,0.659968603768021,58.7443689196773));
#19390=CARTESIAN_POINT('Ctrl Pts',(3.0904039427137,0.944287735587318,58.7630245002923));
#19391=CARTESIAN_POINT('Ctrl Pts',(3.012638488592,1.16886749148693,58.778978712579));
#19392=CARTESIAN_POINT('Ctrl Pts',(2.86589720070745,1.47776576619269,58.8020718155961));
#19393=CARTESIAN_POINT('Ctrl Pts',(2.8161933034815,1.57041895640225,58.809149752206));
#19394=CARTESIAN_POINT('Ctrl Pts',(2.73925132808562,1.69840443070662,58.819010996101));
#19395=CARTESIAN_POINT('Ctrl Pts',(2.71567342796502,1.73585530465207,58.8219070249988));
#19396=CARTESIAN_POINT('Ctrl Pts',(2.67209378292484,1.80201423519084,58.8270267075113));
#19397=CARTESIAN_POINT('Ctrl Pts',(2.65238186747647,1.83090446134634,58.8292636553493));
#19398=CARTESIAN_POINT('Ctrl Pts',(2.620137009386,1.87654920395239,58.8327928304405));
#19399=CARTESIAN_POINT('Ctrl Pts',(2.60790496625729,1.89351171276184,58.8341031935381));
#19400=CARTESIAN_POINT('Ctrl Pts',(2.58465020071729,1.92510686271911,58.8365399138185));
#19401=CARTESIAN_POINT('Ctrl Pts',(2.57366623696074,1.93976679802404,58.8376688721513));
#19402=CARTESIAN_POINT('Ctrl Pts',(2.54314933710594,1.97978112793534,58.8407481869553));
#19403=CARTESIAN_POINT('Ctrl Pts',(2.52336225329173,2.0049401436542,58.8426818712912));
#19404=CARTESIAN_POINT('Ctrl Pts',(2.42079999360231,2.13142254425649,58.8524144159525));
#19405=CARTESIAN_POINT('Ctrl Pts',(2.33227658365501,2.22794244886292,58.8598816318094));
#19406=CARTESIAN_POINT('Ctrl Pts',(2.10863837172773,2.44379763223764,58.8774036577988));
#19407=CARTESIAN_POINT('Ctrl Pts',(1.96891793083494,2.55770682443238,58.8873598692556));
#19408=CARTESIAN_POINT('Ctrl Pts',(1.7608040979732,2.7001677802958,58.9017692453151));
#19409=CARTESIAN_POINT('Ctrl Pts',(1.69983507276302,2.73895909531567,58.90594231409));
#19410=CARTESIAN_POINT('Ctrl Pts',(1.58686718293911,2.8056090446986,58.9136387510404));
#19411=CARTESIAN_POINT('Ctrl Pts',(1.53530869790419,2.83415174864578,58.9171384361721));
#19412=CARTESIAN_POINT('Ctrl Pts',(1.4502967543022,2.878213615928,58.922905928523));
#19413=CARTESIAN_POINT('Ctrl Pts',(1.41730736223012,2.89460082980786,58.925143267815));
#19414=CARTESIAN_POINT('Ctrl Pts',(1.35264234208755,2.9253521874344,58.9295311237942));
#19415=CARTESIAN_POINT('Ctrl Pts',(1.32100070407811,2.93977613376806,58.9316792036037));
#19416=CARTESIAN_POINT('Ctrl Pts',(1.25092893156231,2.97035888933485,58.9364410058048));
#19417=CARTESIAN_POINT('Ctrl Pts',(1.21240664442007,2.98628950270077,58.9390619602566));
#19418=CARTESIAN_POINT('Ctrl Pts',(1.07042996233498,3.04180303056521,58.9487370813451));
#19419=CARTESIAN_POINT('Ctrl Pts',(0.965271876809903,3.07678920455712,58.955936110015));
#19420=CARTESIAN_POINT('Ctrl Pts',(0.838364585865782,3.1118644117633,58.964647882717));
#19421=CARTESIAN_POINT('Ctrl Pts',(0.81814502216379,3.11724140811213,58.9660364571504));
#19422=CARTESIAN_POINT('Ctrl Pts',(0.606425175934186,3.17134235218727,58.98057932777));
#19423=CARTESIAN_POINT('Ctrl Pts',(0.410893209371642,3.20254979908285,58.9940719396457));
#19424=CARTESIAN_POINT('Ctrl Pts',(0.153388597667511,3.2196658143404,59.0112982136109));
#19425=CARTESIAN_POINT('Ctrl Pts',(0.0929324324061976,3.22197770424125,
59.0153009342391));
#19426=CARTESIAN_POINT('Ctrl Pts',(-0.0114722981714657,3.2230288239894,
59.0221058586023));
#19427=CARTESIAN_POINT('Ctrl Pts',(-0.0553956913796581,3.22257321959653,
59.0249358098143));
#19428=CARTESIAN_POINT('Ctrl Pts',(-0.121995253913166,3.22052020007587,
59.0291636161899));
#19429=CARTESIAN_POINT('Ctrl Pts',(-0.144684904973048,3.21958064813989,
59.0305928363602));
#19430=CARTESIAN_POINT('Ctrl Pts',(-0.18712917660364,3.21737345867217,59.0332431856965));
#19431=CARTESIAN_POINT('Ctrl Pts',(-0.206883956676711,3.21616360679244,
59.034467032317));
#19432=CARTESIAN_POINT('Ctrl Pts',(-0.25090510005703,3.21306030319763,59.0371743808418));
#19433=CARTESIAN_POINT('Ctrl Pts',(-0.275163111547384,3.21107384279669,
59.0386529471544));
#19434=CARTESIAN_POINT('Ctrl Pts',(-0.365898148618014,3.20260784299262,
59.0441411750631));
#19435=CARTESIAN_POINT('Ctrl Pts',(-0.432195005777373,3.19433673544487,
59.0480663330513));
#19436=CARTESIAN_POINT('Ctrl Pts',(-0.693620149646696,3.15343243308761,
59.0633727922369));
#19437=CARTESIAN_POINT('Ctrl Pts',(-0.88582981802671,3.10492519762998,59.0742680308405));
#19438=CARTESIAN_POINT('Ctrl Pts',(-1.16822794358344,3.00527703844516,59.0911344287984));
#19439=CARTESIAN_POINT('Ctrl Pts',(-1.26241005717512,2.96694549572378,59.0969092347154));
#19440=CARTESIAN_POINT('Ctrl Pts',(-1.42252883533251,2.89277212603626,59.1071465043538));
#19441=CARTESIAN_POINT('Ctrl Pts',(-1.48931755300562,2.85895975226926,59.1115499560623));
#19442=CARTESIAN_POINT('Ctrl Pts',(-1.58971711902455,2.80365835931714,59.1184151583117));
#19443=CARTESIAN_POINT('Ctrl Pts',(-1.62420901905247,2.78381852207022,59.1208197310163));
#19444=CARTESIAN_POINT('Ctrl Pts',(-1.68774326791549,2.74569070394599,59.1253405507286));
#19445=CARTESIAN_POINT('Ctrl Pts',(-1.71687812658293,2.72756743929242,59.1274506245945));
#19446=CARTESIAN_POINT('Ctrl Pts',(-1.78206279698645,2.68556126875977,59.1322587111041));
#19447=CARTESIAN_POINT('Ctrl Pts',(-1.81793183235876,2.6614114121675,59.1349663351169));
#19448=CARTESIAN_POINT('Ctrl Pts',(-1.93193576583333,2.58127488488144,59.1437788676825));
#19449=CARTESIAN_POINT('Ctrl Pts',(-2.00804961445334,2.52251652644894,59.1499858383815));
#19450=CARTESIAN_POINT('Ctrl Pts',(-2.19784622960557,2.36195797922543,59.1663176417798));
#19451=CARTESIAN_POINT('Ctrl Pts',(-2.30712753929267,2.25533352930772,59.1765917799252));
#19452=CARTESIAN_POINT('Ctrl Pts',(-2.51270917982429,2.02411316306989,59.1974927171383));
#19453=CARTESIAN_POINT('Ctrl Pts',(-2.60827955554223,1.89937527874125,59.208092588991));
#19454=CARTESIAN_POINT('Ctrl Pts',(-2.71595262172634,1.73529940296152,59.2208316499056));
#19455=CARTESIAN_POINT('Ctrl Pts',(-2.73691689645245,1.70204256057179,59.2233556851422));
#19456=CARTESIAN_POINT('Ctrl Pts',(-2.76854989788951,1.64976480029569,59.2272242952187));
#19457=CARTESIAN_POINT('Ctrl Pts',(-2.7796423029921,1.63100618146715,59.2285930901741));
#19458=CARTESIAN_POINT('Ctrl Pts',(-2.80063906359022,1.59466161282985,59.2312058931905));
#19459=CARTESIAN_POINT('Ctrl Pts',(-2.81056989382123,1.57709280511396,59.2324513482967));
#19460=CARTESIAN_POINT('Ctrl Pts',(-2.83547732451168,1.5320460674253,59.2356029189787));
#19461=CARTESIAN_POINT('Ctrl Pts',(-2.85022039138348,1.50444032662634,59.2374951572292));
#19462=CARTESIAN_POINT('Ctrl Pts',(-2.9197415106292,1.36957355175137,59.2465726321053));
#19463=CARTESIAN_POINT('Ctrl Pts',(-2.96888494376337,1.25950390291113,59.2534767143923));
#19464=CARTESIAN_POINT('Ctrl Pts',(-3.11044237894284,0.887784916053613,
59.275959742021));
#19465=CARTESIAN_POINT('Ctrl Pts',(-3.17526602581569,0.617005136844247,
59.2911396651945));
#19466=CARTESIAN_POINT('Ctrl Pts',(-3.21022110947204,0.288766173036444,
59.3106123424897));
#19467=CARTESIAN_POINT('Ctrl Pts',(-3.21452098042975,0.236135282172697,
59.3137622071998));
#19468=CARTESIAN_POINT('Ctrl Pts',(-3.21935478132504,0.151343617337449,
59.3188930054627));
#19469=CARTESIAN_POINT('Ctrl Pts',(-3.22070369453345,0.11923798067955,59.3208486068182));
#19470=CARTESIAN_POINT('Ctrl Pts',(-3.22253010664521,0.0516986523011541,
59.3249921676658));
#19471=CARTESIAN_POINT('Ctrl Pts',(-3.22290370253146,0.0162666845945092,
59.3271830733254));
#19472=CARTESIAN_POINT('Ctrl Pts',(-3.22238791594585,-0.0704737995444062,
59.3325914541781));
#19473=CARTESIAN_POINT('Ctrl Pts',(-3.2208574442024,-0.121767328821068,
59.335828199242));
#19474=CARTESIAN_POINT('Ctrl Pts',(-3.20712032331414,-0.377301517376942,
59.3521539036567));
#19475=CARTESIAN_POINT('Ctrl Pts',(-3.1767091700218,-0.580062455399293,
59.365791885938));
#19476=CARTESIAN_POINT('Ctrl Pts',(-3.08256721426357,-0.958217421897955,
59.3920923054007));
#19477=CARTESIAN_POINT('Ctrl Pts',(-3.02243315722774,-1.13371434719622,
59.4046654065589));
#19478=CARTESIAN_POINT('Ctrl Pts',(-2.93265848917949,-1.33678318485918,
59.4190411984297));
#19479=CARTESIAN_POINT('Ctrl Pts',(-2.91718316834908,-1.37022542796239,
59.4214019132187));
#19480=CARTESIAN_POINT('Ctrl Pts',(-2.89185638029371,-1.42258161000561,
59.425078818019));
#19481=CARTESIAN_POINT('Ctrl Pts',(-2.88238538007774,-1.44167483905053,
59.426415653761));
#19482=CARTESIAN_POINT('Ctrl Pts',(-2.86339215993269,-1.47902905396084,
59.4290209915457));
#19483=CARTESIAN_POINT('Ctrl Pts',(-2.8538830477831,-1.49729529171775,59.4302901016983));
#19484=CARTESIAN_POINT('Ctrl Pts',(-2.82857976978781,-1.54478391707973,
59.4335798930614));
#19485=CARTESIAN_POINT('Ctrl Pts',(-2.81250728646633,-1.57385635361129,
59.4355842605114));
#19486=CARTESIAN_POINT('Ctrl Pts',(-2.77546245002854,-1.6384838121772,59.440029870302));
#19487=CARTESIAN_POINT('Ctrl Pts',(-2.75425054015925,-1.67389523808841,
59.4424587868245));
#19488=CARTESIAN_POINT('Ctrl Pts',(-2.6829884315633,-1.78783696300309,59.4502834191538));
#19489=CARTESIAN_POINT('Ctrl Pts',(-2.63021234622076,-1.86461064868825,
59.4555710001201));
#19490=CARTESIAN_POINT('Ctrl Pts',(-2.41650882681915,-2.14832051555247,
59.4755791294502));
#19491=CARTESIAN_POINT('Ctrl Pts',(-2.23390724096757,-2.33761537859557,
59.4900236324999));
#19492=CARTESIAN_POINT('Ctrl Pts',(-1.99087765978373,-2.53478097948101,
59.5085210285756));
#19493=CARTESIAN_POINT('Ctrl Pts',(-1.95059670433833,-2.56590735306645,
59.5115624673259));
#19494=CARTESIAN_POINT('Ctrl Pts',(-1.88136348061117,-2.61683347962296,
59.5167606006669));
#19495=CARTESIAN_POINT('Ctrl Pts',(-1.85279384056996,-2.63713876040281,
59.5188975074895));
#19496=CARTESIAN_POINT('Ctrl Pts',(-1.79378185994841,-2.67764798155062,
59.5232981600596));
#19497=CARTESIAN_POINT('Ctrl Pts',(-1.76331584096983,-2.69780821145064,
59.5255631217287));
#19498=CARTESIAN_POINT('Ctrl Pts',(-1.68435682414545,-2.74814874305156,
59.5314187549751));
#19499=CARTESIAN_POINT('Ctrl Pts',(-1.63539393730862,-2.77756465969716,
59.5350363680787));
#19500=CARTESIAN_POINT('Ctrl Pts',(-1.4402809663901,-2.8878367470472,59.549407630889));
#19501=CARTESIAN_POINT('Ctrl Pts',(-1.28873492577402,-2.95857393868106,
59.5604920753131));
#19502=CARTESIAN_POINT('Ctrl Pts',(-0.938560002642515,-3.08999894691175,
59.5856742768592));
#19503=CARTESIAN_POINT('Ctrl Pts',(-0.73814310172579,-3.1439054014834,59.599808555615));
#19504=CARTESIAN_POINT('Ctrl Pts',(-0.519498516188417,-3.18063721291414,
59.6141969279335));
#19505=CARTESIAN_POINT('Ctrl Pts',(-0.505047975621658,-3.18296376521452,
59.6151429755576));
#19506=CARTESIAN_POINT('Ctrl Pts',(-0.490582094004581,-3.18519179509525,
59.6160848123881));
#19507=CARTESIAN_POINT('',(-3.22274929773161,-0.00212755034421634,59.5777091182932));
#19508=CARTESIAN_POINT('Ctrl Pts',(-0.490582094296224,-3.18519179505033,
59.8598970253053));
#19509=CARTESIAN_POINT('Ctrl Pts',(-0.588567220510107,-3.17010016116424,
59.8537889339454));
#19510=CARTESIAN_POINT('Ctrl Pts',(-0.685776785759724,-3.15049492155716,
59.8476808425855));
#19511=CARTESIAN_POINT('Ctrl Pts',(-0.781768325518016,-3.12649257918786,
59.8415727512256));
#19512=CARTESIAN_POINT('Ctrl Pts',(-0.877926813432343,-3.10244849202721,
59.8354540366942));
#19513=CARTESIAN_POINT('Ctrl Pts',(-0.972862618905612,-3.07399214979295,
59.8293353221628));
#19514=CARTESIAN_POINT('Ctrl Pts',(-1.06614928443358,-3.0412897372335,59.8232166076314));
#19515=CARTESIAN_POINT('Ctrl Pts',(-1.15916173008287,-3.00868345472172,
59.8171158793057));
#19516=CARTESIAN_POINT('Ctrl Pts',(-1.25053434997069,-2.97185627268983,
59.81101515098));
#19517=CARTESIAN_POINT('Ctrl Pts',(-1.33986848452895,-2.93101859541459,
59.8049144226543));
#19518=CARTESIAN_POINT('Ctrl Pts',(-1.43040172758154,-2.88963276478283,
59.7987318058636));
#19519=CARTESIAN_POINT('Ctrl Pts',(-1.5191708502785,-2.84397750535809,59.7925491890728));
#19520=CARTESIAN_POINT('Ctrl Pts',(-1.60574627620447,-2.79422555620614,
59.786366572282));
#19521=CARTESIAN_POINT('Ctrl Pts',(-1.69220561574934,-2.74454031794436,
59.7801922455759));
#19522=CARTESIAN_POINT('Ctrl Pts',(-1.77647673364627,-2.69076952301357,
59.7740179188698));
#19523=CARTESIAN_POINT('Ctrl Pts',(-1.85815124673768,-2.63313340086431,
59.7678435921637));
#19524=CARTESIAN_POINT('Ctrl Pts',(-1.93974013763877,-2.57555770063658,
59.7616757382158));
#19525=CARTESIAN_POINT('Ctrl Pts',(-2.01873748447073,-2.51412497820492,
59.7555078842679));
#19526=CARTESIAN_POINT('Ctrl Pts',(-2.09476151080866,-2.44910019707947,
59.74934003032));
#19527=CARTESIAN_POINT('Ctrl Pts',(-2.17073027706268,-2.38412268094423,
59.7431766596407));
#19528=CARTESIAN_POINT('Ctrl Pts',(-2.24372969248937,-2.31555857830692,
59.7370132889614));
#19529=CARTESIAN_POINT('Ctrl Pts',(-2.31340960483721,-2.24371423375326,
59.730849918282));
#19530=CARTESIAN_POINT('Ctrl Pts',(-2.38306332949095,-2.17189689034893,
59.7246888639728));
#19531=CARTESIAN_POINT('Ctrl Pts',(-2.44939972943618,-2.09680206519114,
59.7185278096636));
#19532=CARTESIAN_POINT('Ctrl Pts',(-2.51210483965493,-2.01877359728185,
59.7123667553544));
#19533=CARTESIAN_POINT('Ctrl Pts',(-2.57480299288723,-1.94075378645,59.7062063845998));
#19534=CARTESIAN_POINT('Ctrl Pts',(-2.63387038655929,-1.85980131735224,
59.7000460138453));
#19535=CARTESIAN_POINT('Ctrl Pts',(-2.68903339717869,-1.77629303645477,
59.6938856430907));
#19536=CARTESIAN_POINT('Ctrl Pts',(-2.74420489893484,-1.69277190128729,
59.6877243240821));
#19537=CARTESIAN_POINT('Ctrl Pts',(-2.79547058542601,-1.60669453391276,
59.6815630050734));
#19538=CARTESIAN_POINT('Ctrl Pts',(-2.84260075887082,-1.5184658337174,59.6754016860648));
#19539=CARTESIAN_POINT('Ctrl Pts',(-2.88977971480695,-1.4301458116472,59.6692339897299));
#19540=CARTESIAN_POINT('Ctrl Pts',(-2.93281440624732,-1.33967039270124,
59.6630662933951));
#19541=CARTESIAN_POINT('Ctrl Pts',(-2.97152169936721,-1.24746797661899,
59.6568985970602));
#19542=CARTESIAN_POINT('Ctrl Pts',(-3.01025038863967,-1.15521459399263,
59.6507274914202));
#19543=CARTESIAN_POINT('Ctrl Pts',(-3.04464676656595,-1.06123271913011,
59.6445563857803));
#19544=CARTESIAN_POINT('Ctrl Pts',(-3.07457705306434,-0.965967653325046,
59.6383852801403));
#19545=CARTESIAN_POINT('Ctrl Pts',(-3.10455510623962,-0.870550551032845,
59.6322043258406));
#19546=CARTESIAN_POINT('Ctrl Pts',(-3.13005272184961,-0.773846585983105,
59.6260233715408));
#19547=CARTESIAN_POINT('Ctrl Pts',(-3.15098685273959,-0.676313105271749,
59.6198424172411));
#19548=CARTESIAN_POINT('Ctrl Pts',(-3.16502954150311,-0.610887302746178,
59.6156962113179));
#19549=CARTESIAN_POINT('Ctrl Pts',(-3.17701983363642,-0.545088434709207,
59.6115500053947));
#19550=CARTESIAN_POINT('Ctrl Pts',(-3.18694576623428,-0.479055576714712,
59.6074037994715));
#19551=CARTESIAN_POINT('Ctrl Pts',(-3.21064192036897,-0.321415499516386,
59.597505572412));
#19552=CARTESIAN_POINT('Ctrl Pts',(-3.22264376531188,-0.161984886987291,
59.5876073453526));
#19553=CARTESIAN_POINT('Ctrl Pts',(-3.22274929773161,-0.00212755034421634,
59.5777091182932));
#19554=CARTESIAN_POINT('Ctrl Pts',(-3.22515705657206,-0.00210809394305351,
59.5777078161216));
#19555=CARTESIAN_POINT('Ctrl Pts',(-3.21756318232272,0.901980015450162,
59.5217696028439));
#19556=CARTESIAN_POINT('Ctrl Pts',(-2.35196096173306,2.88200781430396,59.3999945151719));
#19557=CARTESIAN_POINT('Ctrl Pts',(0.998193681065493,3.67000140801024,59.2123825531058));
#19558=CARTESIAN_POINT('Ctrl Pts',(3.61883085014894,1.16896682075721,59.0148719299228));
#19559=CARTESIAN_POINT('Ctrl Pts',(2.95640798566869,-2.39226680571159,58.81736130674));
#19560=CARTESIAN_POINT('Ctrl Pts',(0.669413081115714,-3.34327461681512,
58.6823193174151));
#19561=CARTESIAN_POINT('Ctrl Pts',(-0.437675410847414,-3.19850339953065,
58.6131142024843));
#19562=CARTESIAN_POINT('Ctrl Pts',(-0.491343452670647,-3.19000126486617,
58.6097459619479));
#19563=CARTESIAN_POINT('Origin',(-9.35406549764863E-15,0.,41.4527091182931));
#19564=CARTESIAN_POINT('',(-0.49058180811571,-3.18519183912774,57.1123311812828));
#19565=CARTESIAN_POINT('',(-0.490582240097165,-3.18519177259412,57.3619600447814));
#19566=CARTESIAN_POINT('',(-0.490582094296226,-3.18519179505033,41.4527091182931));
#19567=CARTESIAN_POINT('',(-3.22274878421801,0.00279934303327976,58.081859847365));
#19568=CARTESIAN_POINT('Ctrl Pts',(-0.490581808115708,-3.18519183912774,
57.1123311812828));
#19569=CARTESIAN_POINT('Ctrl Pts',(-0.363519266685327,-3.20476195435689,
57.1195896121718));
#19570=CARTESIAN_POINT('Ctrl Pts',(-0.235300550620664,-3.21672691832773,
57.126950618447));
#19571=CARTESIAN_POINT('Ctrl Pts',(-0.0531215777745777,-3.22275646010443,
57.1376960522343));
#19572=CARTESIAN_POINT('Ctrl Pts',(0.000394523536829932,-3.22319413942321,
57.140886515961));
#19573=CARTESIAN_POINT('Ctrl Pts',(0.086128815411882,-3.22176019097727,
57.1460645706055));
#19574=CARTESIAN_POINT('Ctrl Pts',(0.118352235991067,-3.22073742078687,
57.148025852026));
#19575=CARTESIAN_POINT('Ctrl Pts',(0.185817376770669,-3.2175822738534,57.1521664065113));
#19576=CARTESIAN_POINT('Ctrl Pts',(0.221050091166339,-3.21535386658781,
57.1543483955745));
#19577=CARTESIAN_POINT('Ctrl Pts',(0.306693210253217,-3.2085228313182,57.1597030759785));
#19578=CARTESIAN_POINT('Ctrl Pts',(0.35704415803387,-3.20331055208824,57.1628941814196));
#19579=CARTESIAN_POINT('Ctrl Pts',(0.588399476729501,-3.17383860920283,
57.1777633587442));
#19580=CARTESIAN_POINT('Ctrl Pts',(0.767234648021058,-3.13541050638952,
57.1898690476116));
#19581=CARTESIAN_POINT('Ctrl Pts',(1.14335297295845,-3.02047431222032,57.2163549205064));
#19582=CARTESIAN_POINT('Ctrl Pts',(1.33835832866908,-2.939273283835,57.2307398731188));
#19583=CARTESIAN_POINT('Ctrl Pts',(1.55560851429715,-2.82267297650291,57.2466884357191));
#19584=CARTESIAN_POINT('Ctrl Pts',(1.58688632482501,-2.80520812392022,57.2489814973636));
#19585=CARTESIAN_POINT('Ctrl Pts',(1.63610451452224,-2.77663901318277,57.2525772636646));
#19586=CARTESIAN_POINT('Ctrl Pts',(1.65423740809246,-2.76587433689308,57.2538992418942));
#19587=CARTESIAN_POINT('Ctrl Pts',(1.68994586731178,-2.74419904129099,57.2564950470604));
#19588=CARTESIAN_POINT('Ctrl Pts',(1.70752451203387,-2.73329572064327,57.2577691746616));
#19589=CARTESIAN_POINT('Ctrl Pts',(1.75361087552491,-2.7040920738317,57.2611029858357));
#19590=CARTESIAN_POINT('Ctrl Pts',(1.78193797792735,-2.68550968985088,57.2631453791153));
#19591=CARTESIAN_POINT('Ctrl Pts',(1.94734533430325,-2.57323370755409,57.2750638598141));
#19592=CARTESIAN_POINT('Ctrl Pts',(2.07732683492534,-2.4694961026689,57.2844072039961));
#19593=CARTESIAN_POINT('Ctrl Pts',(2.35823966240032,-2.20735460217788,57.3059475879948));
#19594=CARTESIAN_POINT('Ctrl Pts',(2.50219601326392,-2.04272224416803,57.3180941750521));
#19595=CARTESIAN_POINT('Ctrl Pts',(2.66117883123958,-1.81863976646521,57.3342465664888));
#19596=CARTESIAN_POINT('Ctrl Pts',(2.69271724329053,-1.77160849232256,57.3376146691767));
#19597=CARTESIAN_POINT('Ctrl Pts',(2.74246304998617,-1.69302633623517,57.3432223880811));
#19598=CARTESIAN_POINT('Ctrl Pts',(2.76140411902098,-1.6619533330701,57.3454348191831));
#19599=CARTESIAN_POINT('Ctrl Pts',(2.79774321602195,-1.60000191844197,57.3498397290469));
#19600=CARTESIAN_POINT('Ctrl Pts',(2.81516609456666,-1.56914401621594,57.3520309055797));
#19601=CARTESIAN_POINT('Ctrl Pts',(2.85660363979631,-1.49284114252743,57.3574449397183));
#19602=CARTESIAN_POINT('Ctrl Pts',(2.88004607694429,-1.44709818075665,57.3606871970129));
#19603=CARTESIAN_POINT('Ctrl Pts',(2.99206482870654,-1.21500392724573,57.3771299233356));
#19604=CARTESIAN_POINT('Ctrl Pts',(3.06368188208961,-1.02103655511887,57.3908900278049));
#19605=CARTESIAN_POINT('Ctrl Pts',(3.16298229078933,-0.644392258938267,
57.417183776433));
#19606=CARTESIAN_POINT('Ctrl Pts',(3.19450366314214,-0.463523224311926,
57.4296237777371));
#19607=CARTESIAN_POINT('Ctrl Pts',(3.21369957739114,-0.244163597585218,
57.4438832688859));
#19608=CARTESIAN_POINT('Ctrl Pts',(3.21628613982045,-0.207327201106171,
57.446249287105));
#19609=CARTESIAN_POINT('Ctrl Pts',(3.21936648206036,-0.149168692678552,
57.4499316091332));
#19610=CARTESIAN_POINT('Ctrl Pts',(3.22028264788585,-0.127873265124269,
57.4512686983814));
#19611=CARTESIAN_POINT('Ctrl Pts',(3.22166541011702,-0.0860803088763244,
57.4538686960056));
#19612=CARTESIAN_POINT('Ctrl Pts',(3.22214781228551,-0.0655846227731079,
57.4551322850543));
#19613=CARTESIAN_POINT('Ctrl Pts',(3.22289569486623,-0.0121303332849647,
57.4584010521021));
#19614=CARTESIAN_POINT('Ctrl Pts',(3.22285123074699,0.0208312194294717,
57.4603901734727));
#19615=CARTESIAN_POINT('Ctrl Pts',(3.21946010656653,0.223985875842655,57.4725180470774));
#19616=CARTESIAN_POINT('Ctrl Pts',(3.20313865414242,0.393711827527747,57.4820887489451));
#19617=CARTESIAN_POINT('Ctrl Pts',(3.13598090366949,0.77336166160849,57.5036993069403));
#19618=CARTESIAN_POINT('Ctrl Pts',(3.07733795816236,0.981043346933699,57.5156948280978));
#19619=CARTESIAN_POINT('Ctrl Pts',(2.97759373200925,1.23421434138993,57.5316888541461));
#19620=CARTESIAN_POINT('Ctrl Pts',(2.9553601140516,1.2865440115326,57.5350700945385));
#19621=CARTESIAN_POINT('Ctrl Pts',(2.91662626969095,1.37139932984,57.5406936963356));
#19622=CARTESIAN_POINT('Ctrl Pts',(2.90093697063014,1.40428253743463,57.5429085490009));
#19623=CARTESIAN_POINT('Ctrl Pts',(2.86890856587276,1.4685825459715,57.5473138388743));
#19624=CARTESIAN_POINT('Ctrl Pts',(2.85260244524963,1.50001006172084,57.5495028966313));
#19625=CARTESIAN_POINT('Ctrl Pts',(2.81144881726522,1.57622849126425,57.5549033243697));
#19626=CARTESIAN_POINT('Ctrl Pts',(2.78604558587402,1.62070670556981,57.5581338672329));
#19627=CARTESIAN_POINT('Ctrl Pts',(2.65368110125754,1.84014761399111,57.5744817918008));
#19628=CARTESIAN_POINT('Ctrl Pts',(2.53126682652806,2.00520100772327,57.5881517712879));
#19629=CARTESIAN_POINT('Ctrl Pts',(2.27013744495275,2.2949600152189,57.6144797810067));
#19630=CARTESIAN_POINT('Ctrl Pts',(2.13462777313359,2.42151583033966,57.6270474072483));
#19631=CARTESIAN_POINT('Ctrl Pts',(1.96001051197897,2.55848265217056,57.6414175725839));
#19632=CARTESIAN_POINT('Ctrl Pts',(1.93063529101231,2.5807212800703,57.6437780771931));
#19633=CARTESIAN_POINT('Ctrl Pts',(1.88368612655658,2.61501389902058,57.6474538659723));
#19634=CARTESIAN_POINT('Ctrl Pts',(1.86636377332607,2.62740507734548,57.6487898198236));
#19635=CARTESIAN_POINT('Ctrl Pts',(1.83211736628624,2.65139290376272,57.6513894626546));
#19636=CARTESIAN_POINT('Ctrl Pts',(1.81520314212203,2.66300130681889,57.6526538040951));
#19637=CARTESIAN_POINT('Ctrl Pts',(1.77077340573991,2.69287387244312,57.6559272391761));
#19638=CARTESIAN_POINT('Ctrl Pts',(1.74308512396861,2.71087856409127,57.6579201886513));
#19639=CARTESIAN_POINT('Ctrl Pts',(1.68043072432765,2.75026350591833,57.6623371249689));
#19640=CARTESIAN_POINT('Ctrl Pts',(1.64532336772238,2.77140904136289,57.6647489552529));
#19641=CARTESIAN_POINT('Ctrl Pts',(1.53007546459174,2.83786192085284,57.6724952171617));
#19642=CARTESIAN_POINT('Ctrl Pts',(1.44839199149357,2.88040860677375,57.6777232160301));
#19643=CARTESIAN_POINT('Ctrl Pts',(1.13351642074583,3.02763176556984,57.6973004500824));
#19644=CARTESIAN_POINT('Ctrl Pts',(0.89000703225663,3.10794045130935,57.7113713746647));
#19645=CARTESIAN_POINT('Ctrl Pts',(0.585365619488878,3.1696251382868,57.729665176306));
#19646=CARTESIAN_POINT('Ctrl Pts',(0.53088770096092,3.17920338149255,57.7329582698494));
#19647=CARTESIAN_POINT('Ctrl Pts',(0.440445945405425,3.19271534501132,57.7384754743614));
#19648=CARTESIAN_POINT('Ctrl Pts',(0.404613181634699,3.19745397395242,57.7406742230626));
#19649=CARTESIAN_POINT('Ctrl Pts',(0.333315922573735,3.20566488727956,57.745078103364));
#19650=CARTESIAN_POINT('Ctrl Pts',(0.297858486792379,3.20915363215339,57.7472823869861));
#19651=CARTESIAN_POINT('Ctrl Pts',(0.210041500496304,3.21632627861556,57.7527795916799));
#19652=CARTESIAN_POINT('Ctrl Pts',(0.157637461614142,3.2193201271046,57.7560933098251));
#19653=CARTESIAN_POINT('Ctrl Pts',(-0.0917388816373725,3.22746375842088,
57.7720288896367));
#19654=CARTESIAN_POINT('Ctrl Pts',(-0.288810206972034,3.21582118715856,
57.7851517432284));
#19655=CARTESIAN_POINT('Ctrl Pts',(-0.672175759190451,3.1576405591133,57.8113142293623));
#19656=CARTESIAN_POINT('Ctrl Pts',(-0.857891958734288,3.11232146478025,
57.8242851999409));
#19657=CARTESIAN_POINT('Ctrl Pts',(-1.07313730631409,3.03905105567359,57.8390041155607));
#19658=CARTESIAN_POINT('Ctrl Pts',(-1.10755602583907,3.0266772053551,57.8413468780503));
#19659=CARTESIAN_POINT('Ctrl Pts',(-1.16162207360763,3.0061940929379,57.8450016315258));
#19660=CARTESIAN_POINT('Ctrl Pts',(-1.18141165373373,2.99847216590604,57.8463339214628));
#19661=CARTESIAN_POINT('Ctrl Pts',(-1.22019903013725,2.98289363506496,57.8489324080083));
#19662=CARTESIAN_POINT('Ctrl Pts',(-1.23920062974529,2.97504990648184,57.8501991662501));
#19663=CARTESIAN_POINT('Ctrl Pts',(-1.28872644456465,2.95404916140932,57.8534877198561));
#19664=CARTESIAN_POINT('Ctrl Pts',(-1.31912538154011,2.94060040117383,57.8554930848966));
#19665=CARTESIAN_POINT('Ctrl Pts',(-1.38684799971036,2.90937770132362,57.8599426936834));
#19666=CARTESIAN_POINT('Ctrl Pts',(-1.4240491136981,2.89135096434638,57.8623744997194));
#19667=CARTESIAN_POINT('Ctrl Pts',(-1.54415575708393,2.83026958342802,57.8702172436427));
#19668=CARTESIAN_POINT('Ctrl Pts',(-1.62554138035429,2.784323991421,57.8755188768522));
#19669=CARTESIAN_POINT('Ctrl Pts',(-1.9278482624066,2.59587914200526,57.8955744331124));
#19670=CARTESIAN_POINT('Ctrl Pts',(-2.13301448771868,2.43010860565412,57.9100503415682));
#19671=CARTESIAN_POINT('Ctrl Pts',(-2.35119945571632,2.20467075676006,57.928590028529));
#19672=CARTESIAN_POINT('Ctrl Pts',(-2.3857487111276,2.16723664813066,57.9316330520963));
#19673=CARTESIAN_POINT('Ctrl Pts',(-2.44251976480121,2.10272206840221,57.9368299593646));
#19674=CARTESIAN_POINT('Ctrl Pts',(-2.46521407632804,2.07606895539098,57.9389639148773));
#19675=CARTESIAN_POINT('Ctrl Pts',(-2.51062549333277,2.02094127610624,57.9433545662086));
#19676=CARTESIAN_POINT('Ctrl Pts',(-2.5333029291489,1.99244074097,57.94561241152));
#19677=CARTESIAN_POINT('Ctrl Pts',(-2.59008993137165,1.91853492560334,57.9514399116409));
#19678=CARTESIAN_POINT('Ctrl Pts',(-2.62349007300798,1.87260281541914,57.9550361453516));
#19679=CARTESIAN_POINT('Ctrl Pts',(-2.74910266747708,1.68989857125249,57.9692504537943));
#19680=CARTESIAN_POINT('Ctrl Pts',(-2.83196379421096,1.54702658207734,57.9801910008034));
#19681=CARTESIAN_POINT('Ctrl Pts',(-2.99616117652605,1.20611534976638,58.0056587850009));
#19682=CARTESIAN_POINT('Ctrl Pts',(-3.06946401062656,1.00503504499575,58.0202444199064));
#19683=CARTESIAN_POINT('Ctrl Pts',(-3.13145700286321,0.762527647538431,
58.0364515086102));
#19684=CARTESIAN_POINT('Ctrl Pts',(-3.13995907753847,0.726724589054719,
58.0388090374126));
#19685=CARTESIAN_POINT('Ctrl Pts',(-3.15240936265674,0.669989495848835,
58.0424812889327));
#19686=CARTESIAN_POINT('Ctrl Pts',(-3.15676623937361,0.649151510502292,
58.0438166193007));
#19687=CARTESIAN_POINT('Ctrl Pts',(-3.16491685405933,0.60814467847215,58.0464160269189));
#19688=CARTESIAN_POINT('Ctrl Pts',(-3.16872500682859,0.587980023328616,
58.0476807417008));
#19689=CARTESIAN_POINT('Ctrl Pts',(-3.17613289852994,0.54659012512587,58.0502515363195));
#19690=CARTESIAN_POINT('Ctrl Pts',(-3.17971312438338,0.525362213561324,
58.051556560361));
#19691=CARTESIAN_POINT('Ctrl Pts',(-3.19095758302043,0.454360310408386,
58.0558813662784));
#19692=CARTESIAN_POINT('Ctrl Pts',(-3.19766820145649,0.404440628147002,
58.0588563528042));
#19693=CARTESIAN_POINT('Ctrl Pts',(-3.21612230502583,0.23763649453959,58.0686390841135));
#19694=CARTESIAN_POINT('Ctrl Pts',(-3.22264674940602,0.120267106854988,
58.0752674424239));
#19695=CARTESIAN_POINT('Ctrl Pts',(-3.22274878421801,0.00279934303327976,
58.081859847365));
#19696=CARTESIAN_POINT('Ctrl Pts',(-3.22274878256121,0.00280124978110204,
58.0818597403565));
#19697=CARTESIAN_POINT('Ctrl Pts',(-3.22295790297624,-0.237785136880605,
58.0953616829093));
#19698=CARTESIAN_POINT('Ctrl Pts',(-3.19622788100395,-0.477625984509487,
58.1087087916921));
#19699=CARTESIAN_POINT('Ctrl Pts',(-3.13170233469332,-0.762362747975631,
58.1259544749398));
#19700=CARTESIAN_POINT('Ctrl Pts',(-3.11915318526195,-0.812181903703197,
58.1290223747661));
#19701=CARTESIAN_POINT('Ctrl Pts',(-3.09594587134366,-0.895819233599449,
58.134270033571));
#19702=CARTESIAN_POINT('Ctrl Pts',(-3.08591040996868,-0.929800906142302,
58.1364296532173));
#19703=CARTESIAN_POINT('Ctrl Pts',(-3.0644347111692,-0.998339668287042,
58.1408447584817));
#19704=CARTESIAN_POINT('Ctrl Pts',(-3.05296521092551,-1.03288210431023,
58.1431009286621));
#19705=CARTESIAN_POINT('Ctrl Pts',(-3.02215318343816,-1.12067707895704,
58.1489181680934));
#19706=CARTESIAN_POINT('Ctrl Pts',(-3.00198759552633,-1.17362550002979,
58.1525056297787));
#19707=CARTESIAN_POINT('Ctrl Pts',(-2.89758663148219,-1.42742439535898,
58.1700974239904));
#19708=CARTESIAN_POINT('Ctrl Pts',(-2.79454360409339,-1.61989141685892,
58.1847130849878));
#19709=CARTESIAN_POINT('Ctrl Pts',(-2.57906900765981,-1.93977628476205,
58.2107663277831));
#19710=CARTESIAN_POINT('Ctrl Pts',(-2.47447761883421,-2.0715450545229,58.2221108682565));
#19711=CARTESIAN_POINT('Ctrl Pts',(-2.33757865467796,-2.21876896399696,
58.235074729393));
#19712=CARTESIAN_POINT('Ctrl Pts',(-2.31470281759417,-2.24262362977957,
58.2371847270472));
#19713=CARTESIAN_POINT('Ctrl Pts',(-2.27703559774215,-2.2807120456572,58.2405631615659));
#19714=CARTESIAN_POINT('Ctrl Pts',(-2.2624685004369,-2.29516337260248,58.2418472562922));
#19715=CARTESIAN_POINT('Ctrl Pts',(-2.23250540864576,-2.32432582029433,
58.2444413378016));
#19716=CARTESIAN_POINT('Ctrl Pts',(-2.21709980732378,-2.33902531445437,
58.2457505230534));
#19717=CARTESIAN_POINT('Ctrl Pts',(-2.17466456586406,-2.37871957031481,
58.2492940767393));
#19718=CARTESIAN_POINT('Ctrl Pts',(-2.14734977241055,-2.4034063285044,58.2515070328352));
#19719=CARTESIAN_POINT('Ctrl Pts',(-1.97956498306949,-2.5499034445019,58.2647386416641));
#19720=CARTESIAN_POINT('Ctrl Pts',(-1.8291779708738,-2.65985118417592,58.2751102861338));
#19721=CARTESIAN_POINT('Ctrl Pts',(-1.49562741863346,-2.86196610976069,
58.2969567991984));
#19722=CARTESIAN_POINT('Ctrl Pts',(-1.31149223152743,-2.95088606072196,
58.3084073852797));
#19723=CARTESIAN_POINT('Ctrl Pts',(-1.07210638021965,-3.03962760092729,
58.3234893452765));
#19724=CARTESIAN_POINT('Ctrl Pts',(-1.02359959563135,-3.05630356440855,
58.326552552832));
#19725=CARTESIAN_POINT('Ctrl Pts',(-0.940958123590885,-3.08252653125341,
58.3317947104971));
#19726=CARTESIAN_POINT('Ctrl Pts',(-0.907025579250325,-3.09268111043141,
58.3339536286457));
#19727=CARTESIAN_POINT('Ctrl Pts',(-0.837877438667938,-3.11213836407604,
58.3383694703585));
#19728=CARTESIAN_POINT('Ctrl Pts',(-0.802657813982536,-3.12140738465124,
58.3406271149749));
#19729=CARTESIAN_POINT('Ctrl Pts',(-0.712158911981906,-3.14359178348112,
58.3464529982583));
#19730=CARTESIAN_POINT('Ctrl Pts',(-0.656683589866342,-3.15564662703973,
58.350047782547));
#19731=CARTESIAN_POINT('Ctrl Pts',(-0.564240146069718,-3.17319154966375,
58.3560799619886));
#19732=CARTESIAN_POINT('Ctrl Pts',(-0.527454640627873,-3.17951270074406,
58.3584911188382));
#19733=CARTESIAN_POINT('Ctrl Pts',(-0.490581924382687,-3.18519182122035,
58.3609184893942));
#19734=CARTESIAN_POINT('',(-3.21795389890993,-0.00035016928829556,58.3278759108383));
#19735=CARTESIAN_POINT('Ctrl Pts',(-0.491343452670647,-3.19000126486617,
58.6097459619479));
#19736=CARTESIAN_POINT('Ctrl Pts',(-1.48669079152002,-3.03231753307098,
58.54727732809));
#19737=CARTESIAN_POINT('Ctrl Pts',(-2.87365562611969,-2.04127453831248,
58.4532651482571));
#19738=CARTESIAN_POINT('Ctrl Pts',(-3.218177270761,-0.513265825290757,58.3592529684242));
#19739=CARTESIAN_POINT('Ctrl Pts',(-3.21766489697672,-0.000360507783602748,
58.3277094224493));
#19740=CARTESIAN_POINT('Ctrl Pts',(-3.22274999505125,-0.000178598057266107,
58.3306388484816));
#19741=CARTESIAN_POINT('Ctrl Pts',(-3.22275152166445,0.0273686931957166,
58.3289650202219));
#19742=CARTESIAN_POINT('Ctrl Pts',(-3.22239984723638,0.0549143201914142,
58.3272804884336));
#19743=CARTESIAN_POINT('Ctrl Pts',(-3.22079629405421,0.117571233435313,
58.3234225393163));
#19744=CARTESIAN_POINT('Ctrl Pts',(-3.21932332163406,0.152672718248279,
58.3212424896283));
#19745=CARTESIAN_POINT('Ctrl Pts',(-3.21401069872221,0.243713480325951,
58.3155367566181));
#19746=CARTESIAN_POINT('Ctrl Pts',(-3.20928464604641,0.299587168385481,
58.3119843242949));
#19747=CARTESIAN_POINT('Ctrl Pts',(-3.17931917787674,0.569727177749854,
58.294554344316));
#19748=CARTESIAN_POINT('Ctrl Pts',(-3.13406741837616,0.78118830237778,58.2800786983285));
#19749=CARTESIAN_POINT('Ctrl Pts',(-3.01625659151334,1.14757963909402,58.254080626764));
#19750=CARTESIAN_POINT('Ctrl Pts',(-2.95185826318816,1.30433323055823,58.242649922579));
#19751=CARTESIAN_POINT('Ctrl Pts',(-2.86054366726118,1.48475457999423,58.2296109801442));
#19752=CARTESIAN_POINT('Ctrl Pts',(-2.84519200336798,1.51396462788519,58.2275044157394));
#19753=CARTESIAN_POINT('Ctrl Pts',(-2.81957559134375,1.56093933224634,58.2241300538921));
#19754=CARTESIAN_POINT('Ctrl Pts',(-2.80958537046108,1.57885028879635,58.2228466634055));
#19755=CARTESIAN_POINT('Ctrl Pts',(-2.78887008968411,1.6151702717317,58.2202526387115));
#19756=CARTESIAN_POINT('Ctrl Pts',(-2.77813221753765,1.63357057532253,58.2189428275464));
#19757=CARTESIAN_POINT('Ctrl Pts',(-2.74831278439676,1.68352427672631,58.215395117694));
#19758=CARTESIAN_POINT('Ctrl Pts',(-2.72887036732328,1.71485973987912,58.2131787225866));
#19759=CARTESIAN_POINT('Ctrl Pts',(-2.60908685154661,1.90071743809104,58.2000447344578));
#19760=CARTESIAN_POINT('Ctrl Pts',(-2.4961729413212,2.04675268544039,58.1897617202013));
#19761=CARTESIAN_POINT('Ctrl Pts',(-2.23210266184536,2.33369686681867,58.1679184331134));
#19762=CARTESIAN_POINT('Ctrl Pts',(-2.07866626243933,2.47134758087012,58.1563815547593));
#19763=CARTESIAN_POINT('Ctrl Pts',(-1.87191063449352,2.62387055738965,58.1412036805653));
#19764=CARTESIAN_POINT('Ctrl Pts',(-1.82993408336617,2.65331621627637,58.1381415669522));
#19765=CARTESIAN_POINT('Ctrl Pts',(-1.75780676175894,2.70138612694307,58.1329008464759));
#19766=CARTESIAN_POINT('Ctrl Pts',(-1.72801808305598,2.72053762503069,58.1307422522321));
#19767=CARTESIAN_POINT('Ctrl Pts',(-1.66696737707833,2.75838060668851,58.1263267214002));
#19768=CARTESIAN_POINT('Ctrl Pts',(-1.6356920612514,2.77704071202683,58.1240690578455));
#19769=CARTESIAN_POINT('Ctrl Pts',(-1.55486590233354,2.82342575527607,58.1182423863547));
#19770=CARTESIAN_POINT('Ctrl Pts',(-1.50488806505103,2.85037756022782,58.1146468106689));
#19771=CARTESIAN_POINT('Ctrl Pts',(-1.26122400666847,2.97358463703967,58.0971423012683));
#19772=CARTESIAN_POINT('Ctrl Pts',(-1.05891428376394,3.05148588624235,58.0826320773377));
#19773=CARTESIAN_POINT('Ctrl Pts',(-0.687068309131056,3.15320719913749,
58.0565907867791));
#19774=CARTESIAN_POINT('Ctrl Pts',(-0.520492782642464,3.18494510044275,
58.0451525613443));
#19775=CARTESIAN_POINT('Ctrl Pts',(-0.319361332270748,3.20705724999789,
58.0321048781007));
#19776=CARTESIAN_POINT('Ctrl Pts',(-0.286484335774406,3.21016117764605,
58.0299966875096));
#19777=CARTESIAN_POINT('Ctrl Pts',(-0.233115856756237,3.21437323459194,
58.0266204376985));
#19778=CARTESIAN_POINT('Ctrl Pts',(-0.212651889309117,3.21579189966969,
58.0253367533369));
#19779=CARTESIAN_POINT('Ctrl Pts',(-0.17091425004314,3.21828518122513,58.0227427044638));
#19780=CARTESIAN_POINT('Ctrl Pts',(-0.149640894194258,3.21934447522593,
58.0214331534443));
#19781=CARTESIAN_POINT('Ctrl Pts',(-0.0915432161865209,3.22166026724364,
58.0178874059432));
#19782=CARTESIAN_POINT('Ctrl Pts',(-0.0547043013658262,3.22249635138902,
58.0156726675859));
#19783=CARTESIAN_POINT('Ctrl Pts',(0.16717426609087,3.22372581202411,58.0024925420027));
#19784=CARTESIAN_POINT('Ctrl Pts',(0.351971713844922,3.2088138540784,57.9921675813208));
#19785=CARTESIAN_POINT('Ctrl Pts',(0.736428993599204,3.14415729803788,57.9703299018682));
#19786=CARTESIAN_POINT('Ctrl Pts',(0.934656032977894,3.09102893572924,57.9588410105805));
#19787=CARTESIAN_POINT('Ctrl Pts',(1.17459898318525,3.00151144521947,57.9437130510065));
#19788=CARTESIAN_POINT('Ctrl Pts',(1.22226592145437,2.98241836605535,57.9406466737853));
#19789=CARTESIAN_POINT('Ctrl Pts',(1.30201901417135,2.94824002571026,57.9354006893267));
#19790=CARTESIAN_POINT('Ctrl Pts',(1.33435005684172,2.93374888736945,57.9332411843586));
#19791=CARTESIAN_POINT('Ctrl Pts',(1.39940641215535,2.9032920391361,57.9288255043921));
#19792=CARTESIAN_POINT('Ctrl Pts',(1.43211309689951,2.88729888938893,57.9265686312074));
#19793=CARTESIAN_POINT('Ctrl Pts',(1.51504573119677,2.84499008861874,57.9207477453517));
#19794=CARTESIAN_POINT('Ctrl Pts',(1.56485920046809,2.81789765813526,57.9171572797799));
#19795=CARTESIAN_POINT('Ctrl Pts',(1.80195888149963,2.68071848168018,57.8995974803984));
#19796=CARTESIAN_POINT('Ctrl Pts',(1.97848079589825,2.55321264091338,57.8850205591927));
#19797=CARTESIAN_POINT('Ctrl Pts',(2.26502172379285,2.29856618809587,57.8591260603297));
#19798=CARTESIAN_POINT('Ctrl Pts',(2.38051765674133,2.17873233430675,57.8479016010264));
#19799=CARTESIAN_POINT('Ctrl Pts',(2.50802674302002,2.02412684917581,57.8349615700869));
#19800=CARTESIAN_POINT('Ctrl Pts',(2.52937054621828,1.99739142401738,57.8327750653107));
#19801=CARTESIAN_POINT('Ctrl Pts',(2.56297379075501,1.95389703319851,57.8293058696407));
#19802=CARTESIAN_POINT('Ctrl Pts',(2.57550354005013,1.93735124506997,57.828006037752));
#19803=CARTESIAN_POINT('Ctrl Pts',(2.60039596799797,1.903811937988,57.8254128785718));
#19804=CARTESIAN_POINT('Ctrl Pts',(2.61275399041164,1.88681629418159,57.8241198574134));
#19805=CARTESIAN_POINT('Ctrl Pts',(2.64551751752937,1.84081830226653,57.8206729010836));
#19806=CARTESIAN_POINT('Ctrl Pts',(2.6656126140456,1.81159724589741,57.8185384448015));
#19807=CARTESIAN_POINT('Ctrl Pts',(2.79692150756155,1.61373875257659,57.8044092364315));
#19808=CARTESIAN_POINT('Ctrl Pts',(2.89256221463683,1.43527892424226,57.7931948972296));
#19809=CARTESIAN_POINT('Ctrl Pts',(3.02044469736014,1.13110286277834,57.7747045425397));
#19810=CARTESIAN_POINT('Ctrl Pts',(3.06295355279475,1.0103429281048,57.7675143048786));
#19811=CARTESIAN_POINT('Ctrl Pts',(3.11494092598975,0.828836170490921,57.7566352669263));
#19812=CARTESIAN_POINT('Ctrl Pts',(3.13004608136707,0.769829393781804,57.7530887388334));
#19813=CARTESIAN_POINT('Ctrl Pts',(3.15493079553585,0.659721306799046,57.7464246407004));
#19814=CARTESIAN_POINT('Ctrl Pts',(3.16516232242812,0.608742597816576,57.7433212621948));
#19815=CARTESIAN_POINT('Ctrl Pts',(3.18030452796812,0.52253594410534,57.7380313647149));
#19816=CARTESIAN_POINT('Ctrl Pts',(3.18587345172688,0.487432967305735,57.7358657832285));
#19817=CARTESIAN_POINT('Ctrl Pts',(3.19594792353134,0.416351683497813,57.7314540202528));
#19818=CARTESIAN_POINT('Ctrl Pts',(3.20042909687102,0.380375183808316,57.7292074151364));
#19819=CARTESIAN_POINT('Ctrl Pts',(3.21027376138446,0.288762168159615,57.7234487816755));
#19820=CARTESIAN_POINT('Ctrl Pts',(3.2147983655815,0.233049490379661,57.7199114154083));
#19821=CARTESIAN_POINT('Ctrl Pts',(3.23029217082074,-0.0482316991034988,
57.7018649371716));
#19822=CARTESIAN_POINT('Ctrl Pts',(3.21897644745742,-0.274362845236531,
57.6866888837325));
#19823=CARTESIAN_POINT('Ctrl Pts',(3.15982160339512,-0.653033594529865,
57.6608009758255));
#19824=CARTESIAN_POINT('Ctrl Pts',(3.12413385428399,-0.806672911467985,
57.6501793253463));
#19825=CARTESIAN_POINT('Ctrl Pts',(3.06691634995948,-0.990644225063457,
57.6377262915629));
#19826=CARTESIAN_POINT('Ctrl Pts',(3.05593417190987,-1.02402072591774,57.635478592567));
#19827=CARTESIAN_POINT('Ctrl Pts',(3.03753715548488,-1.07699779823064,57.6319367022852));
#19828=CARTESIAN_POINT('Ctrl Pts',(3.0304734944639,-1.0967163190735,57.6306241568628));
#19829=CARTESIAN_POINT('Ctrl Pts',(3.01600744814588,-1.13589168003481,57.6280300187548));
#19830=CARTESIAN_POINT('Ctrl Pts',(3.00860780279707,-1.15534842209092,57.6267483720005));
#19831=CARTESIAN_POINT('Ctrl Pts',(2.98844055814241,-1.20686848666052,57.6233692421735));
#19832=CARTESIAN_POINT('Ctrl Pts',(2.97534523209174,-1.23880163022747,57.6212899197271));
#19833=CARTESIAN_POINT('Ctrl Pts',(2.87884433953011,-1.46375717624347,57.6067083562));
#19834=CARTESIAN_POINT('Ctrl Pts',(2.77722700054671,-1.64844209560315,57.5950631146779));
#19835=CARTESIAN_POINT('Ctrl Pts',(2.5882554094643,-1.92416597647126,57.5763245108605));
#19836=CARTESIAN_POINT('Ctrl Pts',(2.51234635132951,-2.02227448472634,57.5693469378452));
#19837=CARTESIAN_POINT('Ctrl Pts',(2.39168404625158,-2.16091361971217,57.558747191949));
#19838=CARTESIAN_POINT('Ctrl Pts',(2.35113988230167,-2.2049582593451,57.5552585816594));
#19839=CARTESIAN_POINT('Ctrl Pts',(2.27359208394664,-2.28462937133571,57.5486909517378));
#19840=CARTESIAN_POINT('Ctrl Pts',(2.23691769887164,-2.32054974158849,57.5456253619101));
#19841=CARTESIAN_POINT('Ctrl Pts',(2.17350962106284,-2.37975385878226,57.5403803933288));
#19842=CARTESIAN_POINT('Ctrl Pts',(2.14722061240321,-2.40350077778701,57.5382211014456));
#19843=CARTESIAN_POINT('Ctrl Pts',(2.09313103548318,-2.4507642665179,57.533805583614));
#19844=CARTESIAN_POINT('Ctrl Pts',(2.06531276550229,-2.47425262058322,57.5315486548871));
#19845=CARTESIAN_POINT('Ctrl Pts',(1.99316131752587,-2.53310901936143,57.5257270458555));
#19846=CARTESIAN_POINT('Ctrl Pts',(1.94828313717074,-2.5677861117591,57.5221358955008));
#19847=CARTESIAN_POINT('Ctrl Pts',(1.72726646840164,-2.72943382840837,57.5045824560281));
#19848=CARTESIAN_POINT('Ctrl Pts',(1.5395372650818,-2.83955228568609,57.4900132958563));
#19849=CARTESIAN_POINT('Ctrl Pts',(1.18908557348437,-3.000092735002,57.4639745444006));
#19850=CARTESIAN_POINT('Ctrl Pts',(1.03069679576482,-3.0581292438205,57.4525979376705));
#19851=CARTESIAN_POINT('Ctrl Pts',(0.836608868096332,-3.11244259429169,
57.4396005828479));
#19852=CARTESIAN_POINT('Ctrl Pts',(0.804594551051987,-3.12087185037611,
57.4374869748035));
#19853=CARTESIAN_POINT('Ctrl Pts',(0.75252401882504,-3.13372727041929,57.4341042560607));
#19854=CARTESIAN_POINT('Ctrl Pts',(0.73254598776435,-3.13845749587943,57.4328194178716));
#19855=CARTESIAN_POINT('Ctrl Pts',(0.691772070086702,-3.14770101929637,
57.4302254545844));
#19856=CARTESIAN_POINT('Ctrl Pts',(0.67097415693125,-3.15219987361767,57.4289171063298));
#19857=CARTESIAN_POINT('Ctrl Pts',(0.614144107171793,-3.16390497480123,
57.425378508203));
#19858=CARTESIAN_POINT('Ctrl Pts',(0.578029820853918,-3.17070172920799,
57.4231695713823));
#19859=CARTESIAN_POINT('Ctrl Pts',(0.35667228352335,-3.2084534693292,57.4098291812621));
#19860=CARTESIAN_POINT('Ctrl Pts',(0.169112102368853,-3.22378745357848,
57.3993589396824));
#19861=CARTESIAN_POINT('Ctrl Pts',(-0.176784835446328,-3.22177683668667,
57.3799828441799));
#19862=CARTESIAN_POINT('Ctrl Pts',(-0.334490470502797,-3.20923297810243,
57.3711216961903));
#19863=CARTESIAN_POINT('Ctrl Pts',(-0.490582240097166,-3.18519177259412,
57.3619600447814));
#19864=CARTESIAN_POINT('Origin',(-9.35406549764863E-15,0.,41.4527091182931));
#19865=CARTESIAN_POINT('',(-0.490582094113513,-3.18519179507847,55.8661429281184));
#19866=CARTESIAN_POINT('',(-0.49058220660185,-3.18519177775306,56.1109990110886));
#19867=CARTESIAN_POINT('',(-0.490582094296226,-3.18519179505033,41.4527091182931));
#19868=CARTESIAN_POINT('Ctrl Pts',(-0.490582094113513,-3.18519179507847,
55.8661429281184));
#19869=CARTESIAN_POINT('Ctrl Pts',(-0.47670444968123,-3.18732922488018,
55.8670384748254));
#19870=CARTESIAN_POINT('Ctrl Pts',(-0.462812504433887,-3.18937600998039,
55.8679297983106));
#19871=CARTESIAN_POINT('Ctrl Pts',(-0.428211029566095,-3.1942432094582,
55.8701363448911));
#19872=CARTESIAN_POINT('Ctrl Pts',(-0.407486404536188,-3.19695312033762,
55.8714459329507));
#19873=CARTESIAN_POINT('Ctrl Pts',(-0.366029888983269,-3.20196419399069,
55.874039599157));
#19874=CARTESIAN_POINT('Ctrl Pts',(-0.345299098145667,-3.2042660885778,
55.8753236541104));
#19875=CARTESIAN_POINT('Ctrl Pts',(-0.2900088855317,-3.20986253539667,55.8787173338094));
#19876=CARTESIAN_POINT('Ctrl Pts',(-0.255415183741497,-3.21280032880294,
55.8808085154941));
#19877=CARTESIAN_POINT('Ctrl Pts',(-0.0127784440216769,-3.22946165812842,
55.8952927104781));
#19878=CARTESIAN_POINT('Ctrl Pts',(0.19614304644915,-3.22352829094271,55.9068455410471));
#19879=CARTESIAN_POINT('Ctrl Pts',(0.588178394484766,-3.17411124605778,
55.928994475777));
#19880=CARTESIAN_POINT('Ctrl Pts',(0.770914411840194,-3.13474354180852,
55.9395246334886));
#19881=CARTESIAN_POINT('Ctrl Pts',(0.997698312050101,-3.06484750303191,
55.9535510446941));
#19882=CARTESIAN_POINT('Ctrl Pts',(1.04582596875649,-3.04876036475308,55.9565828701577));
#19883=CARTESIAN_POINT('Ctrl Pts',(1.12677929858761,-3.01955852641632,55.9617877941285));
#19884=CARTESIAN_POINT('Ctrl Pts',(1.15980628279295,-3.00702752160471,55.9639415577062));
#19885=CARTESIAN_POINT('Ctrl Pts',(1.2265778419221,-2.98042958286822,55.9683611056681));
#19886=CARTESIAN_POINT('Ctrl Pts',(1.26030227251802,-2.96632629839689,55.9706278507027));
#19887=CARTESIAN_POINT('Ctrl Pts',(1.34642832032429,-2.92857523828918,55.9765093250905));
#19888=CARTESIAN_POINT('Ctrl Pts',(1.39844840145215,-2.90409427310019,55.980151615767));
#19889=CARTESIAN_POINT('Ctrl Pts',(1.63118595926614,-2.78686309019022,55.9968679769992));
#19890=CARTESIAN_POINT('Ctrl Pts',(1.80351938886978,-2.67855735466658,56.0104606601649));
#19891=CARTESIAN_POINT('Ctrl Pts',(2.06293104411941,-2.47908302951427,56.0325605787091));
#19892=CARTESIAN_POINT('Ctrl Pts',(2.15691535032348,-2.39776051821599,56.0409633809983));
#19893=CARTESIAN_POINT('Ctrl Pts',(2.29619436507772,-2.26241300559162,56.0538313522796));
#19894=CARTESIAN_POINT('Ctrl Pts',(2.34481369435936,-2.21198357967963,56.0584112750476));
#19895=CARTESIAN_POINT('Ctrl Pts',(2.40976248496615,-2.1400664063542,56.0646082076616));
#19896=CARTESIAN_POINT('Ctrl Pts',(2.42752112403396,-2.11990112066129,56.0663112408296));
#19897=CARTESIAN_POINT('Ctrl Pts',(2.45775939543882,-2.08468662931633,56.0692226271702));
#19898=CARTESIAN_POINT('Ctrl Pts',(2.470357560228,-2.06974229793869,56.0704390228371));
#19899=CARTESIAN_POINT('Ctrl Pts',(2.49809864744352,-2.03622076502335,56.0731247757435));
#19900=CARTESIAN_POINT('Ctrl Pts',(2.51317143908598,-2.01758797934894,56.0745894140769));
#19901=CARTESIAN_POINT('Ctrl Pts',(2.55954443531488,-1.95893615018212,56.079118649174));
#19902=CARTESIAN_POINT('Ctrl Pts',(2.59010851189404,-1.91834226992867,56.0821376347155));
#19903=CARTESIAN_POINT('Ctrl Pts',(2.73331671616837,-1.71847295094721,56.0965417879778));
#19904=CARTESIAN_POINT('Ctrl Pts',(2.83231019682779,-1.54990383381216,56.1073319787516));
#19905=CARTESIAN_POINT('Ctrl Pts',(2.98423636713134,-1.22739564660362,56.1273378692314));
#19906=CARTESIAN_POINT('Ctrl Pts',(3.04194603784082,-1.07644050393369,56.1364734983749));
#19907=CARTESIAN_POINT('Ctrl Pts',(3.10421208437822,-0.86784567607846,56.1492746312506));
#19908=CARTESIAN_POINT('Ctrl Pts',(3.11890163276317,-0.813474539407798,
56.1526252391296));
#19909=CARTESIAN_POINT('Ctrl Pts',(3.14071244108851,-0.723438265365074,
56.1582118220488));
#19910=CARTESIAN_POINT('Ctrl Pts',(3.14866821898781,-0.687986804370231,
56.1604210409529));
#19911=CARTESIAN_POINT('Ctrl Pts',(3.16312164009831,-0.618068561490217,
56.1648003310201));
#19912=CARTESIAN_POINT('Ctrl Pts',(3.16965935520165,-0.583615177516491,
56.166968791248));
#19913=CARTESIAN_POINT('Ctrl Pts',(3.18437365578035,-0.498511604972874,
56.1723537130019));
#19914=CARTESIAN_POINT('Ctrl Pts',(3.19190520724935,-0.447761173836143,
56.1755898173135));
#19915=CARTESIAN_POINT('Ctrl Pts',(3.2302866202595,-0.138448366816227,56.1954743207642));
#19916=CARTESIAN_POINT('Ctrl Pts',(3.23091024889173,0.122854387471132,56.2130669271184));
#19917=CARTESIAN_POINT('Ctrl Pts',(3.18893482938931,0.475113758040776,56.2369964425577));
#19918=CARTESIAN_POINT('Ctrl Pts',(3.17364099128598,0.568368749314567,56.2433387032443));
#19919=CARTESIAN_POINT('Ctrl Pts',(3.14574154603605,0.70154007975339,56.2523029659562));
#19920=CARTESIAN_POINT('Ctrl Pts',(3.13642287670455,0.74209177557174,56.2550198158851));
#19921=CARTESIAN_POINT('Ctrl Pts',(3.11821209969496,0.814853604234161,56.2598585442939));
#19922=CARTESIAN_POINT('Ctrl Pts',(3.10959943034297,0.847127310274433,56.2619917936124));
#19923=CARTESIAN_POINT('Ctrl Pts',(3.09486913226624,0.899069790828841,56.2653977364233));
#19924=CARTESIAN_POINT('Ctrl Pts',(3.0890621621364,0.918823412828881,56.266686536685));
#19925=CARTESIAN_POINT('Ctrl Pts',(3.07689197904674,0.958802788549101,56.269279881261));
#19926=CARTESIAN_POINT('Ctrl Pts',(3.0705177399317,0.979023955243096,56.2705837807056));
#19927=CARTESIAN_POINT('Ctrl Pts',(3.05266689599205,1.03376275462796,56.2740959343032));
#19928=CARTESIAN_POINT('Ctrl Pts',(3.04080440289872,1.06815234990088,56.2762834098996));
#19929=CARTESIAN_POINT('Ctrl Pts',(2.96226897875499,1.28390672583224,56.2899297652349));
#19930=CARTESIAN_POINT('Ctrl Pts',(2.87997276202006,1.45918736029554,56.3006842756705));
#19931=CARTESIAN_POINT('Ctrl Pts',(2.71569104769115,1.74030178001293,56.3189247676308));
#19932=CARTESIAN_POINT('Ctrl Pts',(2.64195380804453,1.8503258137384,56.3263511990141));
#19933=CARTESIAN_POINT('Ctrl Pts',(2.52402775760024,2.00480649901951,56.3375389904976));
#19934=CARTESIAN_POINT('Ctrl Pts',(2.48497554605672,2.05301269454797,56.3411480963542));
#19935=CARTESIAN_POINT('Ctrl Pts',(2.41021738422415,2.14003433369257,56.3479162099498));
#19936=CARTESIAN_POINT('Ctrl Pts',(2.3749027870915,2.1791583406538,56.3510601803951));
#19937=CARTESIAN_POINT('Ctrl Pts',(2.31410666266537,2.24327884102337,56.3563984183446));
#19938=CARTESIAN_POINT('Ctrl Pts',(2.28913990124072,2.26875030806929,56.3585708221852));
#19939=CARTESIAN_POINT('Ctrl Pts',(2.23806354121418,2.31915764973697,56.3629792488577));
#19940=CARTESIAN_POINT('Ctrl Pts',(2.21194744237422,2.34407955571488,56.3652154050871));
#19941=CARTESIAN_POINT('Ctrl Pts',(2.1449502155314,2.40589653163552,56.3709104276494));
#19942=CARTESIAN_POINT('Ctrl Pts',(2.10353317742379,2.44219105097937,56.3743935063971));
#19943=CARTESIAN_POINT('Ctrl Pts',(1.88203893702601,2.62647493840984,56.3928384337499));
#19944=CARTESIAN_POINT('Ctrl Pts',(1.68725166408408,2.75564704606478,56.4085202932165));
#19945=CARTESIAN_POINT('Ctrl Pts',(1.38522339005281,2.9118251449608,56.4314837317641));
#19946=CARTESIAN_POINT('Ctrl Pts',(1.28777264186515,2.95621602239485,56.4386960798101));
#19947=CARTESIAN_POINT('Ctrl Pts',(1.14673207983078,3.01216233257248,56.4487196328347));
#19948=CARTESIAN_POINT('Ctrl Pts',(1.10483354061134,3.02778129904125,56.4516468943765));
#19949=CARTESIAN_POINT('Ctrl Pts',(1.02935303677655,3.05414336653264,56.4568152507961));
#19950=CARTESIAN_POINT('Ctrl Pts',(0.995894395060094,3.06521678928511,56.4590699900929));
#19951=CARTESIAN_POINT('Ctrl Pts',(0.942249672518553,3.08199978786892,56.4626202237089));
#19952=CARTESIAN_POINT('Ctrl Pts',(0.922178750631355,3.08806469275649,56.4639342139344));
#19953=CARTESIAN_POINT('Ctrl Pts',(0.882087236783464,3.0997535436629,56.4665284938078));
#19954=CARTESIAN_POINT('Ctrl Pts',(0.862068609168573,3.10538044172264,56.4678088767183));
#19955=CARTESIAN_POINT('Ctrl Pts',(0.808785512829795,3.11980244888435,56.4711805404664));
#19956=CARTESIAN_POINT('Ctrl Pts',(0.775431349086768,3.12825954205491,56.4732538042292));
#19957=CARTESIAN_POINT('Ctrl Pts',(0.536450082281223,3.18479688517124,56.4878848007231));
#19958=CARTESIAN_POINT('Ctrl Pts',(0.326647292156141,3.21310333627802,56.4995769360888));
#19959=CARTESIAN_POINT('Ctrl Pts',(-0.00787833689097536,3.22510664609324,
56.518343107162));
#19960=CARTESIAN_POINT('Ctrl Pts',(-0.131466998268363,3.22243524287872,
56.5252977480078));
#19961=CARTESIAN_POINT('Ctrl Pts',(-0.314145882711706,3.20795868050048,
56.5358672764335));
#19962=CARTESIAN_POINT('Ctrl Pts',(-0.373554652365925,3.20158443251951,
56.5393495261672));
#19963=CARTESIAN_POINT('Ctrl Pts',(-0.483542419707747,3.18668033611588,
56.5459065319408));
#19964=CARTESIAN_POINT('Ctrl Pts',(-0.534161461463274,3.17858709762858,
56.5489679404079));
#19965=CARTESIAN_POINT('Ctrl Pts',(-0.619388244642953,3.16286733055723,
56.5542078987026));
#19966=CARTESIAN_POINT('Ctrl Pts',(-0.654103134020785,3.15587079653844,
56.5563664546534));
#19967=CARTESIAN_POINT('Ctrl Pts',(-0.724276330986334,3.14052033868824,
56.5607822979248));
#19968=CARTESIAN_POINT('Ctrl Pts',(-0.759722279522704,3.13213442993292,
56.5630403187705));
#19969=CARTESIAN_POINT('Ctrl Pts',(-0.850059794046157,3.1091384491417,56.5688688078742));
#19970=CARTESIAN_POINT('Ctrl Pts',(-0.904719212054918,3.09367516885826,
56.5724658721226));
#19971=CARTESIAN_POINT('Ctrl Pts',(-1.16513282242976,3.01251206080619,56.5899531173097));
#19972=CARTESIAN_POINT('Ctrl Pts',(-1.36431596881225,2.92769182767227,56.6044425727736));
#19973=CARTESIAN_POINT('Ctrl Pts',(-1.70186246377706,2.74198091464352,56.6304669194268));
#19974=CARTESIAN_POINT('Ctrl Pts',(-1.84358136506399,2.64877564821555,56.6419090284364));
#19975=CARTESIAN_POINT('Ctrl Pts',(-2.00347763309022,2.52453790421698,56.654967539123));
#19976=CARTESIAN_POINT('Ctrl Pts',(-2.02931455270895,2.50381646684228,56.6570820993504));
#19977=CARTESIAN_POINT('Ctrl Pts',(-2.07064536373954,2.46960864950359,56.660465917439));
#19978=CARTESIAN_POINT('Ctrl Pts',(-2.08633734176591,2.45636635574517,56.6617509213592));
#19979=CARTESIAN_POINT('Ctrl Pts',(-2.11802790831272,2.42910021773898,56.6643447469881));
#19980=CARTESIAN_POINT('Ctrl Pts',(-2.13401619253562,2.41506625930702,56.6656527991246));
#19981=CARTESIAN_POINT('Ctrl Pts',(-2.17722194371027,2.37637763832796,56.6691898050035));
#19982=CARTESIAN_POINT('Ctrl Pts',(-2.20415963682996,2.35141374975379,56.671397476776));
#19983=CARTESIAN_POINT('Ctrl Pts',(-2.39560230770309,2.16781709975211,56.687156021637));
#19984=CARTESIAN_POINT('Ctrl Pts',(-2.54326602324136,1.9925271211549,56.6997218025243));
#19985=CARTESIAN_POINT('Ctrl Pts',(-2.73309519742439,1.71130532520461,56.7187858117523));
#19986=CARTESIAN_POINT('Ctrl Pts',(-2.79026517818625,1.61641373081543,56.725051730982));
#19987=CARTESIAN_POINT('Ctrl Pts',(-2.87976139486696,1.44891845261527,56.7360404852419));
#19988=CARTESIAN_POINT('Ctrl Pts',(-2.91449605258379,1.37771612195877,56.7406903348094));
#19989=CARTESIAN_POINT('Ctrl Pts',(-2.96300379955642,1.2682160977233,56.7478551755739));
#19990=CARTESIAN_POINT('Ctrl Pts',(-2.9787338318114,1.23081603875404,56.7503045430426));
#19991=CARTESIAN_POINT('Ctrl Pts',(-3.00644600427892,1.16128179931595,56.7548676906535));
#19992=CARTESIAN_POINT('Ctrl Pts',(-3.01862944661091,1.12923386242605,56.7569743705802));
#19993=CARTESIAN_POINT('Ctrl Pts',(-3.04469977284466,1.05721838103859,56.7617190010019));
#19994=CARTESIAN_POINT('Ctrl Pts',(-3.05831531635106,1.01716005002643,56.7643654460466));
#19995=CARTESIAN_POINT('Ctrl Pts',(-3.09835471442656,0.891278983986175,
56.7727087230335));
#19996=CARTESIAN_POINT('Ctrl Pts',(-3.12198127854482,0.804618311694492,
56.7784925252685));
#19997=CARTESIAN_POINT('Ctrl Pts',(-3.19580997906034,0.481135234170011,
56.8002219860887));
#19998=CARTESIAN_POINT('Ctrl Pts',(-3.22290709110659,0.239875915335549,
56.8167722868544));
#19999=CARTESIAN_POINT('Ctrl Pts',(-3.22268781229327,-0.0964266138825664,
56.8392710364056));
#20000=CARTESIAN_POINT('Ctrl Pts',(-3.21848516002261,-0.19071206053494,
56.8455055763825));
#20001=CARTESIAN_POINT('Ctrl Pts',(-3.20750067365725,-0.314575060533712,
56.8534938739027));
#20002=CARTESIAN_POINT('Ctrl Pts',(-3.20443242981268,-0.344428503107231,
56.85540353909));
#20003=CARTESIAN_POINT('Ctrl Pts',(-3.19865291071894,-0.393862389159491,
56.8585349646516));
#20004=CARTESIAN_POINT('Ctrl Pts',(-3.19617775182092,-0.413468119291994,
56.8597687931013));
#20005=CARTESIAN_POINT('Ctrl Pts',(-3.19053934935145,-0.455048348932169,
56.862366875966));
#20006=CARTESIAN_POINT('Ctrl Pts',(-3.18732915729476,-0.477014935039213,
56.8637286352716));
#20007=CARTESIAN_POINT('Ctrl Pts',(-3.1774972106612,-0.539754739861388,
56.8675915824539));
#20008=CARTESIAN_POINT('Ctrl Pts',(-3.17031801139851,-0.580437559142972,
56.8700644258148));
#20009=CARTESIAN_POINT('Ctrl Pts',(-3.15165928328733,-0.675458710877265,
56.875788317086));
#20010=CARTESIAN_POINT('Ctrl Pts',(-3.13955339492991,-0.729661426069452,
56.8790133507642));
#20011=CARTESIAN_POINT('Ctrl Pts',(-3.08657282978102,-0.941039040599342,
56.891525386038));
#20012=CARTESIAN_POINT('Ctrl Pts',(-3.03524329246229,-1.09534897354148,
56.9005274824662));
#20013=CARTESIAN_POINT('Ctrl Pts',(-2.90797420169957,-1.39917649074966,
56.919029781238));
#20014=CARTESIAN_POINT('Ctrl Pts',(-2.83158073567251,-1.547950601993,56.9285127391271));
#20015=CARTESIAN_POINT('Ctrl Pts',(-2.71776850439516,-1.73273066165305,
56.9413487171698));
#20016=CARTESIAN_POINT('Ctrl Pts',(-2.69054019086809,-1.7747152635268,56.9443402225764));
#20017=CARTESIAN_POINT('Ctrl Pts',(-2.64270507366503,-1.84484210203831,
56.9494764573911));
#20018=CARTESIAN_POINT('Ctrl Pts',(-2.62259831550368,-1.87331535421201,
56.9516024003649));
#20019=CARTESIAN_POINT('Ctrl Pts',(-2.58040604001634,-1.93105307955987,
56.9560005114345));
#20020=CARTESIAN_POINT('Ctrl Pts',(-2.55827513279346,-1.96027791315073,
56.9582742283772));
#20021=CARTESIAN_POINT('Ctrl Pts',(-2.4998319705294,-2.03477901321709,56.9641979775069));
#20022=CARTESIAN_POINT('Ctrl Pts',(-2.46278784603072,-2.07946167326016,
56.9678763492484));
#20023=CARTESIAN_POINT('Ctrl Pts',(-2.30947364543152,-2.25454352882659,
56.9828113549079));
#20024=CARTESIAN_POINT('Ctrl Pts',(-2.18390711485839,-2.37637756037815,
56.9944328268553));
#20025=CARTESIAN_POINT('Ctrl Pts',(-1.89154285511145,-2.61722308799599,
57.019965039001));
#20026=CARTESIAN_POINT('Ctrl Pts',(-1.72199565712268,-2.7317635137031,57.0338791711534));
#20027=CARTESIAN_POINT('Ctrl Pts',(-1.51182289155625,-2.84635721979762,
57.0493533901504));
#20028=CARTESIAN_POINT('Ctrl Pts',(-1.48062646122085,-2.86270910045825,
57.0516067231796));
#20029=CARTESIAN_POINT('Ctrl Pts',(-1.43044397967395,-2.88797281387489,
57.0551552852409));
#20030=CARTESIAN_POINT('Ctrl Pts',(-1.41162900444431,-2.89721600220376,
57.0564689818545));
#20031=CARTESIAN_POINT('Ctrl Pts',(-1.37396939336562,-2.91526297354355,
57.0590632169092));
#20032=CARTESIAN_POINT('Ctrl Pts',(-1.3551270998134,-2.92406920103678,57.0603438408823));
#20033=CARTESIAN_POINT('Ctrl Pts',(-1.30487266002862,-2.94696624716074,
57.0637169508428));
#20034=CARTESIAN_POINT('Ctrl Pts',(-1.27331686516579,-2.96073759320142,
57.0657913918869));
#20035=CARTESIAN_POINT('Ctrl Pts',(-1.20156321774696,-2.99069231707555,
57.0704237587892));
#20036=CARTESIAN_POINT('Ctrl Pts',(-1.16124706578631,-3.00657617311166,
57.0729676164234));
#20037=CARTESIAN_POINT('Ctrl Pts',(-1.02565995311446,-3.05686066842746,
57.0813658825689));
#20038=CARTESIAN_POINT('Ctrl Pts',(-0.92908579829348,-3.08758438891062,
57.0870938219642));
#20039=CARTESIAN_POINT('Ctrl Pts',(-0.71895002008604,-3.14368117062449,
57.0993140318433));
#20040=CARTESIAN_POINT('Ctrl Pts',(-0.605236661070453,-3.16753275047228,
57.1057815379584));
#20041=CARTESIAN_POINT('Ctrl Pts',(-0.490581808115708,-3.18519183912774,
57.1123311812828));
#20042=CARTESIAN_POINT('Ctrl Pts',(-0.490582240097165,-3.18519177259412,
57.3619600447814));
#20043=CARTESIAN_POINT('Ctrl Pts',(-0.528616395488554,-3.17933376388247,
57.3597276678007));
#20044=CARTESIAN_POINT('Ctrl Pts',(-0.566554773874653,-3.17279310424186,
57.3574782319896));
#20045=CARTESIAN_POINT('Ctrl Pts',(-0.657353474889526,-3.1554575811956,
57.3520309897278));
#20046=CARTESIAN_POINT('Ctrl Pts',(-0.710063144317063,-3.14401589865181,
57.3488165503753));
#20047=CARTESIAN_POINT('Ctrl Pts',(-0.797329981891067,-3.12276649170889,
57.3433938679773));
#20048=CARTESIAN_POINT('Ctrl Pts',(-0.832055764269073,-3.11369374011445,
57.341209120607));
#20049=CARTESIAN_POINT('Ctrl Pts',(-0.90116188029666,-3.09439991633808,
57.3368038840464));
#20050=CARTESIAN_POINT('Ctrl Pts',(-0.935537490481778,-3.08418109333674,
57.3345837387818));
#20051=CARTESIAN_POINT('Ctrl Pts',(-1.02101466384346,-3.05721083487565,
57.3289877996397));
#20052=CARTESIAN_POINT('Ctrl Pts',(-1.07187935136914,-3.03975050596263,
57.3255895231349));
#20053=CARTESIAN_POINT('Ctrl Pts',(-1.35017156914257,-2.93636773752018,
57.3066066019719));
#20054=CARTESIAN_POINT('Ctrl Pts',(-1.56771828938307,-2.82620618732505,
57.2902240416626));
#20055=CARTESIAN_POINT('Ctrl Pts',(-1.85613349627362,-2.63653614801889,
57.2669189161702));
#20056=CARTESIAN_POINT('Ctrl Pts',(-1.93877758632558,-2.57637299759377,
57.2600428463621));
#20057=CARTESIAN_POINT('Ctrl Pts',(-2.05237161865966,-2.48511251269254,
57.2504263656573));
#20058=CARTESIAN_POINT('Ctrl Pts',(-2.08576134547418,-2.45715555370437,
57.2475781827734));
#20059=CARTESIAN_POINT('Ctrl Pts',(-2.14461419195035,-2.40581410636247,
57.2425333042742));
#20060=CARTESIAN_POINT('Ctrl Pts',(-2.17028691670122,-2.38268052148736,
57.2403238390731));
#20061=CARTESIAN_POINT('Ctrl Pts',(-2.21082779571737,-2.34495025061651,
57.2368274009425));
#20062=CARTESIAN_POINT('Ctrl Pts',(-2.22593449617254,-2.33061513303711,
57.2355228347075));
#20063=CARTESIAN_POINT('Ctrl Pts',(-2.25594755574726,-2.30157695437281,
57.2329295306156));
#20064=CARTESIAN_POINT('Ctrl Pts',(-2.27085170100453,-2.28687307463408,
57.2316409584689));
#20065=CARTESIAN_POINT('Ctrl Pts',(-2.31034942376289,-2.24713914267313,
57.2282205017733));
#20066=CARTESIAN_POINT('Ctrl Pts',(-2.33467994111702,-2.22185026147899,
57.2261075784178));
#20067=CARTESIAN_POINT('Ctrl Pts',(-2.49845997688234,-2.04595726480858,
57.2118009763286));
#20068=CARTESIAN_POINT('Ctrl Pts',(-2.62367386487158,-1.88271048827538,
57.200417263054));
#20069=CARTESIAN_POINT('Ctrl Pts',(-2.8297366118413,-1.55316860075325,57.1786346129206));
#20070=CARTESIAN_POINT('Ctrl Pts',(-2.91349988128619,-1.38969468509997,
57.1682972974079));
#20071=CARTESIAN_POINT('Ctrl Pts',(-3.00310887193664,-1.17059930024392,
57.1543411321359));
#20072=CARTESIAN_POINT('Ctrl Pts',(-3.02208040672273,-1.12071189441505,
57.1511589541182));
#20073=CARTESIAN_POINT('Ctrl Pts',(-3.05168990622288,-1.03662288124369,
57.1457749557538));
#20074=CARTESIAN_POINT('Ctrl Pts',(-3.06301248925283,-1.00267273520027,
57.1435958792124));
#20075=CARTESIAN_POINT('Ctrl Pts',(-3.08457605985087,-0.93423854665951,
57.1391894118032));
#20076=CARTESIAN_POINT('Ctrl Pts',(-3.09480971998556,-0.899757613207197,
57.1369621494825));
#20077=CARTESIAN_POINT('Ctrl Pts',(-3.11905262462062,-0.81276185640739,
57.1313221504434));
#20078=CARTESIAN_POINT('Ctrl Pts',(-3.13231406278992,-0.760052073671085,
57.1278861668829));
#20079=CARTESIAN_POINT('Ctrl Pts',(-3.1966232932322,-0.474064111955712,
57.109133148888));
#20080=CARTESIAN_POINT('Ctrl Pts',(-3.22294807162268,-0.236025879415922,
57.0930523698287));
#20081=CARTESIAN_POINT('Ctrl Pts',(-3.22263065423201,0.144369481261549,
57.0673664502987));
#20082=CARTESIAN_POINT('Ctrl Pts',(-3.21316958118118,0.285899179383458,
57.0578333077411));
#20083=CARTESIAN_POINT('Ctrl Pts',(-3.18933104872129,0.464506651136535,
57.0461463786206));
#20084=CARTESIAN_POINT('Ctrl Pts',(-3.1835558176421,0.502565040915061,57.0436766772242));
#20085=CARTESIAN_POINT('Ctrl Pts',(-3.17347134504083,0.561840943787612,
57.0398716355887));
#20086=CARTESIAN_POINT('Ctrl Pts',(-3.16962801691703,0.583132849548935,
57.0385132907892));
#20087=CARTESIAN_POINT('Ctrl Pts',(-3.1617663835976,0.624309498041845,57.0359048417039));
#20088=CARTESIAN_POINT('Ctrl Pts',(-3.15777427376064,0.644197696971805,
57.0346535468147));
#20089=CARTESIAN_POINT('Ctrl Pts',(-3.14703435003528,0.695202148264648,
57.0314637198799));
#20090=CARTESIAN_POINT('Ctrl Pts',(-3.14001251429949,0.726259465015385,
57.0295397682748));
#20091=CARTESIAN_POINT('Ctrl Pts',(-3.10148683257822,0.885638071081805,
57.0197377274504));
#20092=CARTESIAN_POINT('Ctrl Pts',(-3.06257026290644,1.01205034349357,57.0121993307134));
#20093=CARTESIAN_POINT('Ctrl Pts',(-2.92588144408565,1.37503644571576,56.9903393362015));
#20094=CARTESIAN_POINT('Ctrl Pts',(-2.80761224600205,1.60275220779664,56.9762712783642));
#20095=CARTESIAN_POINT('Ctrl Pts',(-2.63168424484929,1.86107113983018,56.9579008786663));
#20096=CARTESIAN_POINT('Ctrl Pts',(-2.59845629744995,1.90718956757727,56.9545205015128));
#20097=CARTESIAN_POINT('Ctrl Pts',(-2.54195715546749,1.98138804991861,56.9488978815025));
#20098=CARTESIAN_POINT('Ctrl Pts',(-2.51939736447835,2.00999540746983,56.9466831250393));
#20099=CARTESIAN_POINT('Ctrl Pts',(-2.47396421076819,2.06564091951147,56.9422776840643));
#20100=CARTESIAN_POINT('Ctrl Pts',(-2.45112050867779,2.09269668577328,56.9400883731959));
#20101=CARTESIAN_POINT('Ctrl Pts',(-2.39414436143811,2.15796550523621,56.9346866658749));
#20102=CARTESIAN_POINT('Ctrl Pts',(-2.35953845406876,2.19575047575958,56.9314550773603));
#20103=CARTESIAN_POINT('Ctrl Pts',(-2.28268710674562,2.27574635443214,56.9243785670789));
#20104=CARTESIAN_POINT('Ctrl Pts',(-2.24013988672676,2.31763985149693,56.92052190858));
#20105=CARTESIAN_POINT('Ctrl Pts',(-2.10617269548767,2.44241185593695,56.9085637623392));
#20106=CARTESIAN_POINT('Ctrl Pts',(-2.01114259494639,2.5212378215737,56.9003279005751));
#20107=CARTESIAN_POINT('Ctrl Pts',(-1.74157465162653,2.71988341876357,56.8777719394522));
#20108=CARTESIAN_POINT('Ctrl Pts',(-1.55936847360893,2.82829066686042,56.8633370472115));
#20109=CARTESIAN_POINT('Ctrl Pts',(-1.33672482780621,2.93265505104793,56.8474569318508));
#20110=CARTESIAN_POINT('Ctrl Pts',(-1.30537064805736,2.9467450862445,56.8452595700417));
#20111=CARTESIAN_POINT('Ctrl Pts',(-1.25470173153,2.96854732247601,56.8417775242171));
#20112=CARTESIAN_POINT('Ctrl Pts',(-1.23552809244358,2.97657857868915,56.8404754846363));
#20113=CARTESIAN_POINT('Ctrl Pts',(-1.1968534942814,2.99234009235655,56.8378823438486));
#20114=CARTESIAN_POINT('Ctrl Pts',(-1.1773521324151,3.00006658724949,56.8365914816703));
#20115=CARTESIAN_POINT('Ctrl Pts',(-1.12485122755343,3.02027680299959,56.8331573613142));
#20116=CARTESIAN_POINT('Ctrl Pts',(-1.09171892556598,3.03241030654612,56.8310333309168));
#20117=CARTESIAN_POINT('Ctrl Pts',(-1.01609885996644,3.0587032671405,56.8262686762409));
#20118=CARTESIAN_POINT('Ctrl Pts',(-0.973501345665638,3.07252633167772,
56.8236433648069));
#20119=CARTESIAN_POINT('Ctrl Pts',(-0.827895540025725,3.11644357669647,
56.8148247065277));
#20120=CARTESIAN_POINT('Ctrl Pts',(-0.723673924140468,3.142281051443,56.8087715379145));
#20121=CARTESIAN_POINT('Ctrl Pts',(-0.390197211506187,3.20747690972804,
56.7897022532714));
#20122=CARTESIAN_POINT('Ctrl Pts',(-0.157906703169872,3.22726164570263,
56.7768038713047));
#20123=CARTESIAN_POINT('Ctrl Pts',(0.129603295213574,3.22061488165758,56.7598751109661));
#20124=CARTESIAN_POINT('Ctrl Pts',(0.184677365624063,3.21792650188442,56.7565919510726));
#20125=CARTESIAN_POINT('Ctrl Pts',(0.275665038386236,3.21114160687779,56.7510866568729));
#20126=CARTESIAN_POINT('Ctrl Pts',(0.311628104763981,3.20785121143749,56.7488896459302));
#20127=CARTESIAN_POINT('Ctrl Pts',(0.382975766200873,3.20011226519172,56.7444855927078));
#20128=CARTESIAN_POINT('Ctrl Pts',(0.418356890651453,3.1956793171569,56.7422793357473));
#20129=CARTESIAN_POINT('Ctrl Pts',(0.505773843253056,3.18325015559359,56.7367700172121));
#20130=CARTESIAN_POINT('Ctrl Pts',(0.557699591627092,3.17456443976123,56.733445955008));
#20131=CARTESIAN_POINT('Ctrl Pts',(0.806608589090579,3.1266337793043,56.7172543094878));
#20132=CARTESIAN_POINT('Ctrl Pts',(0.999819630099894,3.07030857137375,56.7038641530815));
#20133=CARTESIAN_POINT('Ctrl Pts',(1.35963244771787,2.92783020926508,56.6777450358051));
#20134=CARTESIAN_POINT('Ctrl Pts',(1.5265029539427,2.84439590346127,56.6650967169967));
#20135=CARTESIAN_POINT('Ctrl Pts',(1.71661144367588,2.72776778437452,56.6506554727207));
#20136=CARTESIAN_POINT('Ctrl Pts',(1.74765021781395,2.70798650536941,56.6482974431587));
#20137=CARTESIAN_POINT('Ctrl Pts',(1.79609969212866,2.67592912955357,56.6446245549487));
#20138=CARTESIAN_POINT('Ctrl Pts',(1.81373833918672,2.66400527528795,56.6432890789227));
#20139=CARTESIAN_POINT('Ctrl Pts',(1.8481438813376,2.64024674046124,56.6406895042798));
#20140=CARTESIAN_POINT('Ctrl Pts',(1.86491822502484,2.62842513765273,56.6394247663321));
#20141=CARTESIAN_POINT('Ctrl Pts',(1.90841623696524,2.59714415319372,56.6361490092902));
#20142=CARTESIAN_POINT('Ctrl Pts',(1.93495626078633,2.57743181221607,56.6341541772658));
#20143=CARTESIAN_POINT('Ctrl Pts',(2.09500673429521,2.45469001099885,56.6221165519411));
#20144=CARTESIAN_POINT('Ctrl Pts',(2.22057847839881,2.34170885431434,56.6126301846416));
#20145=CARTESIAN_POINT('Ctrl Pts',(2.48613639395769,2.06211156412784,56.5910138039755));
#20146=CARTESIAN_POINT('Ctrl Pts',(2.61925587011288,1.8901500982262,56.5789313584732));
#20147=CARTESIAN_POINT('Ctrl Pts',(2.76411827132919,1.65800636262168,56.5628460336113));
#20148=CARTESIAN_POINT('Ctrl Pts',(2.7928697056949,1.60910321326351,56.5594721116918));
#20149=CARTESIAN_POINT('Ctrl Pts',(2.83793300675741,1.52760580019844,56.5538572944632));
#20150=CARTESIAN_POINT('Ctrl Pts',(2.85500963846013,1.49544743465277,56.5516437263571));
#20151=CARTESIAN_POINT('Ctrl Pts',(2.88761827610561,1.43144440699284,56.5472384712733));
#20152=CARTESIAN_POINT('Ctrl Pts',(2.90317726564428,1.39961923573217,56.545048120027));
#20153=CARTESIAN_POINT('Ctrl Pts',(2.93998530508501,1.32107446127606,56.5396397382782));
#20154=CARTESIAN_POINT('Ctrl Pts',(2.96064838831183,1.27409260556704,56.536402404589));
#20155=CARTESIAN_POINT('Ctrl Pts',(3.00295635081758,1.17130336132989,56.5293109042868));
#20156=CARTESIAN_POINT('Ctrl Pts',(3.02418580093954,1.11534655708579,56.5254449083658));
#20157=CARTESIAN_POINT('Ctrl Pts',(3.08454914157848,0.941819233628293,56.513442553246));
#20158=CARTESIAN_POINT('Ctrl Pts',(3.11846936556817,0.822563823904482,56.5051706797111));
#20159=CARTESIAN_POINT('Ctrl Pts',(3.19124924603733,0.496302722796112,56.4826510771134));
#20160=CARTESIAN_POINT('Ctrl Pts',(3.21684046069395,0.286941853983922,56.4682934616393));
#20161=CARTESIAN_POINT('Ctrl Pts',(3.22265983724127,0.0420849375795456,
56.4524734239454));
#20162=CARTESIAN_POINT('Ctrl Pts',(3.22292572783027,0.00758564547516927,
56.4502677627509));
#20163=CARTESIAN_POINT('Ctrl Pts',(3.2224638228948,-0.047724523493845,56.4467758529688));
#20164=CARTESIAN_POINT('Ctrl Pts',(3.22208841634583,-0.0685347891252205,
56.4454720857196));
#20165=CARTESIAN_POINT('Ctrl Pts',(3.22093070862584,-0.110280263771302,
56.4428788483934));
#20166=CARTESIAN_POINT('Ctrl Pts',(3.22014583698556,-0.131214371300375,
56.4415895669234));
#20167=CARTESIAN_POINT('Ctrl Pts',(3.21749759655341,-0.187248952041684,
56.4381648739455));
#20168=CARTESIAN_POINT('Ctrl Pts',(3.21526399231875,-0.222330025129312,
56.4360485061869));
#20169=CARTESIAN_POINT('Ctrl Pts',(3.19972431648013,-0.416294782983535,
56.4244662067931));
#20170=CARTESIAN_POINT('Ctrl Pts',(3.17521441052865,-0.574074312448822,
56.4154812662513));
#20171=CARTESIAN_POINT('Ctrl Pts',(3.08857924390017,-0.946923869543753,
56.3940145063559));
#20172=CARTESIAN_POINT('Ctrl Pts',(3.01557093985495,-1.15858050863655,56.3815966511459));
#20173=CARTESIAN_POINT('Ctrl Pts',(2.89756360208515,-1.41187637228609,56.3651621607647));
#20174=CARTESIAN_POINT('Ctrl Pts',(2.87252896379868,-1.46213765235327,56.3618212353156));
#20175=CARTESIAN_POINT('Ctrl Pts',(2.82916747646319,-1.54377676857688,56.3562462819122));
#20176=CARTESIAN_POINT('Ctrl Pts',(2.811599648374,-1.57554516710002,56.3540387727067));
#20177=CARTESIAN_POINT('Ctrl Pts',(2.77579566901384,-1.63778401756406,56.349634282699));
#20178=CARTESIAN_POINT('Ctrl Pts',(2.75758509697339,-1.66826327601977,56.34743844144));
#20179=CARTESIAN_POINT('Ctrl Pts',(2.71158632281412,-1.74244035037105,56.3419949712612));
#20180=CARTESIAN_POINT('Ctrl Pts',(2.68324212780437,-1.7857799281773,56.3387274525053));
#20181=CARTESIAN_POINT('Ctrl Pts',(2.54161483072516,-1.99134587978948,56.322794573898));
#20182=CARTESIAN_POINT('Ctrl Pts',(2.41461308575272,-2.14356864449937,56.3096211050842));
#20183=CARTESIAN_POINT('Ctrl Pts',(2.13873446261977,-2.41839745623974,56.2833484804977));
#20184=CARTESIAN_POINT('Ctrl Pts',(1.99119116298506,-2.54125923587026,56.2703189992719));
#20185=CARTESIAN_POINT('Ctrl Pts',(1.80357338840829,-2.67106225735202,56.2555512535026));
#20186=CARTESIAN_POINT('Ctrl Pts',(1.77319630560614,-2.69132414793122,56.2532125159911));
#20187=CARTESIAN_POINT('Ctrl Pts',(1.7246211812975,-2.7225447720268,56.2495625052813));
#20188=CARTESIAN_POINT('Ctrl Pts',(1.70664875693812,-2.73384680148835,56.2482310172543));
#20189=CARTESIAN_POINT('Ctrl Pts',(1.67104724562507,-2.7557470272628,56.2456326608416));
#20190=CARTESIAN_POINT('Ctrl Pts',(1.65342599662417,-2.76635556015612,56.2443652523415));
#20191=CARTESIAN_POINT('Ctrl Pts',(1.60702002156084,-2.79369155064803,56.2410728881965));
#20192=CARTESIAN_POINT('Ctrl Pts',(1.57807467715588,-2.81014347297185,56.2390644333779));
#20193=CARTESIAN_POINT('Ctrl Pts',(1.51255487041812,-2.84605182978926,56.2346067184971));
#20194=CARTESIAN_POINT('Ctrl Pts',(1.47584939481442,-2.86525777431323,56.2321699655945));
#20195=CARTESIAN_POINT('Ctrl Pts',(1.35489777665518,-2.92560383677135,56.2243033348266));
#20196=CARTESIAN_POINT('Ctrl Pts',(1.26922212481919,-2.9637784934947,56.2189834736516));
#20197=CARTESIAN_POINT('Ctrl Pts',(0.938244169545973,-3.09426357872117,
56.1989557983675));
#20198=CARTESIAN_POINT('Ctrl Pts',(0.683702014462386,-3.16027086118547,
56.1845209890317));
#20199=CARTESIAN_POINT('Ctrl Pts',(0.373369530560781,-3.20145583187507,
56.1660234575779));
#20200=CARTESIAN_POINT('Ctrl Pts',(0.322607334643781,-3.2069687136015,56.1629735674045));
#20201=CARTESIAN_POINT('Ctrl Pts',(0.236835962114637,-3.21422667775019,
56.1577684634486));
#20202=CARTESIAN_POINT('Ctrl Pts',(0.20188961603973,-3.21661076956348,56.1556333296901));
#20203=CARTESIAN_POINT('Ctrl Pts',(0.130567843740047,-3.22030962469205,
56.1512432720793));
#20204=CARTESIAN_POINT('Ctrl Pts',(0.094195227287036,-3.22157867017424,
56.1489872489192));
#20205=CARTESIAN_POINT('Ctrl Pts',(0.00118407400272861,-3.22324738345739,
56.1431712266743));
#20206=CARTESIAN_POINT('Ctrl Pts',(-0.0554557993264142,-3.22277040920566,
56.1395848593229));
#20207=CARTESIAN_POINT('Ctrl Pts',(-0.238862715804239,-3.21638972139729,
56.1278211027386));
#20208=CARTESIAN_POINT('Ctrl Pts',(-0.365258903978403,-3.2044940322575,
56.1194749953687));
#20209=CARTESIAN_POINT('Ctrl Pts',(-0.490582206601849,-3.18519177775306,
56.1109990110886));
#20210=CARTESIAN_POINT('Origin',(-9.35406549764863E-15,0.,41.4527091182931));
#20211=CARTESIAN_POINT('',(-0.490582094190866,-3.18519179506656,54.6110712720502));
#20212=CARTESIAN_POINT('',(-0.490582094360392,-3.18519179504045,54.8568649631546));
#20213=CARTESIAN_POINT('',(-0.490582094296226,-3.18519179505033,41.4527091182931));
#20214=CARTESIAN_POINT('',(-3.22274988921121,-0.000845038000876335,55.5782875026161));
#20215=CARTESIAN_POINT('Ctrl Pts',(-0.490582094190866,-3.18519179506656,
54.6110712720502));
#20216=CARTESIAN_POINT('Ctrl Pts',(-0.488218115883238,-3.1855558941549,
54.611227721965));
#20217=CARTESIAN_POINT('Ctrl Pts',(-0.485853718871332,-3.18591736356377,
54.6113842388328));
#20218=CARTESIAN_POINT('Ctrl Pts',(-0.351460153215834,-3.20631038479086,
54.6202829572151));
#20219=CARTESIAN_POINT('Ctrl Pts',(-0.218324002549986,-3.21811745328552,
54.6292281850042));
#20220=CARTESIAN_POINT('Ctrl Pts',(0.106064238668979,-3.2266610217964,54.651122488147));
#20221=CARTESIAN_POINT('Ctrl Pts',(0.297058771535315,-3.21470938461955,
54.6641076547093));
#20222=CARTESIAN_POINT('Ctrl Pts',(0.522018803503048,-3.18040096678932,
54.6788384446438));
#20223=CARTESIAN_POINT('Ctrl Pts',(0.558062842856231,-3.17427473015587,
54.6811802521084));
#20224=CARTESIAN_POINT('Ctrl Pts',(0.614871191674995,-3.1636216676205,54.6848338705702));
#20225=CARTESIAN_POINT('Ctrl Pts',(0.635707347140247,-3.15950073048629,
54.6861659607087));
#20226=CARTESIAN_POINT('Ctrl Pts',(0.676629338688906,-3.15098602866014,
54.6887643975192));
#20227=CARTESIAN_POINT('Ctrl Pts',(0.696716634985155,-3.14660550133401,
54.6900313007804));
#20228=CARTESIAN_POINT('Ctrl Pts',(0.7491778894538,-3.1346380312295,54.693320715881));
#20229=CARTESIAN_POINT('Ctrl Pts',(0.781479750868551,-3.12674154523719,
54.6953267815058));
#20230=CARTESIAN_POINT('Ctrl Pts',(0.853668320567097,-3.10790573043213,
54.6997782296994));
#20231=CARTESIAN_POINT('Ctrl Pts',(0.893478717135233,-3.0966956109964,54.7022111589021));
#20232=CARTESIAN_POINT('Ctrl Pts',(1.02254588647406,-3.05765548667885,54.7100593276068));
#20233=CARTESIAN_POINT('Ctrl Pts',(1.11081292321616,-3.02670675312847,54.7153651018596));
#20234=CARTESIAN_POINT('Ctrl Pts',(1.44143606593318,-2.89436590925381,54.7354142972265));
#20235=CARTESIAN_POINT('Ctrl Pts',(1.67239317729549,-2.7673424425744,54.7498808505692));
#20236=CARTESIAN_POINT('Ctrl Pts',(1.92670902215607,-2.58389379516368,54.7684109264884));
#20237=CARTESIAN_POINT('Ctrl Pts',(1.96732617105176,-2.55310440683157,54.7714555112382));
#20238=CARTESIAN_POINT('Ctrl Pts',(2.03458496251802,-2.49956141516522,54.7766542789936));
#20239=CARTESIAN_POINT('Ctrl Pts',(2.06161727853339,-2.47731251277647,54.7787884994527));
#20240=CARTESIAN_POINT('Ctrl Pts',(2.11601605908315,-2.43103261822754,54.783179005822));
#20241=CARTESIAN_POINT('Ctrl Pts',(2.14334828081445,-2.40696936587802,54.7854364297395));
#20242=CARTESIAN_POINT('Ctrl Pts',(2.21221951650372,-2.34423185932014,54.7912612898189));
#20243=CARTESIAN_POINT('Ctrl Pts',(2.25315393433647,-2.30491537869107,54.7948552562641));
#20244=CARTESIAN_POINT('Ctrl Pts',(2.40874120755135,-2.14737091506546,54.8090500962703));
#20245=CARTESIAN_POINT('Ctrl Pts',(2.5152899636175,-2.02151923606187,54.8199723345397));
#20246=CARTESIAN_POINT('Ctrl Pts',(2.73021884882513,-1.72421430528529,54.8446626096796));
#20247=CARTESIAN_POINT('Ctrl Pts',(2.83300785689257,-1.54954281128614,54.8584657211345));
#20248=CARTESIAN_POINT('Ctrl Pts',(2.93722615732429,-1.32692078660549,54.8744817813078));
#20249=CARTESIAN_POINT('Ctrl Pts',(2.95489954742953,-1.28708405060101,54.8772888476052));
#20250=CARTESIAN_POINT('Ctrl Pts',(2.98052022963348,-1.22602174445777,54.8814899085258));
#20251=CARTESIAN_POINT('Ctrl Pts',(2.98906003671107,-1.20505200055721,54.8829147095781));
#20252=CARTESIAN_POINT('Ctrl Pts',(3.00466203717626,-1.16555422660129,54.8855626242622));
#20253=CARTESIAN_POINT('Ctrl Pts',(3.01177528816914,-1.14704849148357,54.886788403533));
#20254=CARTESIAN_POINT('Ctrl Pts',(3.02893398960021,-1.10114836536465,54.889794254239));
#20255=CARTESIAN_POINT('Ctrl Pts',(3.03877926878053,-1.07368036595767,54.8915631270241));
#20256=CARTESIAN_POINT('Ctrl Pts',(3.07778227376683,-0.960026748210863,
54.8987741659585));
#20257=CARTESIAN_POINT('Ctrl Pts',(3.10365925895005,-0.872752596838835,
54.9040582613079));
#20258=CARTESIAN_POINT('Ctrl Pts',(3.177701441098,-0.577731922154442,54.9214352989276));
#20259=CARTESIAN_POINT('Ctrl Pts',(3.20895147900944,-0.366329106762467,
54.9331324619785));
#20260=CARTESIAN_POINT('Ctrl Pts',(3.22444208500906,-0.0412225616575212,
54.9516571341262));
#20261=CARTESIAN_POINT('Ctrl Pts',(3.22392043589067,0.0711311809176215,
54.958148622425));
#20262=CARTESIAN_POINT('Ctrl Pts',(3.21515817504531,0.225004222129187,54.967299187262));
#20263=CARTESIAN_POINT('Ctrl Pts',(3.21196533500696,0.266734771071235,54.9698067678853));
#20264=CARTESIAN_POINT('Ctrl Pts',(3.2046306230547,0.343032554627598,54.9744454551272));
#20265=CARTESIAN_POINT('Ctrl Pts',(3.20073950528671,0.377617844704507,54.9765685412857));
#20266=CARTESIAN_POINT('Ctrl Pts',(3.19158941898791,0.448581270669863,54.980969879876));
#20267=CARTESIAN_POINT('Ctrl Pts',(3.18626669841827,0.484945899457673,54.9832498333774));
#20268=CARTESIAN_POINT('Ctrl Pts',(3.17085844146737,0.578964055487841,54.9892113601973));
#20269=CARTESIAN_POINT('Ctrl Pts',(3.15982253884326,0.636445952793806,54.9929219746265));
#20270=CARTESIAN_POINT('Ctrl Pts',(3.13182434411174,0.763489837621306,55.0012740666996));
#20271=CARTESIAN_POINT('Ctrl Pts',(3.11409697861974,0.83285011229521,55.0059364133257));
#20272=CARTESIAN_POINT('Ctrl Pts',(3.04477199207156,1.07076776055898,55.0222720414879));
#20273=CARTESIAN_POINT('Ctrl Pts',(2.9816728753774,1.23563686823562,55.0342182951517));
#20274=CARTESIAN_POINT('Ctrl Pts',(2.84655902074834,1.51714327284305,55.0552756732612));
#20275=CARTESIAN_POINT('Ctrl Pts',(2.77998623611765,1.63594168325348,55.0643847445945));
#20276=CARTESIAN_POINT('Ctrl Pts',(2.68868265146704,1.77711326759151,55.0752135535526));
#20277=CARTESIAN_POINT('Ctrl Pts',(2.67086528292944,1.80378069270038,55.0772590136826));
#20278=CARTESIAN_POINT('Ctrl Pts',(2.64224617140743,1.84526108952761,55.0804350436958));
#20279=CARTESIAN_POINT('Ctrl Pts',(2.63171154252255,1.86025474453597,55.0815818802716));
#20280=CARTESIAN_POINT('Ctrl Pts',(2.60889596721909,1.89214578661093,55.0840171978852));
#20281=CARTESIAN_POINT('Ctrl Pts',(2.59657737887008,1.90901540513135,55.0853030019798));
#20282=CARTESIAN_POINT('Ctrl Pts',(2.56326421694991,1.95371681027129,55.0887071220249));
#20283=CARTESIAN_POINT('Ctrl Pts',(2.54198005792617,1.98133046896721,55.0908067924381));
#20284=CARTESIAN_POINT('Ctrl Pts',(2.49278897680459,2.04305217090431,55.0955063593431));
#20285=CARTESIAN_POINT('Ctrl Pts',(2.46462185836465,2.07694450967805,55.0980915619189));
#20286=CARTESIAN_POINT('Ctrl Pts',(2.36746817842859,2.18908466427151,55.1067014214772));
#20287=CARTESIAN_POINT('Ctrl Pts',(2.29537802043148,2.26456163854045,55.1125927844746));
#20288=CARTESIAN_POINT('Ctrl Pts',(2.04679223468783,2.5007349834269,55.1318464105637));
#20289=CARTESIAN_POINT('Ctrl Pts',(1.85613950081233,2.6453299153189,55.1450636770429));
#20290=CARTESIAN_POINT('Ctrl Pts',(1.60459149852999,2.79541763769887,55.1623181247083));
#20291=CARTESIAN_POINT('Ctrl Pts',(1.55720566281375,2.82208852818438,55.165557646386));
#20292=CARTESIAN_POINT('Ctrl Pts',(1.47738802898349,2.86439103105369,55.1710103759082));
#20293=CARTESIAN_POINT('Ctrl Pts',(1.44532749154622,2.88070124249163,55.1731994967862));
#20294=CARTESIAN_POINT('Ctrl Pts',(1.38084303808594,2.91215905463831,55.1776038667476));
#20295=CARTESIAN_POINT('Ctrl Pts',(1.34842647043407,2.92730998463742,55.1798186071413));
#20296=CARTESIAN_POINT('Ctrl Pts',(1.26707330265888,2.96369498773936,55.1853813329415));
#20297=CARTESIAN_POINT('Ctrl Pts',(1.21785056105438,2.98425907190415,55.1887512322334));
#20298=CARTESIAN_POINT('Ctrl Pts',(1.00023236152541,3.0688941050392,55.2036758173797));
#20299=CARTESIAN_POINT('Ctrl Pts',(0.82716517735864,3.11999313967493,55.2156371047934));
#20300=CARTESIAN_POINT('Ctrl Pts',(0.44563305019645,3.19865504127307,55.2418828576738));
#20301=CARTESIAN_POINT('Ctrl Pts',(0.236862671107257,3.22085221301945,55.2561720757712));
#20302=CARTESIAN_POINT('Ctrl Pts',(-0.00720010715993356,3.22292776502206,
55.2719388574884));
#20303=CARTESIAN_POINT('Ctrl Pts',(-0.0418101800208314,3.22266463527656,
55.2741518324622));
#20304=CARTESIAN_POINT('Ctrl Pts',(-0.0972398023030859,3.2213500387901,
55.2776524036174));
#20305=CARTESIAN_POINT('Ctrl Pts',(-0.11806418050657,3.22065405773964,55.2789576628939));
#20306=CARTESIAN_POINT('Ctrl Pts',(-0.159784173360221,3.21885450656175,
55.2815508983957));
#20307=CARTESIAN_POINT('Ctrl Pts',(-0.180678702375732,3.21774930334034,
55.2828387307623));
#20308=CARTESIAN_POINT('Ctrl Pts',(-0.236523009938695,3.21424976080671,
55.2862549481559));
#20309=CARTESIAN_POINT('Ctrl Pts',(-0.271447932757623,3.21148889198248,
55.2883644532032));
#20310=CARTESIAN_POINT('Ctrl Pts',(-0.467659118559107,3.19275419284158,
55.300098298393));
#20311=CARTESIAN_POINT('Ctrl Pts',(-0.627622114528567,3.16519922858504,
55.3092240629311));
#20312=CARTESIAN_POINT('Ctrl Pts',(-0.998528769734702,3.07206715490697,
55.3306661321348));
#20313=CARTESIAN_POINT('Ctrl Pts',(-1.20612623910482,2.99664915791563,55.3429263936251));
#20314=CARTESIAN_POINT('Ctrl Pts',(-1.45519184959555,2.8760595511611,55.3591973130293));
#20315=CARTESIAN_POINT('Ctrl Pts',(-1.5053244718323,2.85014026515908,55.3625545474207));
#20316=CARTESIAN_POINT('Ctrl Pts',(-1.5865921549261,2.8053813435495,55.3681491350678));
#20317=CARTESIAN_POINT('Ctrl Pts',(-1.61813548670954,2.78730632152881,55.3703595700089));
#20318=CARTESIAN_POINT('Ctrl Pts',(-1.67983096543237,2.75055322182661,55.3747642135771));
#20319=CARTESIAN_POINT('Ctrl Pts',(-1.70999393280832,2.73190330900102,55.3769571843854));
#20320=CARTESIAN_POINT('Ctrl Pts',(-1.7832308407509,2.68493245518761,55.3823826924286));
#20321=CARTESIAN_POINT('Ctrl Pts',(-1.8259435900971,2.65606928378936,55.3856348208993));
#20322=CARTESIAN_POINT('Ctrl Pts',(-1.91699804750518,2.59130463791565,55.3927650003643));
#20323=CARTESIAN_POINT('Ctrl Pts',(-1.96506230900659,2.5550480704773,55.3966551219498));
#20324=CARTESIAN_POINT('Ctrl Pts',(-2.10991110106341,2.4392780155006,55.4087724047032));
#20325=CARTESIAN_POINT('Ctrl Pts',(-2.20309280971632,2.35545741010476,55.4171380706289));
#20326=CARTESIAN_POINT('Ctrl Pts',(-2.43713927062181,2.11885818303161,55.439563752036));
#20327=CARTESIAN_POINT('Ctrl Pts',(-2.56853123956947,1.95751502339181,55.4537213442129));
#20328=CARTESIAN_POINT('Ctrl Pts',(-2.70277920996137,1.75565220021036,55.4693856091766));
#20329=CARTESIAN_POINT('Ctrl Pts',(-2.72159191814923,1.72634520396884,55.471612745882));
#20330=CARTESIAN_POINT('Ctrl Pts',(-2.75091945432572,1.67898649887106,55.4751301590685));
#20331=CARTESIAN_POINT('Ctrl Pts',(-2.7617397357215,1.6611282900715,55.4764383782975));
#20332=CARTESIAN_POINT('Ctrl Pts',(-2.78303070629782,1.62520568494068,55.4790318885782));
#20333=CARTESIAN_POINT('Ctrl Pts',(-2.7935009461426,1.60714216865211,55.4803171198939));
#20334=CARTESIAN_POINT('Ctrl Pts',(-2.82095965793227,1.55869050692258,55.4837178237241));
#20335=CARTESIAN_POINT('Ctrl Pts',(-2.83763298748904,1.52812589044978,55.48581471675));
#20336=CARTESIAN_POINT('Ctrl Pts',(-2.92810354252212,1.35569125747713,55.4974102114491));
#20337=CARTESIAN_POINT('Ctrl Pts',(-2.99176434782105,1.20873743676747,55.506422547652));
#20338=CARTESIAN_POINT('Ctrl Pts',(-3.11764965582723,0.84639941413445,55.5279344931588));
#20339=CARTESIAN_POINT('Ctrl Pts',(-3.16884980097137,0.628102370317696,
55.5403697591376));
#20340=CARTESIAN_POINT('Ctrl Pts',(-3.20397397894642,0.35170175904735,55.5567576483647));
#20341=CARTESIAN_POINT('Ctrl Pts',(-3.20950983955604,0.296967088794769,
55.5600304232696));
#20342=CARTESIAN_POINT('Ctrl Pts',(-3.21638275917703,0.205743228111225,
55.5655451551488));
#20343=CARTESIAN_POINT('Ctrl Pts',(-3.21850548643902,0.169323938624154,
55.567762617296));
#20344=CARTESIAN_POINT('Ctrl Pts',(-3.22098376837375,0.109267967967994,
55.5714483292774));
#20345=CARTESIAN_POINT('Ctrl Pts',(-3.22169833283886,0.0856488782510573,
55.5729052527132));
#20346=CARTESIAN_POINT('Ctrl Pts',(-3.22255645023745,0.0410699880881085,
55.5756697160235));
#20347=CARTESIAN_POINT('Ctrl Pts',(-3.22275538448412,0.0201124694179753,
55.5769754575503));
#20348=CARTESIAN_POINT('Ctrl Pts',(-3.22274988921121,-0.000845038000876335,
55.5782875026161));
#20349=CARTESIAN_POINT('Ctrl Pts',(-3.2227498896419,-0.000843393838916127,
55.5782873996834));
#20350=CARTESIAN_POINT('Ctrl Pts',(-3.22274288764006,-0.0275992220640488,
55.5799624482896));
#20351=CARTESIAN_POINT('Ctrl Pts',(-3.2224026891714,-0.0543534235100241,
55.5816476755399));
#20352=CARTESIAN_POINT('Ctrl Pts',(-3.22071865370461,-0.121252538950575,
55.5858879877087));
#20353=CARTESIAN_POINT('Ctrl Pts',(-3.2189573858021,-0.161381378275452,
55.5884553222044));
#20354=CARTESIAN_POINT('Ctrl Pts',(-3.20369698711565,-0.40501746016145,
55.6041886682182));
#20355=CARTESIAN_POINT('Ctrl Pts',(-3.17165512760259,-0.606874403716984,
55.6178876259209));
#20356=CARTESIAN_POINT('Ctrl Pts',(-3.07882886738486,-0.9670399381762,55.6430118722649));
#20357=CARTESIAN_POINT('Ctrl Pts',(-3.02422566227135,-1.1262423935776,55.6543629498995));
#20358=CARTESIAN_POINT('Ctrl Pts',(-2.94421363512423,-1.3110429138473,55.6673528114193));
#20359=CARTESIAN_POINT('Ctrl Pts',(-2.9305029700883,-1.34140970404138,55.6694804781047));
#20360=CARTESIAN_POINT('Ctrl Pts',(-2.90756845006362,-1.39017496879325,
55.6728798093302));
#20361=CARTESIAN_POINT('Ctrl Pts',(-2.898635233766,-1.40870670787885,55.6741674727357));
#20362=CARTESIAN_POINT('Ctrl Pts',(-2.88012690263248,-1.44618012740074,
55.6767609413572));
#20363=CARTESIAN_POINT('Ctrl Pts',(-2.87054099256361,-1.4651151505743,55.6780660647625));
#20364=CARTESIAN_POINT('Ctrl Pts',(-2.8439724507588,-1.51633399517883,55.6815855398929));
#20365=CARTESIAN_POINT('Ctrl Pts',(-2.8266271669469,-1.54842732962711,55.6837789652586));
#20366=CARTESIAN_POINT('Ctrl Pts',(-2.7145897948392,-1.74756649714963,55.697357630424));
#20367=CARTESIAN_POINT('Ctrl Pts',(-2.60566127469289,-1.9061826603677,55.7080484664413));
#20368=CARTESIAN_POINT('Ctrl Pts',(-2.35937874486132,-2.20390894904481,
55.7296939621426));
#20369=CARTESIAN_POINT('Ctrl Pts',(-2.22223501455478,-2.34212389944741,
55.7406156173946));
#20370=CARTESIAN_POINT('Ctrl Pts',(-2.03273493147719,-2.50138757836204,
55.7552119021853));
#20371=CARTESIAN_POINT('Ctrl Pts',(-1.99114402250642,-2.53461952182791,
55.7583862970687));
#20372=CARTESIAN_POINT('Ctrl Pts',(-1.92026818942323,-2.58842935473143,
55.7637609130451));
#20373=CARTESIAN_POINT('Ctrl Pts',(-1.8914284429096,-2.60957750047474,55.7659385696278));
#20374=CARTESIAN_POINT('Ctrl Pts',(-1.83286989453582,-2.65103769142701,
55.7703452258239));
#20375=CARTESIAN_POINT('Ctrl Pts',(-1.80315084620381,-2.67134044096244,
55.7725741488184));
#20376=CARTESIAN_POINT('Ctrl Pts',(-1.72760165192969,-2.72111717745418,
55.77822470734));
#20377=CARTESIAN_POINT('Ctrl Pts',(-1.68135385394976,-2.74993360047054,
55.7816697758867));
#20378=CARTESIAN_POINT('Ctrl Pts',(-1.42952675426891,-2.89811611484992,
55.8003649843496));
#20379=CARTESIAN_POINT('Ctrl Pts',(-1.21197332966864,-2.99561514582695,
55.8163704929202));
#20380=CARTESIAN_POINT('Ctrl Pts',(-0.886011331371105,-3.100333893371,55.8394895939961));
#20381=CARTESIAN_POINT('Ctrl Pts',(-0.784791778974033,-3.12748943776473,
55.8465437945079));
#20382=CARTESIAN_POINT('Ctrl Pts',(-0.639262530915241,-3.15902065320963,
55.8563762400436));
#20383=CARTESIAN_POINT('Ctrl Pts',(-0.595909771719696,-3.16748480194819,
55.8592666350033));
#20384=CARTESIAN_POINT('Ctrl Pts',(-0.531824175297743,-3.17863438760384,
55.863470131914));
#20385=CARTESIAN_POINT('Ctrl Pts',(-0.511218946646582,-3.18201331447733,
55.8648111988455));
#20386=CARTESIAN_POINT('Ctrl Pts',(-0.490582094113513,-3.18519179507847,
55.8661429281184));
#20387=CARTESIAN_POINT('',(-3.22274963550475,-0.0023652837118349,55.8259788468706));
#20388=CARTESIAN_POINT('Ctrl Pts',(-0.49058220660185,-3.18519177775306,
56.1109990110886));
#20389=CARTESIAN_POINT('Ctrl Pts',(-0.527035938123794,-3.17957718582367,
56.1085335377979));
#20390=CARTESIAN_POINT('Ctrl Pts',(-0.563398927501597,-3.17333592017435,
56.1060575984741));
#20391=CARTESIAN_POINT('Ctrl Pts',(-0.796465884766915,-3.12919850823935,
56.0900953600583));
#20392=CARTESIAN_POINT('Ctrl Pts',(-0.989378531457401,-3.0736586133384,
56.0764232066526));
#20393=CARTESIAN_POINT('Ctrl Pts',(-1.2182107367988,-2.98398159018331,56.0603845464486));
#20394=CARTESIAN_POINT('Ctrl Pts',(-1.26017687552495,-2.96650269469745,
56.0574525416929));
#20395=CARTESIAN_POINT('Ctrl Pts',(-1.32279957160357,-2.93885143421542,
56.053106105014));
#20396=CARTESIAN_POINT('Ctrl Pts',(-1.3437383898767,-2.92933672895247,56.0516577533548));
#20397=CARTESIAN_POINT('Ctrl Pts',(-1.38244238719976,-2.91124709052142,
56.0489922228911));
#20398=CARTESIAN_POINT('Ctrl Pts',(-1.40023254369973,-2.90273240534161,
56.0477719377583));
#20399=CARTESIAN_POINT('Ctrl Pts',(-1.44349863930908,-2.88153413959549,
56.0448144440116));
#20400=CARTESIAN_POINT('Ctrl Pts',(-1.4688866149837,-2.86867557584027,56.0430875900951));
#20401=CARTESIAN_POINT('Ctrl Pts',(-1.56820833451165,-2.81670649430969,
56.0363528461759));
#20402=CARTESIAN_POINT('Ctrl Pts',(-1.64078337656342,-2.77505766260991,
56.0314777162139));
#20403=CARTESIAN_POINT('Ctrl Pts',(-1.85995454523111,-2.63767291986913,
56.0166480833059));
#20404=CARTESIAN_POINT('Ctrl Pts',(-2.0004349232622,-2.53278794508391,56.006974110287));
#20405=CARTESIAN_POINT('Ctrl Pts',(-2.24541729786842,-2.31672312410082,
55.9885819914824));
#20406=CARTESIAN_POINT('Ctrl Pts',(-2.35189683224743,-2.20854688599951,
55.9799334391777));
#20407=CARTESIAN_POINT('Ctrl Pts',(-2.48261416030586,-2.05553158101331,
55.9680256366292));
#20408=CARTESIAN_POINT('Ctrl Pts',(-2.51398831649961,-2.01703879449303,
55.9650559859045));
#20409=CARTESIAN_POINT('Ctrl Pts',(-2.56581365002936,-1.95036626671955,
55.9599453173604));
#20410=CARTESIAN_POINT('Ctrl Pts',(-2.58672080573658,-1.92255132255864,
55.9578226057174));
#20411=CARTESIAN_POINT('Ctrl Pts',(-2.62878586494356,-1.86465930245229,
55.953420526404));
#20412=CARTESIAN_POINT('Ctrl Pts',(-2.64988747072764,-1.83454780620086,
55.9511394322938));
#20413=CARTESIAN_POINT('Ctrl Pts',(-2.7032776208159,-1.75551777622357,55.9451713118334));
#20414=CARTESIAN_POINT('Ctrl Pts',(-2.7347538836124,-1.7060694726035,55.9414551235481));
#20415=CARTESIAN_POINT('Ctrl Pts',(-2.80170958235842,-1.59426604139773,
55.9330879108246));
#20416=CARTESIAN_POINT('Ctrl Pts',(-2.83648992433679,-1.53153013190146,
55.9284158944086));
#20417=CARTESIAN_POINT('Ctrl Pts',(-2.88940044191937,-1.42809679512133,
55.9207565769007));
#20418=CARTESIAN_POINT('Ctrl Pts',(-2.90883162626377,-1.38808995565332,
55.9178043519347));
#20419=CARTESIAN_POINT('Ctrl Pts',(-3.02222465732457,-1.14178053141678,
55.8997066447939));
#20420=CARTESIAN_POINT('Ctrl Pts',(-3.09502800721153,-0.926446943796116,
55.8841573814485));
#20421=CARTESIAN_POINT('Ctrl Pts',(-3.15710934938906,-0.649636544659183,
55.8654938365189));
#20422=CARTESIAN_POINT('Ctrl Pts',(-3.16810694615104,-0.593688732898751,
55.8617902145876));
#20423=CARTESIAN_POINT('Ctrl Pts',(-3.18178388576271,-0.512829088650184,
55.8565624849481));
#20424=CARTESIAN_POINT('Ctrl Pts',(-3.18566590138256,-0.488134434512769,
55.8549825768815));
#20425=CARTESIAN_POINT('Ctrl Pts',(-3.19206108095442,-0.444120497028435,
55.8521991974741));
#20426=CARTESIAN_POINT('Ctrl Pts',(-3.19468695256116,-0.424820289713105,
55.8509900062762));
#20427=CARTESIAN_POINT('Ctrl Pts',(-3.19954298916008,-0.38653279932615,
55.84861325251));
#20428=CARTESIAN_POINT('Ctrl Pts',(-3.20177939753818,-0.36754819363111,
55.8474452333136));
#20429=CARTESIAN_POINT('Ctrl Pts',(-3.20662700924488,-0.322988561302356,
55.84472592308));
#20430=CARTESIAN_POINT('Ctrl Pts',(-3.20910142055447,-0.297399641046346,
55.8431814292897));
#20431=CARTESIAN_POINT('Ctrl Pts',(-3.21885286366528,-0.182180850534396,
55.8362930114648));
#20432=CARTESIAN_POINT('Ctrl Pts',(-3.22268324456027,-0.0922947409880173,
55.8310977937728));
#20433=CARTESIAN_POINT('Ctrl Pts',(-3.22274913503596,-0.00236117027106857,
55.8259777403464));
#20434=CARTESIAN_POINT('Ctrl Pts',(-3.22274913198354,-0.0023653328352537,
55.8259779773275));
#20435=CARTESIAN_POINT('Ctrl Pts',(-3.2228229772883,0.0982483686585223,
55.8202498852851));
#20436=CARTESIAN_POINT('Ctrl Pts',(-3.21818507087071,0.198815352652257,
55.8146211056984));
#20437=CARTESIAN_POINT('Ctrl Pts',(-3.1899723467413,0.501587428547368,55.7975878224515));
#20438=CARTESIAN_POINT('Ctrl Pts',(-3.15195669874257,0.7019056765601,55.7861689506042));
#20439=CARTESIAN_POINT('Ctrl Pts',(-3.08100654171627,0.946655981404647,
55.771116825202));
#20440=CARTESIAN_POINT('Ctrl Pts',(-3.06551922547341,0.995665757241424,
55.7680475947046));
#20441=CARTESIAN_POINT('Ctrl Pts',(-3.03738470469542,1.07780678037972,55.7627982896777));
#20442=CARTESIAN_POINT('Ctrl Pts',(-3.02535030728503,1.11113845408135,55.7606383831365));
#20443=CARTESIAN_POINT('Ctrl Pts',(-2.99984781661115,1.17828477790705,55.7562232213153));
#20444=CARTESIAN_POINT('Ctrl Pts',(-2.9863516480399,1.21208316678579,55.7539672903639));
#20445=CARTESIAN_POINT('Ctrl Pts',(-2.95039889775408,1.29787157203897,55.7481518282855));
#20446=CARTESIAN_POINT('Ctrl Pts',(-2.92713978260316,1.34950966125318,55.7445659390009));
#20447=CARTESIAN_POINT('Ctrl Pts',(-2.80775960541484,1.59692382822402,55.72695676684));
#20448=CARTESIAN_POINT('Ctrl Pts',(-2.69330580822685,1.78318728664743,55.7123201359199));
#20449=CARTESIAN_POINT('Ctrl Pts',(-2.45953151085422,2.08919383284132,55.6863076360253));
#20450=CARTESIAN_POINT('Ctrl Pts',(-2.34793756856334,2.21387094349798,55.6750248556402));
#20451=CARTESIAN_POINT('Ctrl Pts',(-2.20304183693845,2.35241125151116,55.6620925586476));
#20452=CARTESIAN_POINT('Ctrl Pts',(-2.17855464697723,2.37510670989627,55.6599603613078));
#20453=CARTESIAN_POINT('Ctrl Pts',(-2.13840448373938,2.41117556174831,55.6565556302991));
#20454=CARTESIAN_POINT('Ctrl Pts',(-2.12295873902952,2.42478609140215,55.6552670106535));
#20455=CARTESIAN_POINT('Ctrl Pts',(-2.09133894538991,2.45211514403191,55.6526735279007));
#20456=CARTESIAN_POINT('Ctrl Pts',(-2.07515791596265,2.46582378650117,55.6513693174119));
#20457=CARTESIAN_POINT('Ctrl Pts',(-2.03084080818286,2.50262420511306,55.6478554726257));
#20458=CARTESIAN_POINT('Ctrl Pts',(-2.00244616786446,2.52540133324973,55.6456666498142));
#20459=CARTESIAN_POINT('Ctrl Pts',(-1.82112306513656,2.66587036417349,55.632034669634));
#20460=CARTESIAN_POINT('Ctrl Pts',(-1.65825209483043,2.77012108498177,55.6212937401246));
#20461=CARTESIAN_POINT('Ctrl Pts',(-1.31375262187064,2.94929002360706,55.599540367835));
#20462=CARTESIAN_POINT('Ctrl Pts',(-1.13267591374804,3.02345707916979,55.5885612852658));
#20463=CARTESIAN_POINT('Ctrl Pts',(-0.895906682083919,3.0961614568649,55.5739454656203));
#20464=CARTESIAN_POINT('Ctrl Pts',(-0.845438308573807,3.11032123045247,
55.5708179555036));
#20465=CARTESIAN_POINT('Ctrl Pts',(-0.760133394249979,3.13202542171231,
55.5654992995984));
#20466=CARTESIAN_POINT('Ctrl Pts',(-0.72547558018151,3.14023423417916,55.5633296399231));
#20467=CARTESIAN_POINT('Ctrl Pts',(-0.655369501236063,3.15561657494592,
55.558919855515));
#20468=CARTESIAN_POINT('Ctrl Pts',(-0.619922391875828,3.16277112843798,
55.5566794803967));
#20469=CARTESIAN_POINT('Ctrl Pts',(-0.529887102066823,3.17937191761829,
55.5509589283532));
#20470=CARTESIAN_POINT('Ctrl Pts',(-0.475163652542741,3.18800957248449,
55.5474540904453));
#20471=CARTESIAN_POINT('Ctrl Pts',(-0.16699929074674,3.22854035184702,55.5275512141267));
#20472=CARTESIAN_POINT('Ctrl Pts',(0.0892767622137504,3.23161726034424,
55.510268933566));
#20473=CARTESIAN_POINT('Ctrl Pts',(0.43467214958567,3.19462763151725,55.4868460016672));
#20474=CARTESIAN_POINT('Ctrl Pts',(0.525713846636263,3.18091373893239,55.4806717228103));
#20475=CARTESIAN_POINT('Ctrl Pts',(0.656262508258042,3.15548976322421,55.4719142417823));
#20476=CARTESIAN_POINT('Ctrl Pts',(0.696326090455761,3.14689154512072,55.4692401943707));
#20477=CARTESIAN_POINT('Ctrl Pts',(0.768362834847134,3.12998824302095,55.4644689102693));
#20478=CARTESIAN_POINT('Ctrl Pts',(0.800392813565002,3.12195121473609,55.4623607446143));
#20479=CARTESIAN_POINT('Ctrl Pts',(0.852111900807501,3.10812542289005,55.4589844560805));
#20480=CARTESIAN_POINT('Ctrl Pts',(0.87187861437407,3.10263856929728,55.4577007106795));
#20481=CARTESIAN_POINT('Ctrl Pts',(0.912060380634412,3.09107053977376,55.4551065589134));
#20482=CARTESIAN_POINT('Ctrl Pts',(0.932470028740062,3.08497502811768,55.453796966314));
#20483=CARTESIAN_POINT('Ctrl Pts',(0.988019647061457,3.0677830033401,55.450250902765));
#20484=CARTESIAN_POINT('Ctrl Pts',(1.02303313710983,3.05628513662685,55.4480358972749));
#20485=CARTESIAN_POINT('Ctrl Pts',(1.23249066356965,2.98349948840664,55.4348640724989));
#20486=CARTESIAN_POINT('Ctrl Pts',(1.40161133343692,2.90788637419721,55.4245466315709));
#20487=CARTESIAN_POINT('Ctrl Pts',(1.74279660810602,2.71862062998475,55.4026916864046));
#20488=CARTESIAN_POINT('Ctrl Pts',(1.91232651738564,2.6021595600219,55.3911777956687));
#20489=CARTESIAN_POINT('Ctrl Pts',(2.10887186918008,2.43749837051577,55.3760295996038));
#20490=CARTESIAN_POINT('Ctrl Pts',(2.14732705043697,2.40368986655771,55.3729715248353));
#20491=CARTESIAN_POINT('Ctrl Pts',(2.21098293632375,2.34497875631701,55.3677354533713));
#20492=CARTESIAN_POINT('Ctrl Pts',(2.23660864693423,2.32055004663294,55.3655773749361));
#20493=CARTESIAN_POINT('Ctrl Pts',(2.28778336730374,2.27013053808316,55.3611609429905));
#20494=CARTESIAN_POINT('Ctrl Pts',(2.31330426221159,2.24411867192428,55.3589018296224));
#20495=CARTESIAN_POINT('Ctrl Pts',(2.37751820064189,2.17640988789781,55.3530670147389));
#20496=CARTESIAN_POINT('Ctrl Pts',(2.41555701762706,2.13411256500581,55.3494646047582));
#20497=CARTESIAN_POINT('Ctrl Pts',(2.61821643490829,1.89640199489849,55.3294369328708));
#20498=CARTESIAN_POINT('Ctrl Pts',(2.76024606778113,1.68297327409865,55.3121342896196));
#20499=CARTESIAN_POINT('Ctrl Pts',(2.91623504233318,1.37470120936979,55.2888458395013));
#20500=CARTESIAN_POINT('Ctrl Pts',(2.95351678504418,1.2926602276134,55.2828064878133));
#20501=CARTESIAN_POINT('Ctrl Pts',(3.00892371422408,1.15577371167581,55.2730875351161));
#20502=CARTESIAN_POINT('Ctrl Pts',(3.0290996503226,1.10181258479639,55.2693442976301));
#20503=CARTESIAN_POINT('Ctrl Pts',(3.05597322053875,1.02360867522688,55.2640720573803));
#20504=CARTESIAN_POINT('Ctrl Pts',(3.06384979676633,0.999785757031245,55.2624860096359));
#20505=CARTESIAN_POINT('Ctrl Pts',(3.07676210538083,0.959145732012153,55.2598170805789));
#20506=CARTESIAN_POINT('Ctrl Pts',(3.08193979420671,0.942376109745944,55.258726474967));
#20507=CARTESIAN_POINT('Ctrl Pts',(3.0939773524714,0.902227920664037,55.2561408859006));
#20508=CARTESIAN_POINT('Ctrl Pts',(3.10070950966011,0.878812664418354,55.2546530341183));
#20509=CARTESIAN_POINT('Ctrl Pts',(3.12127516616435,0.80410270538572,55.2499630077144));
#20510=CARTESIAN_POINT('Ctrl Pts',(3.13410683553579,0.752538939672678,55.2468112067589));
#20511=CARTESIAN_POINT('Ctrl Pts',(3.18759408098974,0.512410811455773,55.2324271559637));
#20512=CARTESIAN_POINT('Ctrl Pts',(3.2125468570552,0.320742991126696,55.2217580674986));
#20513=CARTESIAN_POINT('Ctrl Pts',(3.22657771771426,-0.0322955815934162,
55.2019281767073));
#20514=CARTESIAN_POINT('Ctrl Pts',(3.22097258947683,-0.19280949751601,55.1928455629736));
#20515=CARTESIAN_POINT('Ctrl Pts',(3.19730343434968,-0.408074149992268,
55.1801092845613));
#20516=CARTESIAN_POINT('Ctrl Pts',(3.18970435823871,-0.463744878929698,
55.1767663020544));
#20517=CARTESIAN_POINT('Ctrl Pts',(3.1748053402836,-0.555019696872055,55.1711888647571));
#20518=CARTESIAN_POINT('Ctrl Pts',(3.16835121267288,-0.590750574196046,
55.1689809788493));
#20519=CARTESIAN_POINT('Ctrl Pts',(3.15447562094606,-0.66078151366893,55.1646017117433));
#20520=CARTESIAN_POINT('Ctrl Pts',(3.14709484965502,-0.695084531290105,
55.1624318961566));
#20521=CARTESIAN_POINT('Ctrl Pts',(3.12752203686441,-0.779337303921066,
55.1570385276832));
#20522=CARTESIAN_POINT('Ctrl Pts',(3.11469227106025,-0.829127432213722,
55.1537951924818));
#20523=CARTESIAN_POINT('Ctrl Pts',(3.02989180791858,-1.12840210429823,55.1339486834457));
#20524=CARTESIAN_POINT('Ctrl Pts',(2.929184546471,-1.36871056398113,55.1164078666076));
#20525=CARTESIAN_POINT('Ctrl Pts',(2.73194841900223,-1.71520681340992,55.0895126245274));
#20526=CARTESIAN_POINT('Ctrl Pts',(2.65535275315824,-1.83155271109945,55.0801878383818));
#20527=CARTESIAN_POINT('Ctrl Pts',(2.55212101470315,-1.96820381127954,55.0691565932237));
#20528=CARTESIAN_POINT('Ctrl Pts',(2.53239003932206,-1.99352672076478,55.0671091302164));
#20529=CARTESIAN_POINT('Ctrl Pts',(2.49954757192841,-2.03440235382374,55.0638044637458));
#20530=CARTESIAN_POINT('Ctrl Pts',(2.48666168770702,-2.05013285725691,55.0625327980774));
#20531=CARTESIAN_POINT('Ctrl Pts',(2.45981008772527,-2.08228637545829,55.0599354361305));
#20532=CARTESIAN_POINT('Ctrl Pts',(2.44582696565218,-2.09869310092674,55.0586109842135));
#20533=CARTESIAN_POINT('Ctrl Pts',(2.40667549163683,-2.14370761774219,55.0549756299731));
#20534=CARTESIAN_POINT('Ctrl Pts',(2.38116207566722,-2.17201213709358,55.0526880484139));
#20535=CARTESIAN_POINT('Ctrl Pts',(2.23561226365501,-2.32783661269814,55.0400403495102));
#20536=CARTESIAN_POINT('Ctrl Pts',(2.10582737704225,-2.44587192721079,55.0302421907769));
#20537=CARTESIAN_POINT('Ctrl Pts',(1.80158902890794,-2.68030670418677,55.0087267326335));
#20538=CARTESIAN_POINT('Ctrl Pts',(1.62410625321696,-2.7914217267226,54.9970336041673));
#20539=CARTESIAN_POINT('Ctrl Pts',(1.38973372734427,-2.90818868842021,54.9815894440076));
#20540=CARTESIAN_POINT('Ctrl Pts',(1.34176725120063,-2.93062816661406,54.978431124287));
#20541=CARTESIAN_POINT('Ctrl Pts',(1.26056152441024,-2.96620591623068,54.9730756737991));
#20542=CARTESIAN_POINT('Ctrl Pts',(1.22761646392611,-2.97999170372793,54.9709007353649));
#20543=CARTESIAN_POINT('Ctrl Pts',(1.16096893043593,-3.00658746794712,54.9664930099224));
#20544=CARTESIAN_POINT('Ctrl Pts',(1.12726707147582,-3.01938501066424,54.9642601882941));
#20545=CARTESIAN_POINT('Ctrl Pts',(1.0418162491028,-3.0502030482227,54.9585859648373));
#20546=CARTESIAN_POINT('Ctrl Pts',(0.989810825641516,-3.06747350113949,
54.9551207182374));
#20547=CARTESIAN_POINT('Ctrl Pts',(0.692133141392219,-3.15797103863363,
54.9352083142476));
#20548=CARTESIAN_POINT('Ctrl Pts',(0.438886276367857,-3.20299335167178,
54.9178667207973));
#20549=CARTESIAN_POINT('Ctrl Pts',(0.090953146238864,-3.22278640445546,
54.8943671064587));
#20550=CARTESIAN_POINT('Ctrl Pts',(-0.00131923124893615,-3.22406957593432,
54.8881781514758));
#20551=CARTESIAN_POINT('Ctrl Pts',(-0.134532326748332,-3.22020212874891,
54.8794025709591));
#20552=CARTESIAN_POINT('Ctrl Pts',(-0.175516451819975,-3.2182285451047,
54.8767247519752));
#20553=CARTESIAN_POINT('Ctrl Pts',(-0.249431867276678,-3.21325283959648,
54.8719475179539));
#20554=CARTESIAN_POINT('Ctrl Pts',(-0.282375700579359,-3.21052553760741,
54.8698371353294));
#20555=CARTESIAN_POINT('Ctrl Pts',(-0.335694192137568,-3.20528438975017,
54.8664582247901));
#20556=CARTESIAN_POINT('Ctrl Pts',(-0.356096438378675,-3.20308195494703,
54.8651740316997));
#20557=CARTESIAN_POINT('Ctrl Pts',(-0.397621854361298,-3.19819757159231,
54.8625799550361));
#20558=CARTESIAN_POINT('Ctrl Pts',(-0.41874206050948,-3.19550089837726,
54.8612708701532));
#20559=CARTESIAN_POINT('Ctrl Pts',(-0.456769780723612,-3.19026192831209,
54.8589298906642));
#20560=CARTESIAN_POINT('Ctrl Pts',(-0.473686125210811,-3.18779410613033,
54.8578942793142));
#20561=CARTESIAN_POINT('Ctrl Pts',(-0.490582094360392,-3.18519179504045,
54.8568649631546));
#20562=CARTESIAN_POINT('Origin',(-9.35406549764863E-15,0.,41.4527091182931));
#20563=CARTESIAN_POINT('',(-0.490581732222734,-3.18519185081674,53.3621044196136));
#20564=CARTESIAN_POINT('',(-0.490582106922591,-3.18519179310562,53.611790309282));
#20565=CARTESIAN_POINT('',(-0.490582094296226,-3.18519179505033,41.4527091182931));
#20566=CARTESIAN_POINT('Ctrl Pts',(-0.490581732222735,-3.18519185081674,
53.3621044196136));
#20567=CARTESIAN_POINT('Ctrl Pts',(-0.374900299471536,-3.20300905000696,
53.3687345167815));
#20568=CARTESIAN_POINT('Ctrl Pts',(-0.258278326006094,-3.21451969634228,
53.3754616507783));
#20569=CARTESIAN_POINT('Ctrl Pts',(-0.0891756247728096,-3.22193730412938,
53.3854530367755));
#20570=CARTESIAN_POINT('Ctrl Pts',(-0.0370773199011404,-3.22295781912657,
53.3885628761321));
#20571=CARTESIAN_POINT('Ctrl Pts',(0.0505799220086531,-3.22254925724566,
53.3938604005856));
#20572=CARTESIAN_POINT('Ctrl Pts',(0.0861327506792581,-3.22179500239537,
53.3960270005347));
#20573=CARTESIAN_POINT('Ctrl Pts',(0.157864795363987,-3.21908505349894,
53.4004379997426));
#20574=CARTESIAN_POINT('Ctrl Pts',(0.194037966799418,-3.21710723684919,
53.4026827748256));
#20575=CARTESIAN_POINT('Ctrl Pts',(0.285776141534282,-3.21053851694113,
53.4084305618543));
#20576=CARTESIAN_POINT('Ctrl Pts',(0.341267668412837,-3.20511487132255,
53.4119587205782));
#20577=CARTESIAN_POINT('Ctrl Pts',(0.621974377391368,-3.1703068545971,53.4300766347506));
#20578=CARTESIAN_POINT('Ctrl Pts',(0.84374348982526,-3.11861582141513,53.4453425679518));
#20579=CARTESIAN_POINT('Ctrl Pts',(1.20603461255976,-2.99267334392773,53.4712497543564));
#20580=CARTESIAN_POINT('Ctrl Pts',(1.34994018284468,-2.93057720253295,53.4818017772582));
#20581=CARTESIAN_POINT('Ctrl Pts',(1.51992444398366,-2.84203816900848,53.4941898577305));
#20582=CARTESIAN_POINT('Ctrl Pts',(1.55081028912439,-2.82530333740668,53.4964369833841));
#20583=CARTESIAN_POINT('Ctrl Pts',(1.59966518263867,-2.79778974164801,53.4999781652797));
#20584=CARTESIAN_POINT('Ctrl Pts',(1.61781259640974,-2.78733539329653,53.5012905642927));
#20585=CARTESIAN_POINT('Ctrl Pts',(1.65379236625133,-2.76613840555551,53.5038846022821));
#20586=CARTESIAN_POINT('Ctrl Pts',(1.67162508405082,-2.75539842840672,53.5051662926317));
#20587=CARTESIAN_POINT('Ctrl Pts',(1.7187467143476,-2.7263929733806,53.5085458099808));
#20588=CARTESIAN_POINT('Ctrl Pts',(1.74784918788139,-2.70782797559912,53.5106254682423));
#20589=CARTESIAN_POINT('Ctrl Pts',(1.95203358939378,-2.57291118251023,53.5252040514096));
#20590=CARTESIAN_POINT('Ctrl Pts',(2.11568044063282,-2.44012800840522,53.5368464993517));
#20591=CARTESIAN_POINT('Ctrl Pts',(2.35342340155963,-2.20519511858291,53.5555834994414));
#20592=CARTESIAN_POINT('Ctrl Pts',(2.43650073077047,-2.11304257350967,53.5625624770915));
#20593=CARTESIAN_POINT('Ctrl Pts',(2.55151311848112,-1.96964002528302,53.5731640445865));
#20594=CARTESIAN_POINT('Ctrl Pts',(2.58765620727688,-1.92190941472817,53.5766530157092));
#20595=CARTESIAN_POINT('Ctrl Pts',(2.65228519174817,-1.831430036197,53.5832212274882));
#20596=CARTESIAN_POINT('Ctrl Pts',(2.68111895828496,-1.78895316133468,53.586287033388));
#20597=CARTESIAN_POINT('Ctrl Pts',(2.72811504146043,-1.71603053916185,53.5915322092722));
#20598=CARTESIAN_POINT('Ctrl Pts',(2.74681233450099,-1.68594019340147,53.5936914869712));
#20599=CARTESIAN_POINT('Ctrl Pts',(2.78371044855742,-1.62431492661718,53.5981068330873));
#20600=CARTESIAN_POINT('Ctrl Pts',(2.80188042523399,-1.59276763937255,53.6003636018663));
#20601=CARTESIAN_POINT('Ctrl Pts',(2.8469732920476,-1.51131578268664,53.6061844720179));
#20602=CARTESIAN_POINT('Ctrl Pts',(2.87311972554678,-1.46099785088327,53.6097750314289));
#20603=CARTESIAN_POINT('Ctrl Pts',(2.99296252480382,-1.21469239530267,53.6273342301259));
#20604=CARTESIAN_POINT('Ctrl Pts',(3.06799622582896,-1.0102846682622,53.6419104095151));
#20605=CARTESIAN_POINT('Ctrl Pts',(3.16345648469369,-0.637726260737779,
53.6678897355573));
#20606=CARTESIAN_POINT('Ctrl Pts',(3.19231576705683,-0.472526182697438,
53.6791998258669));
#20607=CARTESIAN_POINT('Ctrl Pts',(3.211391719683,-0.27240994567064,53.6921704878165));
#20608=CARTESIAN_POINT('Ctrl Pts',(3.21405458684576,-0.238950357178618,
53.6943144413036));
#20609=CARTESIAN_POINT('Ctrl Pts',(3.21750898257664,-0.184874900676776,
53.6977330680708));
#20610=CARTESIAN_POINT('Ctrl Pts',(3.21862609495395,-0.16428302464723,53.6990240553682));
#20611=CARTESIAN_POINT('Ctrl Pts',(3.22048894117337,-0.122541122484632,
53.7016172094167));
#20612=CARTESIAN_POINT('Ctrl Pts',(3.22122416340241,-0.101391784046166,
53.7029188014019));
#20613=CARTESIAN_POINT('Ctrl Pts',(3.22265181082952,-0.0440668782097929,
53.7064171579824));
#20614=CARTESIAN_POINT('Ctrl Pts',(3.22294348085417,-0.00788338768629873,
53.7085934214253));
#20615=CARTESIAN_POINT('Ctrl Pts',(3.22091087406947,0.223585255126724,53.7223543320481));
#20616=CARTESIAN_POINT('Ctrl Pts',(3.20144825921741,0.418334366066101,53.7332172868747));
#20617=CARTESIAN_POINT('Ctrl Pts',(3.12782643783467,0.80017099915416,53.7550035225647));
#20618=CARTESIAN_POINT('Ctrl Pts',(3.07414827426386,0.986495907639312,53.765889717617));
#20619=CARTESIAN_POINT('Ctrl Pts',(2.98513654119631,1.21565465098643,53.7803979274953));
#20620=CARTESIAN_POINT('Ctrl Pts',(2.96500323350354,1.26396667973916,53.7835209828908));
#20621=CARTESIAN_POINT('Ctrl Pts',(2.9292128237517,1.34428315128466,53.7888342600876));
#20622=CARTESIAN_POINT('Ctrl Pts',(2.91418489856262,1.37655772798433,53.7910030962683));
#20623=CARTESIAN_POINT('Ctrl Pts',(2.88281461845869,1.44111279615364,53.7954130246769));
#20624=CARTESIAN_POINT('Ctrl Pts',(2.86645719797245,1.47338018828273,53.7976543979769));
#20625=CARTESIAN_POINT('Ctrl Pts',(2.82364600979348,1.55441908852602,53.8033813810989));
#20626=CARTESIAN_POINT('Ctrl Pts',(2.79647041606131,1.60279384209965,53.8068917680219));
#20627=CARTESIAN_POINT('Ctrl Pts',(2.6373161425683,1.86972176983358,53.826793277582));
#20628=CARTESIAN_POINT('Ctrl Pts',(2.48099472928078,2.07266014388038,53.8440672131516));
#20629=CARTESIAN_POINT('Ctrl Pts',(2.23804566940546,2.32071795622034,53.8674794253368));
#20630=CARTESIAN_POINT('Ctrl Pts',(2.17088931717789,2.38365716994643,53.8736517000749));
#20631=CARTESIAN_POINT('Ctrl Pts',(2.07006962176481,2.4703455686221,53.8824066804501));
#20632=CARTESIAN_POINT('Ctrl Pts',(2.0385023949133,2.49645824090771,53.8850801848841));
#20633=CARTESIAN_POINT('Ctrl Pts',(1.98060918254882,2.54251740934866,53.8898505961134));
#20634=CARTESIAN_POINT('Ctrl Pts',(1.95445829114228,2.56267448083339,53.8919584266217));
#20635=CARTESIAN_POINT('Ctrl Pts',(1.91156526781453,2.59469776626446,53.8953342840819));
#20636=CARTESIAN_POINT('Ctrl Pts',(1.89501194066152,2.60681186319998,53.8966179275757));
#20637=CARTESIAN_POINT('Ctrl Pts',(1.86103587841639,2.63118161225266,53.8992119728131));
#20638=CARTESIAN_POINT('Ctrl Pts',(1.84360522345807,2.64342411585323,53.9005215593472));
#20639=CARTESIAN_POINT('Ctrl Pts',(1.79568936228824,2.67637352895882,53.904067756508));
#20640=CARTESIAN_POINT('Ctrl Pts',(1.76496745901041,2.69673240764706,53.9062828977557));
#20641=CARTESIAN_POINT('Ctrl Pts',(1.57812122157672,2.81599092243489,53.9194498454236));
#20642=CARTESIAN_POINT('Ctrl Pts',(1.41405891733148,2.90184835727623,53.9297628923179));
#20643=CARTESIAN_POINT('Ctrl Pts',(1.05418868141317,3.05236355198481,53.9516129824375));
#20644=CARTESIAN_POINT('Ctrl Pts',(0.857740853359154,3.11327907632468,53.9631264156675));
#20645=CARTESIAN_POINT('Ctrl Pts',(0.606685744281197,3.16554496855344,53.9782760337901));
#20646=CARTESIAN_POINT('Ctrl Pts',(0.55628699586078,3.17478926653236,53.9813361596284));
#20647=CARTESIAN_POINT('Ctrl Pts',(0.470722120189921,3.18838391029212,53.9865745964519));
#20648=CARTESIAN_POINT('Ctrl Pts',(0.435664892260104,3.19336299559185,53.9887329422376));
#20649=CARTESIAN_POINT('Ctrl Pts',(0.364387697572853,3.20229077473168,53.9931489327869));
#20650=CARTESIAN_POINT('Ctrl Pts',(0.328168679064477,3.20620488208548,53.9954073207757));
#20651=CARTESIAN_POINT('Ctrl Pts',(0.235299020023553,3.21465102559397,54.0012380436795));
#20652=CARTESIAN_POINT('Ctrl Pts',(0.178582637278034,3.21829993001857,54.0048370150755));
#20653=CARTESIAN_POINT('Ctrl Pts',(-0.0936425913024253,3.22859589635261,
54.0223023276929));
#20654=CARTESIAN_POINT('Ctrl Pts',(-0.309331582753217,3.21510320014451,
54.0367654498928));
#20655=CARTESIAN_POINT('Ctrl Pts',(-0.689552710256647,3.15269038674251,
54.0627930308719));
#20656=CARTESIAN_POINT('Ctrl Pts',(-0.854660547309656,3.11199365571659,
54.0742648134468));
#20657=CARTESIAN_POINT('Ctrl Pts',(-1.04718040851872,3.04805246590306,54.0873464409867));
#20658=CARTESIAN_POINT('Ctrl Pts',(-1.07839609994139,3.03714877656227,54.0894573988245));
#20659=CARTESIAN_POINT('Ctrl Pts',(-1.12870615453252,3.01870188568448,54.0928369552198));
#20660=CARTESIAN_POINT('Ctrl Pts',(-1.14790539329239,3.01145345964324,54.0941212304812));
#20661=CARTESIAN_POINT('Ctrl Pts',(-1.18687701378047,2.99631334225085,54.0967151708548));
#20662=CARTESIAN_POINT('Ctrl Pts',(-1.20664286998425,2.98840822744233,54.0980240420114));
#20663=CARTESIAN_POINT('Ctrl Pts',(-1.26035268240814,2.96630784688494,54.1015659525811));
#20664=CARTESIAN_POINT('Ctrl Pts',(-1.29413517941262,2.95172585452798,54.1037776101112));
#20665=CARTESIAN_POINT('Ctrl Pts',(-1.4976881857728,2.85969678237579,54.1170481407055));
#20666=CARTESIAN_POINT('Ctrl Pts',(-1.66073633103185,2.76819541226212,54.1274549430065));
#20667=CARTESIAN_POINT('Ctrl Pts',(-1.98294952330506,2.54859882815103,54.1492968719715));
#20668=CARTESIAN_POINT('Ctrl Pts',(-2.13971016493408,2.41848595067246,54.1607072025964));
#20669=CARTESIAN_POINT('Ctrl Pts',(-2.31940654664432,2.23810359431552,54.1757474168319));
#20670=CARTESIAN_POINT('Ctrl Pts',(-2.35477126044923,2.20086489911293,54.1788141769598));
#20671=CARTESIAN_POINT('Ctrl Pts',(-2.41300560780607,2.13653378884541,54.1840604840629));
#20672=CARTESIAN_POINT('Ctrl Pts',(-2.43634587097903,2.10987946030708,54.1862199173468));
#20673=CARTESIAN_POINT('Ctrl Pts',(-2.48276663191232,2.05506992520306,54.1906351533523));
#20674=CARTESIAN_POINT('Ctrl Pts',(-2.50581888263873,2.02689765444235,54.1928916492378));
#20675=CARTESIAN_POINT('Ctrl Pts',(-2.56353242359264,1.95387599373125,54.1987108644417));
#20676=CARTESIAN_POINT('Ctrl Pts',(-2.59749553810984,1.90849316816169,54.2023000119246));
#20677=CARTESIAN_POINT('Ctrl Pts',(-2.77851758024688,1.6528162612098,54.2223819454901));
#20678=CARTESIAN_POINT('Ctrl Pts',(-2.90122981653283,1.42645928802078,54.2397617557206));
#20679=CARTESIAN_POINT('Ctrl Pts',(-3.04431400867241,1.06564356688565,54.2659236776472));
#20680=CARTESIAN_POINT('Ctrl Pts',(-3.08529931518377,0.940413963342759,
54.2747264005778));
#20681=CARTESIAN_POINT('Ctrl Pts',(-3.12653883470773,0.782230650267221,
54.2852522329607));
#20682=CARTESIAN_POINT('Ctrl Pts',(-3.13410940925886,0.751324339326221,
54.2872810868837));
#20683=CARTESIAN_POINT('Ctrl Pts',(-3.1457538571183,0.700543696118458,54.2905638374378));
#20684=CARTESIAN_POINT('Ctrl Pts',(-3.15009990823833,0.680734492413324,
54.2918318437902));
#20685=CARTESIAN_POINT('Ctrl Pts',(-3.15869655931377,0.639704535940049,
54.2944305536009));
#20686=CARTESIAN_POINT('Ctrl Pts',(-3.16292092423086,0.618479696918545,
54.2957598742098));
#20687=CARTESIAN_POINT('Ctrl Pts',(-3.17406895501523,0.559363377753016,
54.2994247886798));
#20688=CARTESIAN_POINT('Ctrl Pts',(-3.18052782925342,0.521386744293538,
54.3017364322697));
#20689=CARTESIAN_POINT('Ctrl Pts',(-3.21042212497873,0.324300025070463,
54.3135549037948));
#20690=CARTESIAN_POINT('Ctrl Pts',(-3.22260666222988,0.163699347225663,
54.3225942964115));
#20691=CARTESIAN_POINT('Ctrl Pts',(-3.22293798841606,-0.211402741709704,
54.3436183764822));
#20692=CARTESIAN_POINT('Ctrl Pts',(-3.20176299569259,-0.425117169876697,
54.3555594647547));
#20693=CARTESIAN_POINT('Ctrl Pts',(-3.14832387025797,-0.690952181915791,
54.3714961551642));
#20694=CARTESIAN_POINT('Ctrl Pts',(-3.13562869594029,-0.746451748433032,
54.3748817305995));
#20695=CARTESIAN_POINT('Ctrl Pts',(-3.11240559364864,-0.836885527360803,
54.3805105752936));
#20696=CARTESIAN_POINT('Ctrl Pts',(-3.10274228150948,-0.872029892382777,
54.3827262287743));
#20697=CARTESIAN_POINT('Ctrl Pts',(-3.0825239340578,-0.940965749010611,
54.3871316574012));
#20698=CARTESIAN_POINT('Ctrl Pts',(-3.07200403807014,-0.974762215777557,
54.3893200277684));
#20699=CARTESIAN_POINT('Ctrl Pts',(-3.04492280461057,-1.05696729886844,
54.3947160279171));
#20700=CARTESIAN_POINT('Ctrl Pts',(-3.02776170535773,-1.105166655917,54.3979427568696));
#20701=CARTESIAN_POINT('Ctrl Pts',(-2.93416920249864,-1.34946751933685,
54.4146306820711));
#20702=CARTESIAN_POINT('Ctrl Pts',(-2.83981774490436,-1.53812259221357,
54.428677858855));
#20703=CARTESIAN_POINT('Ctrl Pts',(-2.63264493851938,-1.86740695018094,
54.4549445615683));
#20704=CARTESIAN_POINT('Ctrl Pts',(-2.5251035904157,-2.01044489994952,54.4670611577171));
#20705=CARTESIAN_POINT('Ctrl Pts',(-2.38132006077559,-2.17182812616933,
54.4810660671223));
#20706=CARTESIAN_POINT('Ctrl Pts',(-2.3558970178997,-2.19937994876969,54.483469260114));
#20707=CARTESIAN_POINT('Ctrl Pts',(-2.31519314411685,-2.24197624436961,
54.4871956178509));
#20708=CARTESIAN_POINT('Ctrl Pts',(-2.3002337928999,-2.25732171682827,54.4885403541956));
#20709=CARTESIAN_POINT('Ctrl Pts',(-2.27072485665521,-2.2869943264476,54.4911430596378));
#20710=CARTESIAN_POINT('Ctrl Pts',(-2.25619025225862,-2.30133439509154,
54.4924018961524));
#20711=CARTESIAN_POINT('Ctrl Pts',(-2.21814473060734,-2.33816380012209,
54.4956406538933));
#20712=CARTESIAN_POINT('Ctrl Pts',(-2.1944270660587,-2.3604376792357,54.4976050818879));
#20713=CARTESIAN_POINT('Ctrl Pts',(-2.05529216987988,-2.48719276659433,
54.5088459730212));
#20714=CARTESIAN_POINT('Ctrl Pts',(-1.93275011846136,-2.58357144419009,
54.5176476741744));
#20715=CARTESIAN_POINT('Ctrl Pts',(-1.60915677813517,-2.80211466050229,
54.539565990347));
#20716=CARTESIAN_POINT('Ctrl Pts',(-1.40084925226597,-2.91184542007592,
54.5525842560118));
#20717=CARTESIAN_POINT('Ctrl Pts',(-1.13145026759469,-3.01810316397767,
54.5696355672569));
#20718=CARTESIAN_POINT('Ctrl Pts',(-1.07991989271876,-3.03692260685171,
54.5729027109954));
#20719=CARTESIAN_POINT('Ctrl Pts',(-0.993761133587291,-3.06591855891881,
54.5783886583007));
#20720=CARTESIAN_POINT('Ctrl Pts',(-0.959396265448393,-3.07684520973072,
54.5805827198383));
#20721=CARTESIAN_POINT('Ctrl Pts',(-0.890658133322215,-3.09743767161327,
54.5849866811192));
#20722=CARTESIAN_POINT('Ctrl Pts',(-0.856293208923901,-3.10711342220679,
54.587195895483));
#20723=CARTESIAN_POINT('Ctrl Pts',(-0.770634449312444,-3.12970244903156,
54.5927241086433));
#20724=CARTESIAN_POINT('Ctrl Pts',(-0.71917152955154,-3.14192722081825,
54.5960644315389));
#20725=CARTESIAN_POINT('Ctrl Pts',(-0.60879151596347,-3.16529357745695,
54.603273063545));
#20726=CARTESIAN_POINT('Ctrl Pts',(-0.549818244493652,-3.17606826451108,
54.6071509777578));
#20727=CARTESIAN_POINT('Ctrl Pts',(-0.490582094190866,-3.18519179506656,
54.6110712720502));
#20728=CARTESIAN_POINT('Ctrl Pts',(-0.490582094360392,-3.18519179504045,
54.8568649631546));
#20729=CARTESIAN_POINT('Ctrl Pts',(-0.510063376476227,-3.1821912949776,
54.85567814763));
#20730=CARTESIAN_POINT('Ctrl Pts',(-0.529517570778685,-3.1790119999361,
54.8544997008938));
#20731=CARTESIAN_POINT('Ctrl Pts',(-0.732390573842784,-3.14394346117165,
54.8422694795125));
#20732=CARTESIAN_POINT('Ctrl Pts',(-0.91276722127825,-3.0963927018116,54.831885054248));
#20733=CARTESIAN_POINT('Ctrl Pts',(-1.27892570161431,-2.96506151521871,
54.8100952785896));
#20734=CARTESIAN_POINT('Ctrl Pts',(-1.46289964096266,-2.87874184484615,
54.7987148588697));
#20735=CARTESIAN_POINT('Ctrl Pts',(-1.6821143513557,-2.74941589060746,54.7836861278856));
#20736=CARTESIAN_POINT('Ctrl Pts',(-1.72605068049512,-2.72204794868504,
54.7805960452093));
#20737=CARTESIAN_POINT('Ctrl Pts',(-1.79897870458099,-2.67414536361438,
54.775321967063));
#20738=CARTESIAN_POINT('Ctrl Pts',(-1.82832517116497,-2.65416742478404,
54.7731586085741));
#20739=CARTESIAN_POINT('Ctrl Pts',(-1.88352010341653,-2.6152430594055,54.769007688171));
#20740=CARTESIAN_POINT('Ctrl Pts',(-1.90942780558863,-2.59638779419708,
54.7670237600481));
#20741=CARTESIAN_POINT('Ctrl Pts',(-1.97686681233774,-2.54575131155642,
54.7617627103987));
#20742=CARTESIAN_POINT('Ctrl Pts',(-2.01791178265878,-2.51334113572709,
54.7584615388973));
#20743=CARTESIAN_POINT('Ctrl Pts',(-2.25332199710811,-2.31797047025283,
54.7389265420836));
#20744=CARTESIAN_POINT('Ctrl Pts',(-2.42866330342796,-2.13354162877199,
54.7218075171242));
#20745=CARTESIAN_POINT('Ctrl Pts',(-2.66617821405875,-1.81605233913119,
54.6950515112968));
#20746=CARTESIAN_POINT('Ctrl Pts',(-2.74410674070794,-1.69600646253892,
54.6854609395288));
#20747=CARTESIAN_POINT('Ctrl Pts',(-2.82951995409275,-1.54304005343017,
54.6741744675714));
#20748=CARTESIAN_POINT('Ctrl Pts',(-2.84480658860076,-1.51467205482868,
54.6721189459444));
#20749=CARTESIAN_POINT('Ctrl Pts',(-2.86905272395822,-1.46801513033065,
54.6688047921172));
#20750=CARTESIAN_POINT('Ctrl Pts',(-2.8782686717668,-1.44986257560209,54.6675315444779));
#20751=CARTESIAN_POINT('Ctrl Pts',(-2.89687209409043,-1.41234299582191,
54.664934744533));
#20752=CARTESIAN_POINT('Ctrl Pts',(-2.90623869747397,-1.39296710697062,
54.6636123773449));
#20753=CARTESIAN_POINT('Ctrl Pts',(-2.93157397840242,-1.33919000632293,
54.6599895853819));
#20754=CARTESIAN_POINT('Ctrl Pts',(-2.94713107045096,-1.30459748420348,
54.6577122165));
#20755=CARTESIAN_POINT('Ctrl Pts',(-3.0281355679944,-1.11562810595729,54.6455145409248));
#20756=CARTESIAN_POINT('Ctrl Pts',(-3.08207612340782,-0.956582217573359,
54.6361086581793));
#20757=CARTESIAN_POINT('Ctrl Pts',(-3.15960361010104,-0.651626454712516,
54.6184780420143));
#20758=CARTESIAN_POINT('Ctrl Pts',(-3.18602595702939,-0.506900414735007,
54.610271236269));
#20759=CARTESIAN_POINT('Ctrl Pts',(-3.20981994783154,-0.295752167679915,
54.5980734732127));
#20760=CARTESIAN_POINT('Ctrl Pts',(-3.21517049408673,-0.230415739795087,
54.5942700264858));
#20761=CARTESIAN_POINT('Ctrl Pts',(-3.2213343581676,-0.110156007277225,
54.5871800762855));
#20762=CARTESIAN_POINT('Ctrl Pts',(-3.22274295511204,-0.0552875741277878,
54.5839113801572));
#20763=CARTESIAN_POINT('Ctrl Pts',(-3.22275458631807,0.0356527003089716,
54.5784235007172));
#20764=CARTESIAN_POINT('Ctrl Pts',(-3.22215381187848,0.0717139417525594,
54.5762290953662));
#20765=CARTESIAN_POINT('Ctrl Pts',(-3.21975443429646,0.1434337548322,54.5718249619178));
#20766=CARTESIAN_POINT('Ctrl Pts',(-3.21796819882228,0.179087600705352,
54.5696159281677));
#20767=CARTESIAN_POINT('Ctrl Pts',(-3.21206791962979,0.267455490430315,
54.5640891827152));
#20768=CARTESIAN_POINT('Ctrl Pts',(-3.20724829203575,0.320110339395274,
54.5607501740726));
#20769=CARTESIAN_POINT('Ctrl Pts',(-3.19393262683197,0.434503559790764,
54.5533922080871));
#20770=CARTESIAN_POINT('Ctrl Pts',(-3.18493674747177,0.496161356330239,
54.5493597186413));
#20771=CARTESIAN_POINT('Ctrl Pts',(-3.15108149125626,0.688912539071098,
54.53654854483));
#20772=CARTESIAN_POINT('Ctrl Pts',(-3.11986814139888,0.818738439484068,
54.5276126017586));
#20773=CARTESIAN_POINT('Ctrl Pts',(-3.0245579085852,1.12904070008866,54.5057113017588));
#20774=CARTESIAN_POINT('Ctrl Pts',(-2.9522513469773,1.30648567058488,54.4927090700293));
#20775=CARTESIAN_POINT('Ctrl Pts',(-2.84789278301625,1.50895970258258,54.4779639939658));
#20776=CARTESIAN_POINT('Ctrl Pts',(-2.83060054181081,1.54115330783923,54.4756233212579));
#20777=CARTESIAN_POINT('Ctrl Pts',(-2.80239847153739,1.59158138895333,54.4719710151409));
#20778=CARTESIAN_POINT('Ctrl Pts',(-2.79184997181253,1.61001313807327,54.4706391266519));
#20779=CARTESIAN_POINT('Ctrl Pts',(-2.77073021605332,1.64608458134759,54.46804065288));
#20780=CARTESIAN_POINT('Ctrl Pts',(-2.76017092227311,1.66372981424799,54.4667735174723));
#20781=CARTESIAN_POINT('Ctrl Pts',(-2.7320883159667,1.70965425619625,54.4634828455621));
#20782=CARTESIAN_POINT('Ctrl Pts',(-2.7142942225495,1.73776618408051,54.4614757778645));
#20783=CARTESIAN_POINT('Ctrl Pts',(-2.60387768252931,1.90637211244367,54.4494506484581));
#20784=CARTESIAN_POINT('Ctrl Pts',(-2.50079314727974,2.03972547339855,54.4399849269798));
#20785=CARTESIAN_POINT('Ctrl Pts',(-2.24209595866702,2.32511494871561,54.4183922014856));
#20786=CARTESIAN_POINT('Ctrl Pts',(-2.08060457362502,2.47067376573019,54.406312723231));
#20787=CARTESIAN_POINT('Ctrl Pts',(-1.85998047245909,2.63245286301889,54.3902305071777));
#20788=CARTESIAN_POINT('Ctrl Pts',(-1.81335947187898,2.66478184606136,54.3868563247024));
#20789=CARTESIAN_POINT('Ctrl Pts',(-1.73545376162695,2.71581360477255,54.3812411922853));
#20790=CARTESIAN_POINT('Ctrl Pts',(-1.70466101112749,2.73524660051163,54.3790275759583));
#20791=CARTESIAN_POINT('Ctrl Pts',(-1.64327411118485,2.77254802506471,54.3746223128247));
#20792=CARTESIAN_POINT('Ctrl Pts',(-1.61270144054324,2.79044194733269,54.372432003279));
#20793=CARTESIAN_POINT('Ctrl Pts',(-1.53713120143195,2.83301581951627,54.367023890353));
#20794=CARTESIAN_POINT('Ctrl Pts',(-1.49182838723517,2.85713117437827,54.3637867882773));
#20795=CARTESIAN_POINT('Ctrl Pts',(-1.39249728128651,2.90700001102965,54.3566958924982));
#20796=CARTESIAN_POINT('Ctrl Pts',(-1.33828899831606,2.93235052330283,54.3528302732313));
#20797=CARTESIAN_POINT('Ctrl Pts',(-1.16978381634417,3.00550620152427,54.3408297034384));
#20798=CARTESIAN_POINT('Ctrl Pts',(-1.05341778478968,3.04824018565404,54.3325592847735));
#20799=CARTESIAN_POINT('Ctrl Pts',(-0.733490013640261,3.14521843162858,
54.3100382282056));
#20800=CARTESIAN_POINT('Ctrl Pts',(-0.526584642731852,3.18639690430633,
54.295677508164));
#20801=CARTESIAN_POINT('Ctrl Pts',(-0.282808764264148,3.21050251867335,
54.2798550563176));
#20802=CARTESIAN_POINT('Ctrl Pts',(-0.248430864767838,3.2133455378287,54.2776497292495));
#20803=CARTESIAN_POINT('Ctrl Pts',(-0.193246948454593,3.21701823022155,
54.2741582163811));
#20804=CARTESIAN_POINT('Ctrl Pts',(-0.172467866053886,3.21819911937743,
54.2728545185015));
#20805=CARTESIAN_POINT('Ctrl Pts',(-0.130752558560434,3.22016462015822,
54.2702612849897));
#20806=CARTESIAN_POINT('Ctrl Pts',(-0.109817238493129,3.220946544569,54.2689719399885));
#20807=CARTESIAN_POINT('Ctrl Pts',(-0.0537350537837422,3.22249373470219,
54.2655468686595));
#20808=CARTESIAN_POINT('Ctrl Pts',(-0.0185798613695318,3.222888198736,54.2634301934472));
#20809=CARTESIAN_POINT('Ctrl Pts',(0.176678525717378,3.22188386711047,54.251807808747));
#20810=CARTESIAN_POINT('Ctrl Pts',(0.336514746736353,3.20913067856127,54.2427872893362));
#20811=CARTESIAN_POINT('Ctrl Pts',(0.714580976968956,3.1503938644972,54.2213319423596));
#20812=CARTESIAN_POINT('Ctrl Pts',(0.93025994907462,3.09357628651168,54.2089587673856));
#20813=CARTESIAN_POINT('Ctrl Pts',(1.190965635434,2.99514273180092,54.1925705505967));
#20814=CARTESIAN_POINT('Ctrl Pts',(1.24303754449917,2.97390925094386,54.1892248412624));
#20815=CARTESIAN_POINT('Ctrl Pts',(1.32778326022004,2.9367376590655,54.1836441112269));
#20816=CARTESIAN_POINT('Ctrl Pts',(1.36079125085731,2.92158920297177,54.1814357259609));
#20817=CARTESIAN_POINT('Ctrl Pts',(1.42553752027605,2.89053974481266,54.1770311466058));
#20818=CARTESIAN_POINT('Ctrl Pts',(1.4572830684078,2.87466574363278,54.1748361207666));
#20819=CARTESIAN_POINT('Ctrl Pts',(1.53462280660184,2.83438257077156,54.1693978451491));
#20820=CARTESIAN_POINT('Ctrl Pts',(1.57990272702172,2.80939470326312,54.1661347926162));
#20821=CARTESIAN_POINT('Ctrl Pts',(1.79681482676243,2.68278852473457,54.1501055281509));
#20822=CARTESIAN_POINT('Ctrl Pts',(1.95933933349941,2.56648888628889,54.1368217239276));
#20823=CARTESIAN_POINT('Ctrl Pts',(2.25363033317695,2.3115687177846,54.1105503290812));
#20824=CARTESIAN_POINT('Ctrl Pts',(2.38593947859964,2.17474176621434,54.0976376248897));
#20825=CARTESIAN_POINT('Ctrl Pts',(2.52846936786938,1.99857493131814,54.0829677141026));
#20826=CARTESIAN_POINT('Ctrl Pts',(2.5510211094432,1.96970826753548,54.080621244722));
#20827=CARTESIAN_POINT('Ctrl Pts',(2.58587396159763,1.92349295118756,54.0769620639383));
#20828=CARTESIAN_POINT('Ctrl Pts',(2.59850329941778,1.90639710987125,54.0756289767073));
#20829=CARTESIAN_POINT('Ctrl Pts',(2.62300842312808,1.87252946796888,54.0730301452369));
#20830=CARTESIAN_POINT('Ctrl Pts',(2.63489460036788,1.8557667623581,54.0717638209651));
#20831=CARTESIAN_POINT('Ctrl Pts',(2.66556131925622,1.81162975712169,54.06847818322));
#20832=CARTESIAN_POINT('Ctrl Pts',(2.68408123997484,1.78407612360554,54.0664752433602));
#20833=CARTESIAN_POINT('Ctrl Pts',(2.72465926842631,1.7216422616976,54.0620320504714));
#20834=CARTESIAN_POINT('Ctrl Pts',(2.74648006607318,1.68661428479832,54.0596041790711));
#20835=CARTESIAN_POINT('Ctrl Pts',(2.81534292059383,1.57118958959713,54.0517806066921));
#20836=CARTESIAN_POINT('Ctrl Pts',(2.85957570286652,1.48916796449042,54.0464936342767));
#20837=CARTESIAN_POINT('Ctrl Pts',(3.0150776071079,1.16825951496468,54.0264157559186));
#20838=CARTESIAN_POINT('Ctrl Pts',(3.10044766980587,0.918008038861733,54.0119069145922));
#20839=CARTESIAN_POINT('Ctrl Pts',(3.16482492677151,0.610397900768834,53.9933333454291));
#20840=CARTESIAN_POINT('Ctrl Pts',(3.17405999750145,0.560397291396893,53.9902957253355));
#20841=CARTESIAN_POINT('Ctrl Pts',(3.1876475546923,0.475652127818242,53.9851051169721));
#20842=CARTESIAN_POINT('Ctrl Pts',(3.19262373802499,0.441016324498363,53.982971934843));
#20843=CARTESIAN_POINT('Ctrl Pts',(3.20162986433332,0.370151504111411,53.9785803447379));
#20844=CARTESIAN_POINT('Ctrl Pts',(3.20561104523082,0.333921515288071,53.9763207450685));
#20845=CARTESIAN_POINT('Ctrl Pts',(3.2142333548562,0.240958714274003,53.9704829742739));
#20846=CARTESIAN_POINT('Ctrl Pts',(3.21798729779291,0.184158253721435,53.9668780410474));
#20847=CARTESIAN_POINT('Ctrl Pts',(3.22678929045453,-0.0385166270848243,
53.9525897409715));
#20848=CARTESIAN_POINT('Ctrl Pts',(3.22052704324914,-0.204561837013675,
53.9415797016312));
#20849=CARTESIAN_POINT('Ctrl Pts',(3.17802142478831,-0.572981673708231,
53.9166144875728));
#20850=CARTESIAN_POINT('Ctrl Pts',(3.13515840014403,-0.773897507745744,
53.9026232342128));
#20851=CARTESIAN_POINT('Ctrl Pts',(3.06118143319533,-1.0084458949903,53.8866352535821));
#20852=CARTESIAN_POINT('Ctrl Pts',(3.04811822815049,-1.04726811696155,53.8840020891666));
#20853=CARTESIAN_POINT('Ctrl Pts',(3.02686170489738,-1.1066686551059,53.8800045119826));
#20854=CARTESIAN_POINT('Ctrl Pts',(3.01919088395622,-1.12742794218081,53.8786134254569));
#20855=CARTESIAN_POINT('Ctrl Pts',(3.00417328280183,-1.16681677203176,53.875987631624));
#20856=CARTESIAN_POINT('Ctrl Pts',(2.99686578374266,-1.18545939741121,53.8747509878917));
#20857=CARTESIAN_POINT('Ctrl Pts',(2.97802938070205,-1.232226598959,53.8716617481628));
#20858=CARTESIAN_POINT('Ctrl Pts',(2.96627514318384,-1.26025922380229,53.869821878414));
#20859=CARTESIAN_POINT('Ctrl Pts',(2.91177562314392,-1.38524611512165,53.8616540342483));
#20860=CARTESIAN_POINT('Ctrl Pts',(2.86465758822717,-1.48023143880938,53.8555423653064));
#20861=CARTESIAN_POINT('Ctrl Pts',(2.73985303670194,-1.70345333290227,53.8410199769803));
#20862=CARTESIAN_POINT('Ctrl Pts',(2.65774039708992,-1.82892479893098,53.8327152062218));
#20863=CARTESIAN_POINT('Ctrl Pts',(2.47627652318094,-2.06804080338671,53.8158098874259));
#20864=CARTESIAN_POINT('Ctrl Pts',(2.37708883478255,-2.18132532006941,53.8072274375089));
#20865=CARTESIAN_POINT('Ctrl Pts',(2.23515041867828,-2.32221477967414,53.7953934931294));
#20866=CARTESIAN_POINT('Ctrl Pts',(2.19913899695723,-2.35634593270274,53.7924263078995));
#20867=CARTESIAN_POINT('Ctrl Pts',(2.13656047167297,-2.41297267527477,53.7873185264838));
#20868=CARTESIAN_POINT('Ctrl Pts',(2.11039000659383,-2.43589442598669,53.785196182592));
#20869=CARTESIAN_POINT('Ctrl Pts',(2.05579745515643,-2.48216985387171,53.7807936536765));
#20870=CARTESIAN_POINT('Ctrl Pts',(2.02733641945124,-2.50546946201431,53.7785117220236));
#20871=CARTESIAN_POINT('Ctrl Pts',(1.95245301836596,-2.56466128010022,53.7725385313103));
#20872=CARTESIAN_POINT('Ctrl Pts',(1.9054397749277,-2.59978053377707,53.7688180155848));
#20873=CARTESIAN_POINT('Ctrl Pts',(1.7988001282533,-2.67499435617886,53.7604390202086));
#20874=CARTESIAN_POINT('Ctrl Pts',(1.73873974725404,-2.71441699719679,53.7557594517152));
#20875=CARTESIAN_POINT('Ctrl Pts',(1.525752251308,-2.84424795313825,53.7393137406151));
#20876=CARTESIAN_POINT('Ctrl Pts',(1.36671391899218,-2.9239956993436,53.7272704164231));
#20877=CARTESIAN_POINT('Ctrl Pts',(1.0774644457586,-3.04026035364349,53.7062516519805));
#20878=CARTESIAN_POINT('Ctrl Pts',(0.949983053072209,-3.08247487547531,
53.6972733566348));
#20879=CARTESIAN_POINT('Ctrl Pts',(0.789234370850497,-3.12478063720933,
53.6865672561343));
#20880=CARTESIAN_POINT('Ctrl Pts',(0.758116053302502,-3.13247588227786,
53.6845228700491));
#20881=CARTESIAN_POINT('Ctrl Pts',(0.709037547476687,-3.14383825763317,
53.681348053055));
#20882=CARTESIAN_POINT('Ctrl Pts',(0.691152879655012,-3.14781844613387,
53.6802013761708));
#20883=CARTESIAN_POINT('Ctrl Pts',(0.652802752370202,-3.15601055827438,
53.677765888194));
#20884=CARTESIAN_POINT('Ctrl Pts',(0.632328161527379,-3.16017645544471,
53.6764797611073));
#20885=CARTESIAN_POINT('Ctrl Pts',(0.577563562966301,-3.17076565425228,
53.673073883215));
#20886=CARTESIAN_POINT('Ctrl Pts',(0.543206429755999,-3.17683199116043,
53.6709728108066));
#20887=CARTESIAN_POINT('Ctrl Pts',(0.465206083339248,-3.18930179407254,
53.6662695297599));
#20888=CARTESIAN_POINT('Ctrl Pts',(0.421515837015358,-3.1953696779379,53.6636820495336));
#20889=CARTESIAN_POINT('Ctrl Pts',(0.273960462157292,-3.21278348609836,
53.6550605280975));
#20890=CARTESIAN_POINT('Ctrl Pts',(0.169667920374966,-3.2199762880829,53.6491601595463));
#20891=CARTESIAN_POINT('Ctrl Pts',(-0.120882067791962,-3.225856123177,53.6328426080335));
#20892=CARTESIAN_POINT('Ctrl Pts',(-0.306834800524082,-3.21349248787365,
53.6225167194536));
#20893=CARTESIAN_POINT('Ctrl Pts',(-0.490582106922524,-3.18519179310563,
53.611790309282));
#20894=CARTESIAN_POINT('Origin',(-9.35406549764863E-15,0.,41.4527091182931));
#20895=CARTESIAN_POINT('',(-0.49058209429419,-3.18519179505064,52.1162187418821));
#20896=CARTESIAN_POINT('',(-0.490582094296231,-3.18519179505033,52.3599056026743));
#20897=CARTESIAN_POINT('',(-0.490582094296226,-3.18519179505033,41.4527091182931));
#20898=CARTESIAN_POINT('',(-3.2227494359304,-0.00190675388112439,53.0831681868229));
#20899=CARTESIAN_POINT('Ctrl Pts',(-0.49058209429419,-3.18519179505064,
52.1162187418821));
#20900=CARTESIAN_POINT('Ctrl Pts',(-0.471422613079779,-3.18814273145403,
52.1174424045019));
#20901=CARTESIAN_POINT('Ctrl Pts',(-0.452236283182814,-3.19092083075083,
52.1186572587537));
#20902=CARTESIAN_POINT('Ctrl Pts',(-0.412634041374947,-3.19629068845668,
52.1211415364045));
#20903=CARTESIAN_POINT('Ctrl Pts',(-0.392216192911372,-3.19886034581764,
52.1224095510059));
#20904=CARTESIAN_POINT('Ctrl Pts',(-0.338644886686095,-3.20508183815937,
52.1257061957732));
#20905=CARTESIAN_POINT('Ctrl Pts',(-0.305455898587567,-3.20841500418907,
52.1277182390375));
#20906=CARTESIAN_POINT('Ctrl Pts',(-0.13201741738564,-3.22311757488889,
52.1381023948326));
#20907=CARTESIAN_POINT('Ctrl Pts',(0.00882799816034327,-3.22580931540793,
52.1460950759228));
#20908=CARTESIAN_POINT('Ctrl Pts',(0.402765974297692,-3.20752618248547,
52.1682731323922));
#20909=CARTESIAN_POINT('Ctrl Pts',(0.653824315681166,-3.16590415144211,
52.1822739342074));
#20910=CARTESIAN_POINT('Ctrl Pts',(0.947622086190241,-3.0807245706664,52.2003271277172));
#20911=CARTESIAN_POINT('Ctrl Pts',(0.997477051463299,-3.06494544381852,
52.2034474847888));
#20912=CARTESIAN_POINT('Ctrl Pts',(1.077224405187,-3.03755354990032,52.2085427635738));
#20913=CARTESIAN_POINT('Ctrl Pts',(1.10736691258954,-3.02669496231513,52.2104930201567));
#20914=CARTESIAN_POINT('Ctrl Pts',(1.17055289575816,-3.00286253064938,52.2146354414854));
#20915=CARTESIAN_POINT('Ctrl Pts',(1.20355375699964,-2.98978856354878,52.2168307065457));
#20916=CARTESIAN_POINT('Ctrl Pts',(1.2841205626578,-2.95632033169812,52.222271591795));
#20917=CARTESIAN_POINT('Ctrl Pts',(1.33142273408795,-2.935320857193,52.2255370668947));
#20918=CARTESIAN_POINT('Ctrl Pts',(1.56582986623484,-2.82442563199419,52.2420876233332));
#20919=CARTESIAN_POINT('Ctrl Pts',(1.74442046309859,-2.71775202842572,52.2559387553089));
#20920=CARTESIAN_POINT('Ctrl Pts',(2.05706302484094,-2.48742871141326,52.2821553253392));
#20921=CARTESIAN_POINT('Ctrl Pts',(2.19336162851785,-2.36811815089191,52.2944240922266));
#20922=CARTESIAN_POINT('Ctrl Pts',(2.34474162724589,-2.21126315177056,52.3085439493399));
#20923=CARTESIAN_POINT('Ctrl Pts',(2.37008017867017,-2.18408292919107,52.3109253266136));
#20924=CARTESIAN_POINT('Ctrl Pts',(2.40923730992446,-2.14059557481503,52.3146257739316));
#20925=CARTESIAN_POINT('Ctrl Pts',(2.42337272024541,-2.1245796170276,52.3159659556855));
#20926=CARTESIAN_POINT('Ctrl Pts',(2.45073704128388,-2.09294632683357,52.3185669320059));
#20927=CARTESIAN_POINT('Ctrl Pts',(2.46397827663471,-2.07734143938101,52.3198284849702));
#20928=CARTESIAN_POINT('Ctrl Pts',(2.49803778177659,-2.03641821003639,52.3230844289045));
#20929=CARTESIAN_POINT('Ctrl Pts',(2.51862068831802,-2.01090574148968,52.3250630046848));
#20930=CARTESIAN_POINT('Ctrl Pts',(2.6501908580659,-1.84263471737163,52.3378158705556));
#20931=CARTESIAN_POINT('Ctrl Pts',(2.74939748059288,-1.69104813762514,52.3479452698348));
#20932=CARTESIAN_POINT('Ctrl Pts',(2.93224542058372,-1.35262257976696,52.3694955054425));
#20933=CARTESIAN_POINT('Ctrl Pts',(3.01188534193679,-1.16455477356078,52.3808856889092));
#20934=CARTESIAN_POINT('Ctrl Pts',(3.09053479669109,-0.915431611605484,
52.3962329416021));
#20935=CARTESIAN_POINT('Ctrl Pts',(3.10636674075913,-0.860177565033137,
52.3996495968494));
#20936=CARTESIAN_POINT('Ctrl Pts',(3.12983707905995,-0.769138102149606,
52.405316108137));
#20937=CARTESIAN_POINT('Ctrl Pts',(3.13835870373939,-0.733592557472927,
52.4075375783617));
#20938=CARTESIAN_POINT('Ctrl Pts',(3.15392395705122,-0.663422353162895,
52.4119443270527));
#20939=CARTESIAN_POINT('Ctrl Pts',(3.16100639590858,-0.628811540833945,
52.4141280218646));
#20940=CARTESIAN_POINT('Ctrl Pts',(3.17687476915188,-0.544206240445368,
52.4194934457681));
#20941=CARTESIAN_POINT('Ctrl Pts',(3.18505103432578,-0.49410846541297,52.4226937637584));
#20942=CARTESIAN_POINT('Ctrl Pts',(3.21781154853035,-0.258499391474556,
52.4378614871394));
#20943=CARTESIAN_POINT('Ctrl Pts',(3.22738777920457,-0.0712925020199418,
52.4502801860719));
#20944=CARTESIAN_POINT('Ctrl Pts',(3.21321698339483,0.323302485876479,52.47688623264));
#20945=CARTESIAN_POINT('Ctrl Pts',(3.18569725825432,0.529746007867061,52.4910573598766));
#20946=CARTESIAN_POINT('Ctrl Pts',(3.13058648240641,0.766000504741335,52.5067321295767));
#20947=CARTESIAN_POINT('Ctrl Pts',(3.12213257273492,0.799760539931585,52.5089577330203));
#20948=CARTESIAN_POINT('Ctrl Pts',(3.10773492918348,0.853543759116961,52.5124733704233));
#20949=CARTESIAN_POINT('Ctrl Pts',(3.10214076886668,0.873656709152015,52.5137813150147));
#20950=CARTESIAN_POINT('Ctrl Pts',(3.09056019092132,0.913778624694611,52.51637488935));
#20951=CARTESIAN_POINT('Ctrl Pts',(3.08457392492454,0.933786606366464,52.5176604499905));
#20952=CARTESIAN_POINT('Ctrl Pts',(3.06808307899381,0.987014471805906,52.521063070057));
#20953=CARTESIAN_POINT('Ctrl Pts',(3.05723332281614,1.02012547178175,52.5231615135305));
#20954=CARTESIAN_POINT('Ctrl Pts',(3.03146237010262,1.09466514434225,52.5278578000113));
#20955=CARTESIAN_POINT('Ctrl Pts',(3.01622467845812,1.13597751431622,52.5304409803315));
#20956=CARTESIAN_POINT('Ctrl Pts',(2.96210634630069,1.27392776981211,52.5390403781021));
#20957=CARTESIAN_POINT('Ctrl Pts',(2.91938771394712,1.36899370582799,52.544923645375));
#20958=CARTESIAN_POINT('Ctrl Pts',(2.76378258770588,1.6747199972565,52.5641867635012));
#20959=CARTESIAN_POINT('Ctrl Pts',(2.632104793227,1.87488557525754,52.5774201669147));
#20960=CARTESIAN_POINT('Ctrl Pts',(2.44481861772149,2.10045974902195,52.5946910408471));
#20961=CARTESIAN_POINT('Ctrl Pts',(2.40906382022346,2.14137344544636,52.5979282411802));
#20962=CARTESIAN_POINT('Ctrl Pts',(2.34795212277716,2.20783415511511,52.6033781806802));
#20963=CARTESIAN_POINT('Ctrl Pts',(2.32317016978486,2.23389593065752,52.6055668877421));
#20964=CARTESIAN_POINT('Ctrl Pts',(2.2728662028248,2.28505526857974,52.6099713048634));
#20965=CARTESIAN_POINT('Ctrl Pts',(2.24735188199573,2.31015317928954,52.6121865212443));
#20966=CARTESIAN_POINT('Ctrl Pts',(2.18275376129814,2.37161398172644,52.617752212039));
#20967=CARTESIAN_POINT('Ctrl Pts',(2.14317564630202,2.40743940139083,52.6211246512535));
#20968=CARTESIAN_POINT('Ctrl Pts',(1.96265710835377,2.5628613358724,52.6363508871203));
#20969=CARTESIAN_POINT('Ctrl Pts',(1.81249063149865,2.67116852599916,52.6486355464533));
#20970=CARTESIAN_POINT('Ctrl Pts',(1.47933785067283,2.87037288540808,52.6748013366586));
#20971=CARTESIAN_POINT('Ctrl Pts',(1.29528497271156,2.95799385834272,52.6886617018734));
#20972=CARTESIAN_POINT('Ctrl Pts',(1.07102348504934,3.03978169568756,52.7040938779604));
#20973=CARTESIAN_POINT('Ctrl Pts',(1.03765650706262,3.05133303185523,52.7063530076903));
#20974=CARTESIAN_POINT('Ctrl Pts',(0.98416949440476,3.0688708211572,52.7099084523376));
#20975=CARTESIAN_POINT('Ctrl Pts',(0.964170067072682,3.0752128136938,52.7112233520003));
#20976=CARTESIAN_POINT('Ctrl Pts',(0.924241120709941,3.08744679691797,52.7138177524495));
#20977=CARTESIAN_POINT('Ctrl Pts',(0.904313770302774,3.0933422098082,52.715097370741));
#20978=CARTESIAN_POINT('Ctrl Pts',(0.851306376083945,3.10846817490518,52.7184644764938));
#20979=CARTESIAN_POINT('Ctrl Pts',(0.818132509615256,3.11736368583707,52.7205340342382));
#20980=CARTESIAN_POINT('Ctrl Pts',(0.742937299594117,3.1362440271104,52.7251534290824));
#20981=CARTESIAN_POINT('Ctrl Pts',(0.700844261146414,3.1459180025066,52.7276893167787));
#20982=CARTESIAN_POINT('Ctrl Pts',(0.559986181482525,3.17532279752959,52.7360472467679));
#20983=CARTESIAN_POINT('Ctrl Pts',(0.460488449175386,3.19127122764661,52.7417441007411));
#20984=CARTESIAN_POINT('Ctrl Pts',(0.115720369404362,3.23007025084176,52.7612400745245));
#20985=CARTESIAN_POINT('Ctrl Pts',(-0.131288548408443,3.22947345281254,
52.7748564860493));
#20986=CARTESIAN_POINT('Ctrl Pts',(-0.428791399848154,3.1945423148272,52.7925177033988));
#20987=CARTESIAN_POINT('Ctrl Pts',(-0.481601971918925,3.18700827166916,
52.7956982944682));
#20988=CARTESIAN_POINT('Ctrl Pts',(-0.565963785330671,3.17282839992237,
52.8008646722894));
#20989=CARTESIAN_POINT('Ctrl Pts',(-0.597645678632529,3.16701351262686,
52.8028243833263));
#20990=CARTESIAN_POINT('Ctrl Pts',(-0.663881736657569,3.15382729840659,
52.8069650742735));
#20991=CARTESIAN_POINT('Ctrl Pts',(-0.698412332702053,3.14636069853373,
52.8091488228204));
#20992=CARTESIAN_POINT('Ctrl Pts',(-0.782249639706248,3.12678435270964,
52.8145150367139));
#20993=CARTESIAN_POINT('Ctrl Pts',(-0.831405055510819,3.11407451040364,
52.8177161076703));
#20994=CARTESIAN_POINT('Ctrl Pts',(-1.06065445156192,3.04898408726272,52.8329117769836));
#20995=CARTESIAN_POINT('Ctrl Pts',(-1.23622932652036,2.98211504929666,52.8453599631252));
#20996=CARTESIAN_POINT('Ctrl Pts',(-1.59146554086719,2.81003490002589,52.8719588807387));
#20997=CARTESIAN_POINT('Ctrl Pts',(-1.76882088892803,2.70191438283583,52.8860910360824));
#20998=CARTESIAN_POINT('Ctrl Pts',(-1.96245645060557,2.5565792913504,52.9017354665703));
#20999=CARTESIAN_POINT('Ctrl Pts',(-1.98999928313984,2.53519941496186,52.9039653412491));
#21000=CARTESIAN_POINT('Ctrl Pts',(-2.03348107111656,2.50030170086807,52.9074860028827));
#21001=CARTESIAN_POINT('Ctrl Pts',(-2.04964418822886,2.48706908228006,52.9087947874549));
#21002=CARTESIAN_POINT('Ctrl Pts',(-2.0816962826965,2.46030357032108,52.9113883518853));
#21003=CARTESIAN_POINT('Ctrl Pts',(-2.09758475026516,2.4467716162721,52.9126730873425));
#21004=CARTESIAN_POINT('Ctrl Pts',(-2.13959235093509,2.41028445697734,52.916070820585));
#21005=CARTESIAN_POINT('Ctrl Pts',(-2.16547402154489,2.387058665748,52.9181652967321));
#21006=CARTESIAN_POINT('Ctrl Pts',(-2.22317772161475,2.3335651908511,52.9228510067565));
#21007=CARTESIAN_POINT('Ctrl Pts',(-2.25476754614464,2.3030565205436,52.9254276769711));
#21008=CARTESIAN_POINT('Ctrl Pts',(-2.35881271992539,2.198378676343,52.9339935554121));
#21009=CARTESIAN_POINT('Ctrl Pts',(-2.42831349264826,2.12135858208016,52.9398509016356));
#21010=CARTESIAN_POINT('Ctrl Pts',(-2.64591400805072,1.85547876684069,52.9591453033921));
#21011=CARTESIAN_POINT('Ctrl Pts',(-2.77662998547973,1.653474713881,52.9724311691208));
#21012=CARTESIAN_POINT('Ctrl Pts',(-2.90791878081266,1.39034650197362,52.9897555740468));
#21013=CARTESIAN_POINT('Ctrl Pts',(-2.93088808779307,1.34124924735414,52.9929852924918));
#21014=CARTESIAN_POINT('Ctrl Pts',(-2.96701069260175,1.25867257769772,52.9984262533494));
#21015=CARTESIAN_POINT('Ctrl Pts',(-2.98086155545157,1.22550941849734,53.0006136401906));
#21016=CARTESIAN_POINT('Ctrl Pts',(-3.00740145346462,1.15885137667292,53.0050182579616));
#21017=CARTESIAN_POINT('Ctrl Pts',(-3.02009244678333,1.12536281481107,53.0072350439398));
#21018=CARTESIAN_POINT('Ctrl Pts',(-3.05034677819123,1.04132844856807,53.0128104553458));
#21019=CARTESIAN_POINT('Ctrl Pts',(-3.06721374790806,0.990545146567159,
53.0161912120146));
#21020=CARTESIAN_POINT('Ctrl Pts',(-3.10126486782354,0.878796517847917,
53.0236592817187));
#21021=CARTESIAN_POINT('Ctrl Pts',(-3.11793146420971,0.81769777873726,53.0277608628059));
#21022=CARTESIAN_POINT('Ctrl Pts',(-3.19270799141907,0.507893286975151,
53.0486411883242));
#21023=CARTESIAN_POINT('Ctrl Pts',(-3.22290049581669,0.253411023710327,
53.0661558434012));
#21024=CARTESIAN_POINT('Ctrl Pts',(-3.2227494359304,-0.00190675388112439,
53.0831681868229));
#21025=CARTESIAN_POINT('Ctrl Pts',(-3.22274943328784,-0.00191121505285077,
53.0831684840798));
#21026=CARTESIAN_POINT('Ctrl Pts',(-3.22271772432663,-0.0553798378646609,
53.0867312056951));
#21027=CARTESIAN_POINT('Ctrl Pts',(-3.22135536909969,-0.108842478347912,
53.0902648959406));
#21028=CARTESIAN_POINT('Ctrl Pts',(-3.21686196289615,-0.197981605506103,
53.096084777586));
#21029=CARTESIAN_POINT('Ctrl Pts',(-3.2144657519642,-0.233683025948998,
53.0983963781368));
#21030=CARTESIAN_POINT('Ctrl Pts',(-3.20975897216,-0.289804597775859,53.1019922981067));
#21031=CARTESIAN_POINT('Ctrl Pts',(-3.20784689275809,-0.310254293233996,
53.1032946496888));
#21032=CARTESIAN_POINT('Ctrl Pts',(-3.20385690258654,-0.34893422260551,
53.105741222731));
#21033=CARTESIAN_POINT('Ctrl Pts',(-3.20181853808203,-0.367167883617922,
53.1068874336563));
#21034=CARTESIAN_POINT('Ctrl Pts',(-3.19703678975587,-0.406868017816232,
53.109366269031));
#21035=CARTESIAN_POINT('Ctrl Pts',(-3.19423271797125,-0.428326071733101,
53.1106955519831));
#21036=CARTESIAN_POINT('Ctrl Pts',(-3.18583780188757,-0.487891757877464,
53.1143602343152));
#21037=CARTESIAN_POINT('Ctrl Pts',(-3.17977950586519,-0.525931033073054,
53.1166716884514));
#21038=CARTESIAN_POINT('Ctrl Pts',(-3.14112999498181,-0.743427724020373,
53.1297686303432));
#21039=CARTESIAN_POINT('Ctrl Pts',(-3.09402954915463,-0.919987902043252,
53.1399460253711));
#21040=CARTESIAN_POINT('Ctrl Pts',(-2.96298774501041,-1.28398497584804,
53.1616162624548));
#21041=CARTESIAN_POINT('Ctrl Pts',(-2.87560000956937,-1.46929486605143,
53.1730872064711));
#21042=CARTESIAN_POINT('Ctrl Pts',(-2.74504509641757,-1.6892251166233,53.1881952150955));
#21043=CARTESIAN_POINT('Ctrl Pts',(-2.71778441415138,-1.73274392798073,
53.1912617793187));
#21044=CARTESIAN_POINT('Ctrl Pts',(-2.66997802716068,-1.80515649886275,
53.1965078529293));
#21045=CARTESIAN_POINT('Ctrl Pts',(-2.64997365764608,-1.83439693375694,
53.1986672529939));
#21046=CARTESIAN_POINT('Ctrl Pts',(-2.60844584599184,-1.89300102278889,
53.2030825077528));
#21047=CARTESIAN_POINT('Ctrl Pts',(-2.58689880660851,-1.92234153996346,
53.2053390570679));
#21048=CARTESIAN_POINT('Ctrl Pts',(-2.53054050729678,-1.99642057506568,
53.2111586017881));
#21049=CARTESIAN_POINT('Ctrl Pts',(-2.4950386409874,-2.04061557113202,53.2147480313735));
#21050=CARTESIAN_POINT('Ctrl Pts',(-2.31779890900502,-2.2497116196632,53.2323194259474));
#21051=CARTESIAN_POINT('Ctrl Pts',(-2.16080106458157,-2.40089702043185,
53.2469103446982));
#21052=CARTESIAN_POINT('Ctrl Pts',(-1.85752879741484,-2.63893599177738,
53.2729532070226));
#21053=CARTESIAN_POINT('Ctrl Pts',(-1.71731185694977,-2.73226020121365,
53.2843121299865));
#21054=CARTESIAN_POINT('Ctrl Pts',(-1.5415397390561,-2.83034772081998,53.2972929166255));
#21055=CARTESIAN_POINT('Ctrl Pts',(-1.51239002097139,-2.84603050042357,
53.2994062133198));
#21056=CARTESIAN_POINT('Ctrl Pts',(-1.46477749536448,-2.87070824632975,
53.3027885350636));
#21057=CARTESIAN_POINT('Ctrl Pts',(-1.44646178158218,-2.87998043990741,
53.3040732818903));
#21058=CARTESIAN_POINT('Ctrl Pts',(-1.40898335572586,-2.89850585647834,
53.3066671423694));
#21059=CARTESIAN_POINT('Ctrl Pts',(-1.38981528382808,-2.90774548959518,
53.3079754779408));
#21060=CARTESIAN_POINT('Ctrl Pts',(-1.33729906453871,-2.9324220430405,53.3115141862648));
#21061=CARTESIAN_POINT('Ctrl Pts',(-1.30377521447105,-2.94747998672584,
53.3137232423185));
#21062=CARTESIAN_POINT('Ctrl Pts',(-1.09744848097736,-3.03594664262729,
53.3270599832969));
#21063=CARTESIAN_POINT('Ctrl Pts',(-0.91874247139775,-3.09472019893946,
53.3375269287872));
#21064=CARTESIAN_POINT('Ctrl Pts',(-0.654739885777959,-3.15664153724001,
53.3527166130787));
#21065=CARTESIAN_POINT('Ctrl Pts',(-0.572898969281294,-3.17251338916061,
53.3573865382102));
#21066=CARTESIAN_POINT('Ctrl Pts',(-0.490581732222734,-3.18519185081674,
53.3621044196136));
#21067=CARTESIAN_POINT('',(-3.22274878139355,0.00280259281299765,53.3277091182931));
#21068=CARTESIAN_POINT('Ctrl Pts',(-0.490582106922522,-3.18519179310563,
53.6117903092821));
#21069=CARTESIAN_POINT('Ctrl Pts',(-0.542014919510384,-3.17727012960677,
53.6087878737367));
#21070=CARTESIAN_POINT('Ctrl Pts',(-0.593275039676424,-3.16809975755217,
53.6057559209604));
#21071=CARTESIAN_POINT('Ctrl Pts',(-0.697634432052406,-3.14680549719471,
53.5994822420388));
#21072=CARTESIAN_POINT('Ctrl Pts',(-0.750664989935348,-3.13457815352351,
53.5962400949983));
#21073=CARTESIAN_POINT('Ctrl Pts',(-0.838201641574686,-3.11204596025405,
53.5907841464142));
#21074=CARTESIAN_POINT('Ctrl Pts',(-0.87289108300727,-3.10249464900551,
53.5885944928083));
#21075=CARTESIAN_POINT('Ctrl Pts',(-0.941740120137199,-3.08229183778636,
53.5841899883102));
#21076=CARTESIAN_POINT('Ctrl Pts',(-0.975896674804988,-3.07164824554058,
53.5819756621852));
#21077=CARTESIAN_POINT('Ctrl Pts',(-1.06048476309417,-3.04373629956317,
53.5764158496298));
#21078=CARTESIAN_POINT('Ctrl Pts',(-1.11067689086895,-3.02578170096815,
53.5730485014055));
#21079=CARTESIAN_POINT('Ctrl Pts',(-1.34001434028316,-2.93726857360369,
53.5573364486652));
#21080=CARTESIAN_POINT('Ctrl Pts',(-1.5130314919546,-2.85199950145234,53.5445188741822));
#21081=CARTESIAN_POINT('Ctrl Pts',(-1.84303283713041,-2.65084565155453,
53.5184485190678));
#21082=CARTESIAN_POINT('Ctrl Pts',(-1.99923645699547,-2.53511652309719,
53.5052505247895));
#21083=CARTESIAN_POINT('Ctrl Pts',(-2.17119508503107,-2.38187901746128,
53.4903444127689));
#21084=CARTESIAN_POINT('Ctrl Pts',(-2.19789219749092,-2.35726661471363,
53.4880191149323));
#21085=CARTESIAN_POINT('Ctrl Pts',(-2.23950172106203,-2.31758462999663,
53.4843850485082));
#21086=CARTESIAN_POINT('Ctrl Pts',(-2.2546904625627,-2.30281077217671,53.4830563438441));
#21087=CARTESIAN_POINT('Ctrl Pts',(-2.28435786558828,-2.27337878579174,
53.4804587726769));
#21088=CARTESIAN_POINT('Ctrl Pts',(-2.29884370906879,-2.25872964319822,
53.4791894359282));
#21089=CARTESIAN_POINT('Ctrl Pts',(-2.33648500443717,-2.21992676938085,
53.4758851561427));
#21090=CARTESIAN_POINT('Ctrl Pts',(-2.35940721955533,-2.19554886255723,
53.4738669397837));
#21091=CARTESIAN_POINT('Ctrl Pts',(-2.41003588117067,-2.13999616012176,
53.4693834933687));
#21092=CARTESIAN_POINT('Ctrl Pts',(-2.43752551789892,-2.10863134854571,
53.4669309945015));
#21093=CARTESIAN_POINT('Ctrl Pts',(-2.52550648138278,-2.00422722741648,
53.4589876534119));
#21094=CARTESIAN_POINT('Ctrl Pts',(-2.58338646591933,-1.9290479896424,53.4536091394));
#21095=CARTESIAN_POINT('Ctrl Pts',(-2.78507248332578,-1.64168971448005,
53.4338519998825));
#21096=CARTESIAN_POINT('Ctrl Pts',(-2.90672641004,-1.41517026243518,53.4197251268083));
#21097=CARTESIAN_POINT('Ctrl Pts',(-3.01959072066893,-1.12738148000629,
53.4014916866001));
#21098=CARTESIAN_POINT('Ctrl Pts',(-3.0376918180448,-1.07765721281974,53.3983356144902));
#21099=CARTESIAN_POINT('Ctrl Pts',(-3.06480770888264,-0.997047815542967,
53.3931980953715));
#21100=CARTESIAN_POINT('Ctrl Pts',(-3.0745987976094,-0.966433007509562,
53.3912421439505));
#21101=CARTESIAN_POINT('Ctrl Pts',(-3.09420701175458,-0.901805666908098,
53.3871005917486));
#21102=CARTESIAN_POINT('Ctrl Pts',(-3.10392485207667,-0.867767738204134,
53.3849120876854));
#21103=CARTESIAN_POINT('Ctrl Pts',(-3.12631366810605,-0.784154451084484,
53.379515579172));
#21104=CARTESIAN_POINT('Ctrl Pts',(-3.13836806270366,-0.734425477669683,
53.3762884692533));
#21105=CARTESIAN_POINT('Ctrl Pts',(-3.19830959240318,-0.458620681204706,
53.3582846235088));
#21106=CARTESIAN_POINT('Ctrl Pts',(-3.22294714079275,-0.228227449020224,
53.3427859443142));
#21107=CARTESIAN_POINT('Ctrl Pts',(-3.22274881214297,0.00276700761489099,
53.3271823260263));
#21108=CARTESIAN_POINT('Ctrl Pts',(-3.22274878139355,0.00280259281299765,
53.3277091182931));
#21109=CARTESIAN_POINT('Ctrl Pts',(-3.22262670745773,0.143177472133502,
53.3190327436128));
#21110=CARTESIAN_POINT('Ctrl Pts',(-3.21332957379828,0.283164167668086,
53.3103563689325));
#21111=CARTESIAN_POINT('Ctrl Pts',(-3.19502939606302,0.421787530390862,
53.3016799942521));
#21112=CARTESIAN_POINT('Ctrl Pts',(-3.18475329542461,0.499628721158624,
53.296807948708));
#21113=CARTESIAN_POINT('Ctrl Pts',(-3.17163920981312,0.577040641109694,
53.2919359031639));
#21114=CARTESIAN_POINT('Ctrl Pts',(-3.15572373989173,0.653854142744276,
53.2870638576197));
#21115=CARTESIAN_POINT('Ctrl Pts',(-3.13554371359198,0.751249852127526,
53.2808863455702));
#21116=CARTESIAN_POINT('Ctrl Pts',(-3.11081578012451,0.8478782970476,53.2747088335206));
#21117=CARTESIAN_POINT('Ctrl Pts',(-3.08161241256265,0.943282832049788,
53.268531321471));
#21118=CARTESIAN_POINT('Ctrl Pts',(-3.05244806418123,1.03855989521991,53.262362063314));
#21119=CARTESIAN_POINT('Ctrl Pts',(-3.01882029357804,1.13261588800971,53.2561928051569));
#21120=CARTESIAN_POINT('Ctrl Pts',(-2.98085259523344,1.22500423182539,53.2500235469999));
#21121=CARTESIAN_POINT('Ctrl Pts',(-2.94292446595288,1.317296290629,53.2438607183021));
#21122=CARTESIAN_POINT('Ctrl Pts',(-2.90066556548995,1.40792375713449,53.2376978896043));
#21123=CARTESIAN_POINT('Ctrl Pts',(-2.85424892698835,1.4964560218349,53.2315350609066));
#21124=CARTESIAN_POINT('Ctrl Pts',(-2.8078653971926,1.5849251370095,53.225376628117));
#21125=CARTESIAN_POINT('Ctrl Pts',(-2.75733022663391,1.67130163902001,53.2192181953275));
#21126=CARTESIAN_POINT('Ctrl Pts',(-2.70286383602891,1.75517652855407,53.213059762538));
#21127=CARTESIAN_POINT('Ctrl Pts',(-2.64841743736294,1.8390206317324,53.2069035902069));
#21128=CARTESIAN_POINT('Ctrl Pts',(-2.59004292187591,1.92036458391123,53.2007474178758));
#21129=CARTESIAN_POINT('Ctrl Pts',(-2.52800531551196,1.99882632743402,53.1945912455447));
#21130=CARTESIAN_POINT('Ctrl Pts',(-2.46597396908345,2.07728015373565,53.1884356944052));
#21131=CARTESIAN_POINT('Ctrl Pts',(-2.40028053564343,2.15285200967157,53.1822801432658));
#21132=CARTESIAN_POINT('Ctrl Pts',(-2.33123118856794,2.22519183621281,53.1761245921263));
#21133=CARTESIAN_POINT('Ctrl Pts',(-2.26217043203404,2.29754361591912,53.1699680238664));
#21134=CARTESIAN_POINT('Ctrl Pts',(-2.18975295971744,2.36666199184607,53.1638114556064));
#21135=CARTESIAN_POINT('Ctrl Pts',(-2.11432204988025,2.43223350685954,53.1576548873465));
#21136=CARTESIAN_POINT('Ctrl Pts',(-2.03881132895827,2.49787440104071,53.1514918050144));
#21137=CARTESIAN_POINT('Ctrl Pts',(-1.9602811318023,2.55996065599349,53.1453287226823));
#21138=CARTESIAN_POINT('Ctrl Pts',(-1.87910798997542,2.6182189985772,53.1391656403501));
#21139=CARTESIAN_POINT('Ctrl Pts',(-1.79788902548743,2.67651022829857,53.1329990789259));
#21140=CARTESIAN_POINT('Ctrl Pts',(-1.71402450854919,2.73096900614671,53.1268325175018));
#21141=CARTESIAN_POINT('Ctrl Pts',(-1.6279183862366,2.78136644300115,53.1206659560776));
#21142=CARTESIAN_POINT('Ctrl Pts',(-1.54167251566397,2.83184567373878,53.1144893864658));
#21143=CARTESIAN_POINT('Ctrl Pts',(-1.45317815752836,2.87825019745168,53.1083128168539));
#21144=CARTESIAN_POINT('Ctrl Pts',(-1.36286225037172,2.92039792648395,53.1021362472421));
#21145=CARTESIAN_POINT('Ctrl Pts',(-1.30153121563375,2.94901928361566,53.0979419096403));
#21146=CARTESIAN_POINT('Ctrl Pts',(-1.23936062752267,2.97567866694849,53.0937475720386));
#21147=CARTESIAN_POINT('Ctrl Pts',(-1.17648823748014,3.0003321465416,53.0895532344368));
#21148=CARTESIAN_POINT('Ctrl Pts',(-1.08388844404121,3.03664231570056,53.0833757247975));
#21149=CARTESIAN_POINT('Ctrl Pts',(-0.98944653174153,3.06872416127268,53.0771982151581));
#21150=CARTESIAN_POINT('Ctrl Pts',(-0.893584562560482,3.09638889548028,
53.0710207055188));
#21151=CARTESIAN_POINT('Ctrl Pts',(-0.797850676486028,3.12401666627966,
53.0648514497744));
#21152=CARTESIAN_POINT('Ctrl Pts',(-0.700700917939257,3.14723893772386,
53.0586821940301));
#21153=CARTESIAN_POINT('Ctrl Pts',(-0.602576792875929,3.16591515539936,
53.0525129382857));
#21154=CARTESIAN_POINT('Ctrl Pts',(-0.504554930552762,3.18457190914391,
53.0463501119999));
#21155=CARTESIAN_POINT('Ctrl Pts',(-0.405561144255584,3.19869194827091,
53.0401872857141));
#21156=CARTESIAN_POINT('Ctrl Pts',(-0.306050630364382,3.2081849345313,53.0340244594283));
#21157=CARTESIAN_POINT('Ctrl Pts',(-0.206611096568207,3.21767114951656,
53.0278660290398));
#21158=CARTESIAN_POINT('Ctrl Pts',(-0.106655998286694,3.22253683273671,
53.0217075986512));
#21159=CARTESIAN_POINT('Ctrl Pts',(-0.00664832232328756,3.22274314246579,
53.0155491682627));
#21160=CARTESIAN_POINT('Ctrl Pts',(0.0933226458389801,3.22294937646892,
53.0093929983251));
#21161=CARTESIAN_POINT('Ctrl Pts',(0.19334572030702,3.21849963457444,53.0032368283874));
#21162=CARTESIAN_POINT('Ctrl Pts',(0.292956109397393,3.20940715404991,52.9970806584497));
#21163=CARTESIAN_POINT('Ctrl Pts',(0.392556447416537,3.20031559099162,52.9909251096933));
#21164=CARTESIAN_POINT('Ctrl Pts',(0.491743751176398,3.1865822602719,52.9847695609368));
#21165=CARTESIAN_POINT('Ctrl Pts',(0.590057548787154,3.16827234492543,52.9786140121804));
#21166=CARTESIAN_POINT('Ctrl Pts',(0.688387591623784,3.14995940407574,52.9724574462902));
#21167=CARTESIAN_POINT('Ctrl Pts',(0.785843415434532,3.1270684558414,52.9663008804));
#21168=CARTESIAN_POINT('Ctrl Pts',(0.881974932271338,3.09971575815347,52.9601443145098));
#21169=CARTESIAN_POINT('Ctrl Pts',(0.978208163440187,3.07233411926638,52.9539812345126));
#21170=CARTESIAN_POINT('Ctrl Pts',(1.07311387208691,3.04048142343067,52.9478181545155));
#21171=CARTESIAN_POINT('Ctrl Pts',(1.16625745873088,3.0043237346289,52.9416550745183));
#21172=CARTESIAN_POINT('Ctrl Pts',(1.25945362567591,2.96814563452206,52.935488515413));
#21173=CARTESIAN_POINT('Ctrl Pts',(1.35088529327482,2.92765787710775,52.9293219563078));
#21174=CARTESIAN_POINT('Ctrl Pts',(1.44014005775924,2.88307373761705,52.9231553972026));
#21175=CARTESIAN_POINT('Ctrl Pts',(1.52953968144246,2.83841723870933,52.9169788298606));
#21176=CARTESIAN_POINT('Ctrl Pts',(1.61675496724579,2.78965129091158,52.9108022625187));
#21177=CARTESIAN_POINT('Ctrl Pts',(1.7014001489357,2.73703399608071,52.9046256951767));
#21178=CARTESIAN_POINT('Ctrl Pts',(1.75888069683518,2.70130283128805,52.9004313338691));
#21179=CARTESIAN_POINT('Ctrl Pts',(1.81517665591439,2.66379654871379,52.8962369725616));
#21180=CARTESIAN_POINT('Ctrl Pts',(1.87017596998735,2.62460652361108,52.892042611254));
#21181=CARTESIAN_POINT('Ctrl Pts',(1.95117970363851,2.56688692458135,52.88586509919));
#21182=CARTESIAN_POINT('Ctrl Pts',(2.02964841309519,2.50531430026754,52.879687587126));
#21183=CARTESIAN_POINT('Ctrl Pts',(2.10519338421395,2.44013900783578,52.8735100750621));
#21184=CARTESIAN_POINT('Ctrl Pts',(2.18063741804477,2.37505079753749,52.867340816907));
#21185=CARTESIAN_POINT('Ctrl Pts',(2.25316515312644,2.30636976803818,52.861171558752));
#21186=CARTESIAN_POINT('Ctrl Pts',(2.32241765031869,2.23438891421976,52.855002300597));
#21187=CARTESIAN_POINT('Ctrl Pts',(2.3915979739655,2.16248307738463,52.8488394719175));
#21188=CARTESIAN_POINT('Ctrl Pts',(2.45750954733497,2.08728456446029,52.842676643238));
#21189=CARTESIAN_POINT('Ctrl Pts',(2.51982801044539,2.00912527241951,52.8365138145585));
#21190=CARTESIAN_POINT('Ctrl Pts',(2.58210202193359,1.93102173122927,52.830355381811));
#21191=CARTESIAN_POINT('Ctrl Pts',(2.64078774953701,1.84996194792784,52.8241969490636));
#21192=CARTESIAN_POINT('Ctrl Pts',(2.69559970826759,1.7663124795142,52.8180385163162));
#21193=CARTESIAN_POINT('Ctrl Pts',(2.75039154808751,1.6826937149145,52.8118823440419));
#21194=CARTESIAN_POINT('Ctrl Pts',(2.80131220720641,1.59648751629959,52.8057261717675));
#21195=CARTESIAN_POINT('Ctrl Pts',(2.84811883367611,1.50809040569833,52.7995699994932));
#21196=CARTESIAN_POINT('Ctrl Pts',(2.89492073698975,1.41970221505949,52.793414448425));
#21197=CARTESIAN_POINT('Ctrl Pts',(2.93760923031824,1.32912393514834,52.7872588973568));
#21198=CARTESIAN_POINT('Ctrl Pts',(2.9759873293797,1.23677685047523,52.7811033462886));
#21199=CARTESIAN_POINT('Ctrl Pts',(3.01437176980688,1.14441450692658,52.7749467781142));
#21200=CARTESIAN_POINT('Ctrl Pts',(3.04844423488406,1.05028317838321,52.7687902099399));
#21201=CARTESIAN_POINT('Ctrl Pts',(3.07805619173572,0.954823356970983,52.7626336417655));
#21202=CARTESIAN_POINT('Ctrl Pts',(3.10769947997009,0.859262532838365,52.7564705595403));
#21203=CARTESIAN_POINT('Ctrl Pts',(3.13287270768393,0.762370823919694,52.750307477315));
#21204=CARTESIAN_POINT('Ctrl Pts',(3.15347751953469,0.664602961390698,52.7441443950898));
#21205=CARTESIAN_POINT('Ctrl Pts',(3.17409396286887,0.566779908584761,52.7379778337845));
#21206=CARTESIAN_POINT('Ctrl Pts',(3.19013678486609,0.468080144975986,52.7318112724793));
#21207=CARTESIAN_POINT('Ctrl Pts',(3.20155929892123,0.368965605430828,52.7256447111741));
#21208=CARTESIAN_POINT('Ctrl Pts',(3.21300035142143,0.269690205549891,52.7194681416992));
#21209=CARTESIAN_POINT('Ctrl Pts',(3.21980608988906,0.169999117734282,52.7132915722244));
#21210=CARTESIAN_POINT('Ctrl Pts',(3.22198192598891,0.0703564574201773,
52.7071150027495));
#21211=CARTESIAN_POINT('Ctrl Pts',(3.22345947636126,0.00269187098393442,
52.7029206645234));
#21212=CARTESIAN_POINT('Ctrl Pts',(3.22280308774812,-0.0649503896133836,
52.6987263262972));
#21213=CARTESIAN_POINT('Ctrl Pts',(3.22002806994389,-0.132426550485002,
52.6945319880711));
#21214=CARTESIAN_POINT('Ctrl Pts',(3.21594096084956,-0.231806968992186,
52.6883544717025));
#21215=CARTESIAN_POINT('Ctrl Pts',(3.20724170618463,-0.331169256470755,
52.6821769553339));
#21216=CARTESIAN_POINT('Ctrl Pts',(3.19392762109117,-0.430051059446254,
52.6759994389653));
#21217=CARTESIAN_POINT('Ctrl Pts',(3.18063132513885,-0.528800745018493,
52.6698301764654));
#21218=CARTESIAN_POINT('Ctrl Pts',(3.16273251235513,-0.627070796217695,
52.6636609139655));
#21219=CARTESIAN_POINT('Ctrl Pts',(3.1402804769695,-0.72440050280501,52.6574916514657));
#21220=CARTESIAN_POINT('Ctrl Pts',(3.11785184049886,-0.821628774957042,
52.6513288184073));
#21221=CARTESIAN_POINT('Ctrl Pts',(3.09087951293835,-0.917918230806609,
52.645165985349));
#21222=CARTESIAN_POINT('Ctrl Pts',(3.05946426354687,-1.0128158680528,52.6390031522906));
#21223=CARTESIAN_POINT('Ctrl Pts',(3.02807142240255,-1.10764581557021,52.632844715132));
#21224=CARTESIAN_POINT('Ctrl Pts',(2.99224209627347,-1.20108550804784,52.6266862779734));
#21225=CARTESIAN_POINT('Ctrl Pts',(2.95212732349995,-1.29269556676929,52.6205278408148));
#21226=CARTESIAN_POINT('Ctrl Pts',(2.91202727485667,-1.38427200001207,52.614371664111));
#21227=CARTESIAN_POINT('Ctrl Pts',(2.86764507901428,-1.47401973734669,52.6082154874072));
#21228=CARTESIAN_POINT('Ctrl Pts',(2.81918016427108,-1.56151873632064,52.6020593107034));
#21229=CARTESIAN_POINT('Ctrl Pts',(2.77072013991374,-1.64900890614737,52.5959037551929));
#21230=CARTESIAN_POINT('Ctrl Pts',(2.71817842590117,-1.73425040963265,52.5897481996823));
#21231=CARTESIAN_POINT('Ctrl Pts',(2.66180025029488,-1.81684809217228,52.5835926441718));
#21232=CARTESIAN_POINT('Ctrl Pts',(2.6054127590379,-1.89945942274416,52.5774360715478));
#21233=CARTESIAN_POINT('Ctrl Pts',(2.54518779139796,-1.9794257065864,52.5712794989237));
#21234=CARTESIAN_POINT('Ctrl Pts',(2.48141313430962,-2.05638187586247,52.5651229262997));
#21235=CARTESIAN_POINT('Ctrl Pts',(2.41757099968903,-2.13341946952608,52.558959839641));
#21236=CARTESIAN_POINT('Ctrl Pts',(2.3501719533757,-2.20744025486283,52.5527967529822));
#21237=CARTESIAN_POINT('Ctrl Pts',(2.27954312278993,-2.27811341110163,52.5466336663235));
#21238=CARTESIAN_POINT('Ctrl Pts',(2.20887442205615,-2.34882646251038,52.5404671005873));
#21239=CARTESIAN_POINT('Ctrl Pts',(2.13497262636165,-2.41618782936041,52.534300534851));
#21240=CARTESIAN_POINT('Ctrl Pts',(2.05819912582431,-2.47990603067052,52.5281339691147));
#21241=CARTESIAN_POINT('Ctrl Pts',(1.9813010245793,-2.54372764439402,52.5219573952579));
#21242=CARTESIAN_POINT('Ctrl Pts',(1.90152225611161,-2.60389402243564,52.515780821401));
#21243=CARTESIAN_POINT('Ctrl Pts',(1.81925450076102,-2.66015612774151,52.5096042475441));
#21244=CARTESIAN_POINT('Ctrl Pts',(1.76338935956113,-2.6983617460147,52.5054099533255));
#21245=CARTESIAN_POINT('Ctrl Pts',(1.70637706542877,-2.73476790802879,52.5012156591069));
#21246=CARTESIAN_POINT('Ctrl Pts',(1.64834639751306,-2.76930888784651,52.4970213648882));
#21247=CARTESIAN_POINT('Ctrl Pts',(1.56289523468098,-2.82017107842255,52.4908451940614));
#21248=CARTESIAN_POINT('Ctrl Pts',(1.47494049959711,-2.86716211889021,52.4846690232346));
#21249=CARTESIAN_POINT('Ctrl Pts',(1.38486771824877,-2.91002731352344,52.4784928524078));
#21250=CARTESIAN_POINT('Ctrl Pts',(1.29490670478629,-2.95283931836826,52.4723243453563));
#21251=CARTESIAN_POINT('Ctrl Pts',(1.2028332546352,-2.99153546474498,52.4661558383048));
#21252=CARTESIAN_POINT('Ctrl Pts',(1.10906001329222,-3.0259053933354,52.4599873312532));
#21253=CARTESIAN_POINT('Ctrl Pts',(1.01537816395696,-3.06024182477104,52.4538248360686));
#21254=CARTESIAN_POINT('Ctrl Pts',(0.920000220491095,-3.09026026975514,
52.4476623408839));
#21255=CARTESIAN_POINT('Ctrl Pts',(0.823360576297346,-3.11579763847065,
52.4414998456993));
#21256=CARTESIAN_POINT('Ctrl Pts',(0.726789391592974,-3.1413169165233,52.435341716024));
#21257=CARTESIAN_POINT('Ctrl Pts',(0.628958700957384,-3.16236131916738,
52.4291835863488));
#21258=CARTESIAN_POINT('Ctrl Pts',(0.53031895751404,-3.17881729040869,52.4230254566735));
#21259=CARTESIAN_POINT('Ctrl Pts',(0.431709789962919,-3.19526816070401,
52.4168692358669));
#21260=CARTESIAN_POINT('Ctrl Pts',(0.332292494402997,-3.20713335100443,
52.4107130150602));
#21261=CARTESIAN_POINT('Ctrl Pts',(0.232527846560202,-3.21435037963724,
52.4045567942536));
#21262=CARTESIAN_POINT('Ctrl Pts',(0.13278130284569,-3.22156609860761,52.3984016906063));
#21263=CARTESIAN_POINT('Ctrl Pts',(0.0326879648162029,-3.22413530683116,
52.392246586959));
#21264=CARTESIAN_POINT('Ctrl Pts',(-0.067287323570641,-3.22204748236067,
52.3860914833117));
#21265=CARTESIAN_POINT('Ctrl Pts',(-0.167298174937415,-3.21995891521405,
52.3799341901851));
#21266=CARTESIAN_POINT('Ctrl Pts',(-0.267190459316207,-3.21321001964345,
52.3737768970585));
#21267=CARTESIAN_POINT('Ctrl Pts',(-0.366501012415672,-3.20184237126038,
52.3676196039319));
#21268=CARTESIAN_POINT('Ctrl Pts',(-0.407973875882795,-3.19709515241385,
52.3650482701794));
#21269=CARTESIAN_POINT('Ctrl Pts',(-0.449345351154687,-3.19154306339272,
52.3624769364268));
#21270=CARTESIAN_POINT('Ctrl Pts',(-0.490582094296232,-3.18519179505033,
52.3599056026743));
#21271=CARTESIAN_POINT('Origin',(-9.35406549764863E-15,0.,41.4527091182931));
#21272=CARTESIAN_POINT('',(-0.490581718709063,-3.18519185289811,50.8612231915357));
#21273=CARTESIAN_POINT('',(-0.49058209429631,-3.18519179505032,51.1068136617517));
#21274=CARTESIAN_POINT('',(-0.490582094296226,-3.18519179505033,41.4527091182931));
#21275=CARTESIAN_POINT('Ctrl Pts',(-0.490581718709059,-3.18519185289811,
50.8612231915357));
#21276=CARTESIAN_POINT('Ctrl Pts',(-0.346603507787341,-3.20736730776321,
50.8708079128671));
#21277=CARTESIAN_POINT('Ctrl Pts',(-0.201224047347916,-3.2197648351351,
50.8806253624206));
#21278=CARTESIAN_POINT('Ctrl Pts',(0.1150624159999,-3.22520666569334,50.9019986000714));
#21279=CARTESIAN_POINT('Ctrl Pts',(0.285543187370928,-3.21460291450712,
50.9135292413597));
#21280=CARTESIAN_POINT('Ctrl Pts',(0.488056539100501,-3.18576120491405,
50.9267353279802));
#21281=CARTESIAN_POINT('Ctrl Pts',(0.521641609968407,-3.18043454307468,
50.9289084276596));
#21282=CARTESIAN_POINT('Ctrl Pts',(0.575570297106993,-3.17100404577209,
50.9323637964471));
#21283=CARTESIAN_POINT('Ctrl Pts',(0.595968704995193,-3.16723367992426,
50.9336628875048));
#21284=CARTESIAN_POINT('Ctrl Pts',(0.634376982659992,-3.1597502221884,50.936092228012));
#21285=CARTESIAN_POINT('Ctrl Pts',(0.652394097027578,-3.15607946690025,
50.9372248275988));
#21286=CARTESIAN_POINT('Ctrl Pts',(0.702356005513021,-3.14545423736711,
50.9403485842437));
#21287=CARTESIAN_POINT('Ctrl Pts',(0.734228799388278,-3.13816739117671,
50.9423220171601));
#21288=CARTESIAN_POINT('Ctrl Pts',(0.926956716171972,-3.09100819109944,
50.9541675753366));
#21289=CARTESIAN_POINT('Ctrl Pts',(1.08466822331222,-3.03925775677906,50.9634977044365));
#21290=CARTESIAN_POINT('Ctrl Pts',(1.43189930086637,-2.89482545794972,50.9845750620373));
#21291=CARTESIAN_POINT('Ctrl Pts',(1.61769665727226,-2.79524588710479,50.9962710778001));
#21292=CARTESIAN_POINT('Ctrl Pts',(1.84387196464562,-2.64387598105526,51.0121969983384));
#21293=CARTESIAN_POINT('Ctrl Pts',(1.89427575841785,-2.60799974044836,51.0158626894327));
#21294=CARTESIAN_POINT('Ctrl Pts',(1.97332125325968,-2.54823621668385,51.021822659834));
#21295=CARTESIAN_POINT('Ctrl Pts',(2.00263616536732,-2.5252629162438,51.0240817384394));
#21296=CARTESIAN_POINT('Ctrl Pts',(2.0584374705346,-2.47995015881982,51.0284812358785));
#21297=CARTESIAN_POINT('Ctrl Pts',(2.08497475014839,-2.45768137749764,51.0306186339193));
#21298=CARTESIAN_POINT('Ctrl Pts',(2.14702063563997,-2.40388731594316,51.0357272300583));
#21299=CARTESIAN_POINT('Ctrl Pts',(2.18220082050033,-2.37199726669711,51.0387132513175));
#21300=CARTESIAN_POINT('Ctrl Pts',(2.3053730472564,-2.25528448618121,51.0494995720332));
#21301=CARTESIAN_POINT('Ctrl Pts',(2.389220932612,-2.16625726332375,51.0574750639635));
#21302=CARTESIAN_POINT('Ctrl Pts',(2.58347978933681,-1.93496740901208,51.0775535106357));
#21303=CARTESIAN_POINT('Ctrl Pts',(2.68741904657515,-1.7878030636864,51.0898063567217));
#21304=CARTESIAN_POINT('Ctrl Pts',(2.83427673859514,-1.53788784604615,51.1092852271069));
#21305=CARTESIAN_POINT('Ctrl Pts',(2.88513103190173,-1.44022461591109,51.1165977823114));
#21306=CARTESIAN_POINT('Ctrl Pts',(2.94360296329596,-1.31234650712155,51.1256407533031));
#21307=CARTESIAN_POINT('Ctrl Pts',(2.95591738980371,-1.2843692243956,51.1275876747268));
#21308=CARTESIAN_POINT('Ctrl Pts',(2.97561886967302,-1.23782427249649,51.1307699319569));
#21309=CARTESIAN_POINT('Ctrl Pts',(2.98323443214233,-1.21935597565351,51.1320179641752));
#21310=CARTESIAN_POINT('Ctrl Pts',(2.99886244208603,-1.18043384541739,51.1346161762013));
#21311=CARTESIAN_POINT('Ctrl Pts',(3.00683829787248,-1.15996703580725,51.1359643526674));
#21312=CARTESIAN_POINT('Ctrl Pts',(3.02878747762368,-1.10189528038919,51.1397430450231));
#21313=CARTESIAN_POINT('Ctrl Pts',(3.0422692744859,-1.06410750346113,51.1421471368228));
#21314=CARTESIAN_POINT('Ctrl Pts',(3.12061738068006,-0.830833547553012,
51.1567111321666));
#21315=CARTESIAN_POINT('Ctrl Pts',(3.16733195316815,-0.629733207815807,
51.1681063791059));
#21316=CARTESIAN_POINT('Ctrl Pts',(3.21651895832334,-0.260478884034092,
51.1889981250994));
#21317=CARTESIAN_POINT('Ctrl Pts',(3.22567868455243,-0.0939853738832021,
51.1984062918477));
#21318=CARTESIAN_POINT('Ctrl Pts',(3.22065257180319,0.129495373666211,51.2115439284476));
#21319=CARTESIAN_POINT('Ctrl Pts',(3.21785579060651,0.186482089594798,51.2149366843071));
#21320=CARTESIAN_POINT('Ctrl Pts',(3.21079058959678,0.279776647418364,51.2205771230478));
#21321=CARTESIAN_POINT('Ctrl Pts',(3.20741426102531,0.316140433246197,51.2227971000573));
#21322=CARTESIAN_POINT('Ctrl Pts',(3.19958700258732,0.387284891404672,51.2271861862824));
#21323=CARTESIAN_POINT('Ctrl Pts',(3.19518494281967,0.422065874680274,51.2293534789949));
#21324=CARTESIAN_POINT('Ctrl Pts',(3.18299535808989,0.50720207704881,51.2347143525462));
#21325=CARTESIAN_POINT('Ctrl Pts',(3.17457956266573,0.557456302039472,51.2379270350474));
#21326=CARTESIAN_POINT('Ctrl Pts',(3.11563230704754,0.864568132425557,51.257868077414));
#21327=CARTESIAN_POINT('Ctrl Pts',(3.03515583084424,1.11464158858787,51.27555112519));
#21328=CARTESIAN_POINT('Ctrl Pts',(2.88623442755968,1.43682427464072,51.2994778972471));
#21329=CARTESIAN_POINT('Ctrl Pts',(2.84345176478616,1.51973580875641,51.3057347663267));
#21330=CARTESIAN_POINT('Ctrl Pts',(2.77661474829883,1.63653122452382,51.3145955464418));
#21331=CARTESIAN_POINT('Ctrl Pts',(2.75540952640791,1.6719876049724,51.3172917694867));
#21332=CARTESIAN_POINT('Ctrl Pts',(2.71592255916043,1.73521955886606,51.3220990328241));
#21333=CARTESIAN_POINT('Ctrl Pts',(2.69788166009409,1.76313839828696,51.3242211714526));
#21334=CARTESIAN_POINT('Ctrl Pts',(2.66796672148072,1.80789804311074,51.3276164868225));
#21335=CARTESIAN_POINT('Ctrl Pts',(2.65635780657193,1.82491233640051,51.3289054704183));
#21336=CARTESIAN_POINT('Ctrl Pts',(2.63240932739258,1.85929897064144,51.3315052694796));
#21337=CARTESIAN_POINT('Ctrl Pts',(2.62005909514223,1.87666244326464,51.3328153336423));
#21338=CARTESIAN_POINT('Ctrl Pts',(2.58590029482987,1.92369249444011,51.3363600838525));
#21339=CARTESIAN_POINT('Ctrl Pts',(2.5637534790662,1.95311072473937,51.3385733875717));
#21340=CARTESIAN_POINT('Ctrl Pts',(2.42667250734329,2.1288483460997,51.3518136277443));
#21341=CARTESIAN_POINT('Ctrl Pts',(2.29973613525833,2.26538379113368,51.3621933499323));
#21342=CARTESIAN_POINT('Ctrl Pts',(2.01063772102105,2.52684504155757,51.384030565213));
#21343=CARTESIAN_POINT('Ctrl Pts',(1.84696527851101,2.64883337279974,51.395463614612));
#21344=CARTESIAN_POINT('Ctrl Pts',(1.62901682843735,2.78119683519003,51.410527483014));
#21345=CARTESIAN_POINT('Ctrl Pts',(1.58452130994426,2.80678525154454,51.4135928571634));
#21346=CARTESIAN_POINT('Ctrl Pts',(1.50830482397528,2.84822571859362,51.418838267375));
#21347=CARTESIAN_POINT('Ctrl Pts',(1.47689808388018,2.86463698952662,51.4209982456831));
#21348=CARTESIAN_POINT('Ctrl Pts',(1.41266704353984,2.89686321598575,51.4254159398403));
#21349=CARTESIAN_POINT('Ctrl Pts',(1.37983247801889,2.91264601838906,51.4276743714946));
#21350=CARTESIAN_POINT('Ctrl Pts',(1.29516182583676,2.95159217654632,51.4335016314827));
#21351=CARTESIAN_POINT('Ctrl Pts',(1.24297011679141,2.97394774250894,51.4370969994106));
#21352=CARTESIAN_POINT('Ctrl Pts',(0.988677768890194,3.0750068848551,51.454639813883));
#21353=CARTESIAN_POINT('Ctrl Pts',(0.779595516522362,3.13454234023561,51.4691922759406));
#21354=CARTESIAN_POINT('Ctrl Pts',(0.39979282705659,3.20231809729583,51.4952551462515));
#21355=CARTESIAN_POINT('Ctrl Pts',(0.231338474068705,3.2188767490565,51.506672442795));
#21356=CARTESIAN_POINT('Ctrl Pts',(0.0293193802694555,3.22278597400439,
51.5197022294294));
#21357=CARTESIAN_POINT('Ctrl Pts',(-0.00372164682127379,3.22291721981298,
51.5218116568994));
#21358=CARTESIAN_POINT('Ctrl Pts',(-0.0572742518132538,3.2223063324279,
51.5251893829077));
#21359=CARTESIAN_POINT('Ctrl Pts',(-0.077786379463264,3.22187643959687,
51.5264733312751));
#21360=CARTESIAN_POINT('Ctrl Pts',(-0.119561239700812,3.22060171287252,
51.5290663577978));
#21361=CARTESIAN_POINT('Ctrl Pts',(-0.14082231175952,3.21974213535921,51.5303746427153));
#21362=CARTESIAN_POINT('Ctrl Pts',(-0.198812265089489,3.21682209151492,
51.5339156026212));
#21363=CARTESIAN_POINT('Ctrl Pts',(-0.235517922746272,3.21434320657835,
51.5361268811256));
#21364=CARTESIAN_POINT('Ctrl Pts',(-0.458029135002967,3.19548382103351,
51.5493923809504));
#21365=CARTESIAN_POINT('Ctrl Pts',(-0.642186449231802,3.16362442705648,
51.5597945833701));
#21366=CARTESIAN_POINT('Ctrl Pts',(-1.01918283315119,3.06410422450463,51.5816340366025));
#21367=CARTESIAN_POINT('Ctrl Pts',(-1.21042222813626,2.99371599481762,51.5930465330263));
#21368=CARTESIAN_POINT('Ctrl Pts',(-1.44004501231891,2.88357842866269,51.6080893068275));
#21369=CARTESIAN_POINT('Ctrl Pts',(-1.48580352517005,2.86026950510811,51.6111558005791));
#21370=CARTESIAN_POINT('Ctrl Pts',(-1.56214170148145,2.81905739919269,51.6164006095534));
#21371=CARTESIAN_POINT('Ctrl Pts',(-1.59301917340379,2.80172466075089,51.6185587832939));
#21372=CARTESIAN_POINT('Ctrl Pts',(-1.65501558965293,2.76556744084902,51.6229704193284));
#21373=CARTESIAN_POINT('Ctrl Pts',(-1.6861139120703,2.74671796440172,51.6252245574796));
#21374=CARTESIAN_POINT('Ctrl Pts',(-1.76476684405288,2.69720534457655,51.631035075565));
#21375=CARTESIAN_POINT('Ctrl Pts',(-1.81184340207097,2.66580973280929,51.6346177844948));
#21376=CARTESIAN_POINT('Ctrl Pts',(-2.03673184592032,2.50712109071081,51.6522606835108));
#21377=CARTESIAN_POINT('Ctrl Pts',(-2.20207695971448,2.36321030941291,51.6669386121071));
#21378=CARTESIAN_POINT('Ctrl Pts',(-2.46596731120831,2.08161405691009,51.69300981072));
#21379=CARTESIAN_POINT('Ctrl Pts',(-2.57070504651076,1.95079388933501,51.7043098415843));
#21380=CARTESIAN_POINT('Ctrl Pts',(-2.68341493073205,1.78507579751925,51.7172344133315));
#21381=CARTESIAN_POINT('Ctrl Pts',(-2.70159267324075,1.75744374533985,51.7193460893101));
#21382=CARTESIAN_POINT('Ctrl Pts',(-2.7303511136458,1.71222695149777,51.7227258778065));
#21383=CARTESIAN_POINT('Ctrl Pts',(-2.7411945696428,1.69481289319038,51.7240097005034));
#21384=CARTESIAN_POINT('Ctrl Pts',(-2.76294500248613,1.65912783394793,51.7266025944916));
#21385=CARTESIAN_POINT('Ctrl Pts',(-2.77383868125454,1.64085017146012,51.7279108788143));
#21386=CARTESIAN_POINT('Ctrl Pts',(-2.80304538038821,1.59072426953281,51.731448954046));
#21387=CARTESIAN_POINT('Ctrl Pts',(-2.82099667124735,1.55866774595962,51.733657445387));
#21388=CARTESIAN_POINT('Ctrl Pts',(-2.9465997406804,1.32509043253427,51.749413133658));
#21389=CARTESIAN_POINT('Ctrl Pts',(-3.03311178645538,1.11291174552003,51.761975992925));
#21390=CARTESIAN_POINT('Ctrl Pts',(-3.12715878885688,0.786931921859993,
51.7810388781258));
#21391=CARTESIAN_POINT('Ctrl Pts',(-3.15235230131314,0.679011595659373,
51.7873069667753));
#21392=CARTESIAN_POINT('Ctrl Pts',(-3.18595249730045,0.492037487787791,
51.7982993464871));
#21393=CARTESIAN_POINT('Ctrl Pts',(-3.19708423195664,0.413576107576438,
51.8029506050496));
#21394=CARTESIAN_POINT('Ctrl Pts',(-3.20952927375639,0.29442544989722,51.8101175680425));
#21395=CARTESIAN_POINT('Ctrl Pts',(-3.21298216889166,0.253987917458752,
51.8125676195864));
#21396=CARTESIAN_POINT('Ctrl Pts',(-3.21771480389859,0.182705541190045,
51.8169226661762));
#21397=CARTESIAN_POINT('Ctrl Pts',(-3.21931672008742,0.151886886554207,
51.8188173963318));
#21398=CARTESIAN_POINT('Ctrl Pts',(-3.22200518489214,0.0803620702082446,
51.8232443299988));
#21399=CARTESIAN_POINT('Ctrl Pts',(-3.22276327758165,0.0396495831764976,
51.82578640537));
#21400=CARTESIAN_POINT('Ctrl Pts',(-3.22272338396855,-0.0810807397634633,
51.8333946720167));
#21401=CARTESIAN_POINT('Ctrl Pts',(-3.21971698248088,-0.161061791120952,
51.8385268269826));
#21402=CARTESIAN_POINT('Ctrl Pts',(-3.20533209376363,-0.353009526920111,
51.8510656580518));
#21403=CARTESIAN_POINT('Ctrl Pts',(-3.19106031479194,-0.464650453387044,
51.8585434419437));
#21404=CARTESIAN_POINT('Ctrl Pts',(-3.131004613375,-0.795664927442708,51.8811449957779));
#21405=CARTESIAN_POINT('Ctrl Pts',(-3.06816503194015,-1.0112582683208,51.8964783897741));
#21406=CARTESIAN_POINT('Ctrl Pts',(-2.96930069525715,-1.25330621883191,
51.9134191186105));
#21407=CARTESIAN_POINT('Ctrl Pts',(-2.95451939493151,-1.28776493137933,
51.9158226554828));
#21408=CARTESIAN_POINT('Ctrl Pts',(-2.93034641479588,-1.34150921001089,
51.9195497804402));
#21409=CARTESIAN_POINT('Ctrl Pts',(-2.92135826160687,-1.36097135862665,
51.9208949327615));
#21410=CARTESIAN_POINT('Ctrl Pts',(-2.90342884304259,-1.3987979188145,51.923498401907));
#21411=CARTESIAN_POINT('Ctrl Pts',(-2.89450603912762,-1.4171695318841,51.9247575849345));
#21412=CARTESIAN_POINT('Ctrl Pts',(-2.87090960728617,-1.46460072022845,
51.9279978236705));
#21413=CARTESIAN_POINT('Ctrl Pts',(-2.8559687982564,-1.49352591214228,51.9299633657896));
#21414=CARTESIAN_POINT('Ctrl Pts',(-2.76662488307548,-1.66024912815791,
51.9412599735414));
#21415=CARTESIAN_POINT('Ctrl Pts',(-2.68268737323053,-1.79271851829971,
51.9501106139534));
#21416=CARTESIAN_POINT('Ctrl Pts',(-2.45045738311239,-2.10615280965664,
51.972005068897));
#21417=CARTESIAN_POINT('Ctrl Pts',(-2.29151660715481,-2.27806122643698,
51.9849552002255));
#21418=CARTESIAN_POINT('Ctrl Pts',(-2.07390624900671,-2.46739874427539,
52.0019366578584));
#21419=CARTESIAN_POINT('Ctrl Pts',(-2.03148992694457,-2.50243718078142,
52.0052128068452));
#21420=CARTESIAN_POINT('Ctrl Pts',(-1.95979693775776,-2.5586355573769,52.0107096367362));
#21421=CARTESIAN_POINT('Ctrl Pts',(-1.93102338649137,-2.58042021217952,
52.0129053629018));
#21422=CARTESIAN_POINT('Ctrl Pts',(-1.87309028198291,-2.62277011839903,
52.0173093869278));
#21423=CARTESIAN_POINT('Ctrl Pts',(-1.84394297457001,-2.64334342139428,
52.0195169432223));
#21424=CARTESIAN_POINT('Ctrl Pts',(-1.77086616487369,-2.69312701778929,
52.0250345151969));
#21425=CARTESIAN_POINT('Ctrl Pts',(-1.72655088265893,-2.72174973819913,
52.0283656720968));
#21426=CARTESIAN_POINT('Ctrl Pts',(-1.62857106013073,-2.781677801534,52.0357029435847));
#21427=CARTESIAN_POINT('Ctrl Pts',(-1.57466414675696,-2.81254460048031,
52.0397224537275));
#21428=CARTESIAN_POINT('Ctrl Pts',(-1.40294072168675,-2.90438768757778,
52.0524687891351));
#21429=CARTESIAN_POINT('Ctrl Pts',(-1.2822384618318,-2.95965705729563,52.0613510735051));
#21430=CARTESIAN_POINT('Ctrl Pts',(-0.978661125312268,-3.07660118106556,
52.0832985959682));
#21431=CARTESIAN_POINT('Ctrl Pts',(-0.792976734036559,-3.12960856421699,
52.0964054959467));
#21432=CARTESIAN_POINT('Ctrl Pts',(-0.567880417754941,-3.17253149297339,
52.1112373287149));
#21433=CARTESIAN_POINT('Ctrl Pts',(-0.531986622331881,-3.17874735268946,
52.113570359628));
#21434=CARTESIAN_POINT('Ctrl Pts',(-0.494189929094215,-3.18463454861332,
52.1159882262296));
#21435=CARTESIAN_POINT('Ctrl Pts',(-0.492386130713441,-3.18491393801041,
52.1161035231083));
#21436=CARTESIAN_POINT('Ctrl Pts',(-0.49058209429419,-3.18519179505064,
52.1162187418821));
#21437=CARTESIAN_POINT('',(-3.22274931785554,-0.00209684566102432,52.0777091182931));
#21438=CARTESIAN_POINT('Ctrl Pts',(-0.490582094296232,-3.18519179505033,
52.3599056026743));
#21439=CARTESIAN_POINT('Ctrl Pts',(-0.589440239020645,-3.16996569916734,
52.353741263183));
#21440=CARTESIAN_POINT('Ctrl Pts',(-0.68752304555204,-3.15014310743925,
52.3475769236916));
#21441=CARTESIAN_POINT('Ctrl Pts',(-0.784379920417554,-3.12583840000499,
52.3414125842003));
#21442=CARTESIAN_POINT('Ctrl Pts',(-0.881301117565013,-3.10151755190703,
52.3352441509945));
#21443=CARTESIAN_POINT('Ctrl Pts',(-0.976994347927334,-3.07270878719306,
52.3290757177888));
#21444=CARTESIAN_POINT('Ctrl Pts',(-1.07102569701638,-3.03957587811698,
52.322907284583));
#21445=CARTESIAN_POINT('Ctrl Pts',(-1.16519852671715,-3.00639311689808,
52.3167295702842));
#21446=CARTESIAN_POINT('Ctrl Pts',(-1.25770408491926,-2.96887339055742,
52.3105518559853));
#21447=CARTESIAN_POINT('Ctrl Pts',(-1.34813007879941,-2.92722784441805,
52.3043741416865));
#21448=CARTESIAN_POINT('Ctrl Pts',(-1.37185933936709,-2.91629937160376,
52.3027530083595));
#21449=CARTESIAN_POINT('Ctrl Pts',(-1.39544553924316,-2.90508702448003,
52.3011318750324));
#21450=CARTESIAN_POINT('Ctrl Pts',(-1.41888154641625,-2.89359512021628,
52.2995107417054));
#21451=CARTESIAN_POINT('Ctrl Pts',(-1.50818724395349,-2.84980384985502,
52.2933332200183));
#21452=CARTESIAN_POINT('Ctrl Pts',(-1.59561763230012,-2.80179885452189,
52.2871556983311));
#21453=CARTESIAN_POINT('Ctrl Pts',(-1.68074848388976,-2.74976400740178,
52.280978176644));
#21454=CARTESIAN_POINT('Ctrl Pts',(-1.76576558933375,-2.69779868576144,
52.2748089089478));
#21455=CARTESIAN_POINT('Ctrl Pts',(-1.84848889858135,-2.64181443927142,
52.2686396412516));
#21456=CARTESIAN_POINT('Ctrl Pts',(-1.92851663570881,-2.58204205006317,
52.2624703735555));
#21457=CARTESIAN_POINT('Ctrl Pts',(-2.00846096847379,-2.52233195523178,
52.2563075354281));
#21458=CARTESIAN_POINT('Ctrl Pts',(-2.08571496917602,-2.45884182514739,
52.2501446973007));
#21459=CARTESIAN_POINT('Ctrl Pts',(-2.15990466079608,-2.39184644548337,
52.2439818591733));
#21460=CARTESIAN_POINT('Ctrl Pts',(-2.23404143102699,-2.32489885532327,
52.2378234171547));
#21461=CARTESIAN_POINT('Ctrl Pts',(-2.305117917431,-2.25445127668952,52.231664975136));
#21462=CARTESIAN_POINT('Ctrl Pts',(-2.37279286988877,-2.18081901108393,
52.2255065331174));
#21463=CARTESIAN_POINT('Ctrl Pts',(-2.44044298084045,-2.10721377374076,
52.2193503516837));
#21464=CARTESIAN_POINT('Ctrl Pts',(-2.50469374599709,-2.0304264912499,52.21319417025));
#21465=CARTESIAN_POINT('Ctrl Pts',(-2.56524111306123,-1.95080895896048,
52.2070379888162));
#21466=CARTESIAN_POINT('Ctrl Pts',(-2.62578236922915,-1.87119946227195,
52.2008824287107));
#21467=CARTESIAN_POINT('Ctrl Pts',(-2.68262070816888,-1.78876062884767,
52.1947268686052));
#21468=CARTESIAN_POINT('Ctrl Pts',(-2.735493312346,-1.70387614004375,52.1885713084996));
#21469=CARTESIAN_POINT('Ctrl Pts',(-2.78837465172301,-1.61897762728566,
52.1824147314204));
#21470=CARTESIAN_POINT('Ctrl Pts',(-2.83728872571689,-1.53163302452011,
52.1762581543411));
#21471=CARTESIAN_POINT('Ctrl Pts',(-2.88201740350844,-1.44225283788057,
52.1701015772619));
#21472=CARTESIAN_POINT('Ctrl Pts',(-2.92679340522606,-1.35277808503532,
52.1639384863885));
#21473=CARTESIAN_POINT('Ctrl Pts',(-2.96737497435138,-1.26126383629905,
52.1577753955151));
#21474=CARTESIAN_POINT('Ctrl Pts',(-3.00359117726584,-1.1681428004961,52.1516123046418));
#21475=CARTESIAN_POINT('Ctrl Pts',(-3.03982782354858,-1.07496919961244,
52.145445734819));
#21476=CARTESIAN_POINT('Ctrl Pts',(-3.07169405802658,-0.980187416157667,
52.1392791649963));
#21477=CARTESIAN_POINT('Ctrl Pts',(-3.09906875876202,-0.884245662112788,
52.1331125951736));
#21478=CARTESIAN_POINT('Ctrl Pts',(-3.12648788655829,-0.78814820188564,
52.1269360174762));
#21479=CARTESIAN_POINT('Ctrl Pts',(-3.14940082251084,-0.690887433118548,
52.1207594397788));
#21480=CARTESIAN_POINT('Ctrl Pts',(-3.16773749635297,-0.592922184354288,
52.1145828620815));
#21481=CARTESIAN_POINT('Ctrl Pts',(-3.18018914169148,-0.526398203854166,
52.1103886142285));
#21482=CARTESIAN_POINT('Ctrl Pts',(-3.19053166669938,-0.45954954615121,
52.1061943663755));
#21483=CARTESIAN_POINT('Ctrl Pts',(-3.19875681761807,-0.392520552636372,
52.1020001185225));
#21484=CARTESIAN_POINT('Ctrl Pts',(-3.21463548048016,-0.263121007202109,
52.0939031184461));
#21485=CARTESIAN_POINT('Ctrl Pts',(-3.22266431702142,-0.132738974111897,
52.0858061183696));
#21486=CARTESIAN_POINT('Ctrl Pts',(-3.22274931785554,-0.00209684566102432,
52.0777091182931));
#21487=CARTESIAN_POINT('Ctrl Pts',(-0.49058209429631,-3.18519179505032,
51.1068136617517));
#21488=CARTESIAN_POINT('Ctrl Pts',(-0.490290107655991,-3.18523676672761,
51.1068316447501));
#21489=CARTESIAN_POINT('Ctrl Pts',(-0.489998114782029,-3.18528169838757,
51.1068496298593));
#21490=CARTESIAN_POINT('Ctrl Pts',(-0.468096712346372,-3.18864877873823,
51.1081987512924));
#21491=CARTESIAN_POINT('Ctrl Pts',(-0.446454779646167,-3.19175087250692,
51.1095409714125));
#21492=CARTESIAN_POINT('Ctrl Pts',(-0.404815837904996,-3.19728751664578,
51.1121436895462));
#21493=CARTESIAN_POINT('Ctrl Pts',(-0.384824715757757,-3.19975517514846,
51.1134024422831));
#21494=CARTESIAN_POINT('Ctrl Pts',(-0.333899886945455,-3.2055571173243,
51.1166302994167));
#21495=CARTESIAN_POINT('Ctrl Pts',(-0.302939026454846,-3.20863107052092,
51.1186126466662));
#21496=CARTESIAN_POINT('Ctrl Pts',(-0.154965786186221,-3.22116193810289,
51.1281666872916));
#21497=CARTESIAN_POINT('Ctrl Pts',(-0.0375478319452818,-3.22466801702292,
51.1359823598414));
#21498=CARTESIAN_POINT('Ctrl Pts',(0.259554203716849,-3.21731020474563,
51.1559707327345));
#21499=CARTESIAN_POINT('Ctrl Pts',(0.438645180692646,-3.19781966457959,
51.1681998515738));
#21500=CARTESIAN_POINT('Ctrl Pts',(0.727511777596534,-3.1416460708504,51.1876991900715));
#21501=CARTESIAN_POINT('Ctrl Pts',(0.838610496093273,-3.11383214988942,
51.1951478109563));
#21502=CARTESIAN_POINT('Ctrl Pts',(0.988197115764423,-3.06779277200161,
51.2050859567072));
#21503=CARTESIAN_POINT('Ctrl Pts',(1.02814512885269,-3.05463645800857,51.2077314169602));
#21504=CARTESIAN_POINT('Ctrl Pts',(1.10068721352603,-3.02916131506546,51.2125215864282));
#21505=CARTESIAN_POINT('Ctrl Pts',(1.13336040919608,-3.01708882000855,51.214673918202));
#21506=CARTESIAN_POINT('Ctrl Pts',(1.1999816092941,-2.99123777817153,51.2190542336476));
#21507=CARTESIAN_POINT('Ctrl Pts',(1.23390331379865,-2.97740526120672,51.2212800514071));
#21508=CARTESIAN_POINT('Ctrl Pts',(1.32089412138698,-2.94019021743242,51.2269811971863));
#21509=CARTESIAN_POINT('Ctrl Pts',(1.37358228803536,-2.91594789076526,51.2304273539274));
#21510=CARTESIAN_POINT('Ctrl Pts',(1.58200656681976,-2.81314609925882,51.2440732512367));
#21511=CARTESIAN_POINT('Ctrl Pts',(1.73190786415949,-2.72342405145618,51.2538997102635));
#21512=CARTESIAN_POINT('Ctrl Pts',(2.04042777626394,-2.50293940724075,51.2751490872247));
#21513=CARTESIAN_POINT('Ctrl Pts',(2.1952856898368,-2.368280410139,51.2865044750282));
#21514=CARTESIAN_POINT('Ctrl Pts',(2.36051924651906,-2.19437969419563,51.3007821596266));
#21515=CARTESIAN_POINT('Ctrl Pts',(2.38431388412331,-2.16850188626445,51.3028985868121));
#21516=CARTESIAN_POINT('Ctrl Pts',(2.42159804535607,-2.12659796658401,51.3063227184349));
#21517=CARTESIAN_POINT('Ctrl Pts',(2.43536348757143,-2.11081989564496,51.3076113502371));
#21518=CARTESIAN_POINT('Ctrl Pts',(2.46249915356084,-2.07909798131315,51.3102034803851));
#21519=CARTESIAN_POINT('Ctrl Pts',(2.47587064688338,-2.06315655691087,51.311506787569));
#21520=CARTESIAN_POINT('Ctrl Pts',(2.51097698385488,-2.0204701974759,51.3149958302204));
#21521=CARTESIAN_POINT('Ctrl Pts',(2.53243823152593,-1.99350485725825,51.317199033236));
#21522=CARTESIAN_POINT('Ctrl Pts',(2.57993098342679,-1.93182709324429,51.3222268375603));
#21523=CARTESIAN_POINT('Ctrl Pts',(2.60570204253932,-1.89692285624048,51.3250640883028));
#21524=CARTESIAN_POINT('Ctrl Pts',(2.68939254143697,-1.77864818238451,51.3346249068805));
#21525=CARTESIAN_POINT('Ctrl Pts',(2.74407525939569,-1.69306545881416,51.3414551200959));
#21526=CARTESIAN_POINT('Ctrl Pts',(2.91638846445753,-1.39304303545962,51.3648122754991));
#21527=CARTESIAN_POINT('Ctrl Pts',(3.01365172664422,-1.16783184519339,51.3812963766599));
#21528=CARTESIAN_POINT('Ctrl Pts',(3.10003600224227,-0.882476852655956,
51.4003571228152));
#21529=CARTESIAN_POINT('Ctrl Pts',(3.11428020503107,-0.830811627159511,
51.403743220065));
#21530=CARTESIAN_POINT('Ctrl Pts',(3.13502534927322,-0.747511954259369,
51.4091021868561));
#21531=CARTESIAN_POINT('Ctrl Pts',(3.14235038933667,-0.716095114170127,
51.4111008261522));
#21532=CARTESIAN_POINT('Ctrl Pts',(3.15670181977314,-0.650075002280733,
51.415255608819));
#21533=CARTESIAN_POINT('Ctrl Pts',(3.1636337704346,-0.61545544660668,51.4174085180746));
#21534=CARTESIAN_POINT('Ctrl Pts',(3.17911033525125,-0.530974151325396,
51.4226035957965));
#21535=CARTESIAN_POINT('Ctrl Pts',(3.18705271958366,-0.481010864800697,
51.4256266401028));
#21536=CARTESIAN_POINT('Ctrl Pts',(3.21809515478472,-0.250914287982896,
51.4393523052373));
#21537=CARTESIAN_POINT('Ctrl Pts',(3.22712156888969,-0.0692120845311815,
51.4496181978966));
#21538=CARTESIAN_POINT('Ctrl Pts',(3.21351051033534,0.321159625871323,51.4715234059123));
#21539=CARTESIAN_POINT('Ctrl Pts',(3.18593029833733,0.528792442210811,51.4830862323664));
#21540=CARTESIAN_POINT('Ctrl Pts',(3.12998248802018,0.768581636709448,51.497705460616));
#21541=CARTESIAN_POINT('Ctrl Pts',(3.12088027545296,0.804744772095314,51.4999458853901));
#21542=CARTESIAN_POINT('Ctrl Pts',(3.10557133090353,0.861395420711091,51.5035235629975));
#21543=CARTESIAN_POINT('Ctrl Pts',(3.09978416848768,0.881993997396937,51.5048387240409));
#21544=CARTESIAN_POINT('Ctrl Pts',(3.08806406623339,0.922169342552654,51.50743457907));
#21545=CARTESIAN_POINT('Ctrl Pts',(3.08214905722959,0.94175001238857,51.5087143087785));
#21546=CARTESIAN_POINT('Ctrl Pts',(3.0662916496347,0.992493342557641,51.5120663669271));
#21547=CARTESIAN_POINT('Ctrl Pts',(3.05606062919632,1.02356277558895,51.514153918756));
#21548=CARTESIAN_POINT('Ctrl Pts',(2.99048064656726,1.21296090783879,51.5270733460814));
#21549=CARTESIAN_POINT('Ctrl Pts',(2.92331800224965,1.3669129551894,51.5383971390847));
#21550=CARTESIAN_POINT('Ctrl Pts',(2.74161808155065,1.70808059803781,51.5645073229794));
#21551=CARTESIAN_POINT('Ctrl Pts',(2.61932502007288,1.89028368108255,51.5792006897566));
#21552=CARTESIAN_POINT('Ctrl Pts',(2.44336519088943,2.10220883763423,51.5968563902201));
#21553=CARTESIAN_POINT('Ctrl Pts',(2.4061004205941,2.14476032631172,51.6004375258929));
#21554=CARTESIAN_POINT('Ctrl Pts',(2.34305528999035,2.21303699275526,51.6062474625127));
#21555=CARTESIAN_POINT('Ctrl Pts',(2.31792591084968,2.23934375802175,51.6085025191718));
#21556=CARTESIAN_POINT('Ctrl Pts',(2.26744178830494,2.29043263662587,51.6129174383105));
#21557=CARTESIAN_POINT('Ctrl Pts',(2.2421129261613,2.31523297034333,51.6150779515386));
#21558=CARTESIAN_POINT('Ctrl Pts',(2.17902922843028,2.37499392599764,51.6203313436629));
#21559=CARTESIAN_POINT('Ctrl Pts',(2.14083583868097,2.40947854845139,51.623403979037));
#21560=CARTESIAN_POINT('Ctrl Pts',(2.05631498153327,2.48219489121072,51.6299894891352));
#21561=CARTESIAN_POINT('Ctrl Pts',(2.00971132950778,2.52007613681449,51.6334887955878));
#21562=CARTESIAN_POINT('Ctrl Pts',(1.8631835979615,2.63252799328865,51.6441392890125));
#21563=CARTESIAN_POINT('Ctrl Pts',(1.75996882270117,2.7026226154538,51.6511553475141));
#21564=CARTESIAN_POINT('Ctrl Pts',(1.47365435942886,2.87368797625666,51.6698507839225));
#21565=CARTESIAN_POINT('Ctrl Pts',(1.28439195996141,2.96311594629629,51.6814201138146));
#21566=CARTESIAN_POINT('Ctrl Pts',(1.0551891854481,3.04530727265274,51.6959219249024));
#21567=CARTESIAN_POINT('Ctrl Pts',(1.02235465232164,3.0564867656135,51.6980112112522));
#21568=CARTESIAN_POINT('Ctrl Pts',(0.969502823696837,3.07353487511818,51.7014025669018));
#21569=CARTESIAN_POINT('Ctrl Pts',(0.949596993810202,3.0797431466081,51.7026862376561));
#21570=CARTESIAN_POINT('Ctrl Pts',(0.90961467911149,3.09178844680354,51.7052798980192));
#21571=CARTESIAN_POINT('Ctrl Pts',(0.889538842442377,3.09762413076188,51.7065898759589));
#21572=CARTESIAN_POINT('Ctrl Pts',(0.835749975787081,3.11269358323241,51.7101174358386));
#21573=CARTESIAN_POINT('Ctrl Pts',(0.801942000068785,3.12157462909925,51.7123531330496));
#21574=CARTESIAN_POINT('Ctrl Pts',(0.725051079468145,3.14044168467961,51.717469508535));
#21575=CARTESIAN_POINT('Ctrl Pts',(0.681893810142788,3.15009420773003,51.7203634611653));
#21576=CARTESIAN_POINT('Ctrl Pts',(0.535673901478936,3.17965214954521,51.7302143335137));
#21577=CARTESIAN_POINT('Ctrl Pts',(0.431844089580025,3.19540967775533,51.7372837866577));
#21578=CARTESIAN_POINT('Ctrl Pts',(0.0914729767297211,3.23017175029711,
51.7603879707462));
#21579=CARTESIAN_POINT('Ctrl Pts',(-0.146468486493921,3.22815085417305,
51.7763622917443));
#21580=CARTESIAN_POINT('Ctrl Pts',(-0.436209392761729,3.19355806952478,
51.7950334414112));
#21581=CARTESIAN_POINT('Ctrl Pts',(-0.490190750646011,3.18571897372396,
51.7984822437652));
#21582=CARTESIAN_POINT('Ctrl Pts',(-0.579431127491248,3.17043734628283,
51.804137093452));
#21583=CARTESIAN_POINT('Ctrl Pts',(-0.614809173474371,3.16376725511623,
51.8063666532724));
#21584=CARTESIAN_POINT('Ctrl Pts',(-0.685081857004411,3.1492948879866,51.8107732613681));
#21585=CARTESIAN_POINT('Ctrl Pts',(-0.719973131141142,3.1415019163951,51.8129502549527));
#21586=CARTESIAN_POINT('Ctrl Pts',(-0.806417913065924,3.12067853628499,
51.8183207485106));
#21587=CARTESIAN_POINT('Ctrl Pts',(-0.857793158825484,3.10694958964908,
51.8214917587533));
#21588=CARTESIAN_POINT('Ctrl Pts',(-1.09846725678583,3.03620910082595,51.8362843219656));
#21589=CARTESIAN_POINT('Ctrl Pts',(-1.28260132638872,2.9631300959435,51.84738499997));
#21590=CARTESIAN_POINT('Ctrl Pts',(-1.62686334038401,2.78835429070109,51.8690118830049));
#21591=CARTESIAN_POINT('Ctrl Pts',(-1.78701603336566,2.68852411073114,51.8795097837651));
#21592=CARTESIAN_POINT('Ctrl Pts',(-1.96686007627628,2.55321904865113,51.8928804843974));
#21593=CARTESIAN_POINT('Ctrl Pts',(-1.99582374975928,2.53064287779629,51.8950879438696));
#21594=CARTESIAN_POINT('Ctrl Pts',(-2.04094594220585,2.49421525743405,51.8986246515297));
#21595=CARTESIAN_POINT('Ctrl Pts',(-2.05736467762032,2.48068954407287,51.899932620253));
#21596=CARTESIAN_POINT('Ctrl Pts',(-2.08936686590869,2.45378999269332,51.9025264395873));
#21597=CARTESIAN_POINT('Ctrl Pts',(-2.10495861574456,2.44042790951428,51.9038115225685));
#21598=CARTESIAN_POINT('Ctrl Pts',(-2.14536402887971,2.40512532676235,51.9071956129615));
#21599=CARTESIAN_POINT('Ctrl Pts',(-2.16996854438321,2.38295005672354,51.9093103695604));
#21600=CARTESIAN_POINT('Ctrl Pts',(-2.31836503331676,2.24500084198258,51.9223768133586));
#21601=CARTESIAN_POINT('Ctrl Pts',(-2.43319689165671,2.11999730758702,51.9338273301582));
#21602=CARTESIAN_POINT('Ctrl Pts',(-2.67066272947989,1.81665502342507,51.9598499172809));
#21603=CARTESIAN_POINT('Ctrl Pts',(-2.78628762603418,1.63379986941337,51.9743292393177));
#21604=CARTESIAN_POINT('Ctrl Pts',(-2.90817058466921,1.3899238463634,51.9918082234132));
#21605=CARTESIAN_POINT('Ctrl Pts',(-2.93221893885977,1.33844581121686,51.9954061772336));
#21606=CARTESIAN_POINT('Ctrl Pts',(-2.96943423327285,1.25295837911296,52.0012358369022));
#21607=CARTESIAN_POINT('Ctrl Pts',(-2.98340652612153,1.21931539711588,52.0034941545762));
#21608=CARTESIAN_POINT('Ctrl Pts',(-3.00983145913836,1.15251295564747,52.0079104130502));
#21609=CARTESIAN_POINT('Ctrl Pts',(-3.02231377212018,1.11937086890504,52.0100690902119));
#21610=CARTESIAN_POINT('Ctrl Pts',(-3.05151870996004,1.03777540743443,52.0153090801155));
#21611=CARTESIAN_POINT('Ctrl Pts',(-3.06763686240202,0.98911513283617,52.0183704041163));
#21612=CARTESIAN_POINT('Ctrl Pts',(-3.14257448439993,0.743391774206481,
52.0335468520173));
#21613=CARTESIAN_POINT('Ctrl Pts',(-3.1835990865213,0.541399705689971,52.0450832042486));
#21614=CARTESIAN_POINT('Ctrl Pts',(-3.21693512294275,0.224218463995345,
52.0629479811517));
#21615=CARTESIAN_POINT('Ctrl Pts',(-3.22282683556096,0.111039161045053,
52.0692837228589));
#21616=CARTESIAN_POINT('Ctrl Pts',(-3.22274924355897,-0.00220808517695452,
52.0757655954735));
#21617=CARTESIAN_POINT('Origin',(-9.07107736682793E-15,0.,39.1419356690201));
#21618=CARTESIAN_POINT('',(-3.9329991429617,-0.00259643266821552,59.9877721469517));
#21619=CARTESIAN_POINT('',(-1.9005600208235,-3.44330663857395,60.199854037326));
#21620=CARTESIAN_POINT('Ctrl Pts',(-3.93299914296127,-0.00259643332659257,
59.9877721469851));
#21621=CARTESIAN_POINT('Ctrl Pts',(-3.93287035264033,-0.197684139483549,
59.9976703740445));
#21622=CARTESIAN_POINT('Ctrl Pts',(-3.91822346530484,-0.39225107737111,
60.007568601104));
#21623=CARTESIAN_POINT('Ctrl Pts',(-3.88930500305625,-0.584632870442379,
60.0174668281635));
#21624=CARTESIAN_POINT('Ctrl Pts',(-3.87231073497013,-0.697688251404115,
60.0232836355296));
#21625=CARTESIAN_POINT('Ctrl Pts',(-3.85035239201043,-0.810203799500005,
60.0291004428958));
#21626=CARTESIAN_POINT('Ctrl Pts',(-3.82347367061698,-0.921703905871498,
60.0349172502619));
#21627=CARTESIAN_POINT('Ctrl Pts',(-3.79662898496787,-1.03306282289629,
60.0407266919738));
#21628=CARTESIAN_POINT('Ctrl Pts',(-3.76487640454396,-1.14340844800533,
60.0465361336857));
#21629=CARTESIAN_POINT('Ctrl Pts',(-3.72831122421556,-1.25227170190353,
60.0523455753976));
#21630=CARTESIAN_POINT('Ctrl Pts',(-3.69178210763556,-1.36102758543014,
60.0581492873348));
#21631=CARTESIAN_POINT('Ctrl Pts',(-3.65044996275524,-1.46830360724953,
60.063952999272));
#21632=CARTESIAN_POINT('Ctrl Pts',(-3.6044606494612,-1.5736430429058,60.0697567112092));
#21633=CARTESIAN_POINT('Ctrl Pts',(-3.55850265691398,-1.6789107377693,60.0755564705631));
#21634=CARTESIAN_POINT('Ctrl Pts',(-3.50789397143091,-1.78224408377972,
60.081356229917));
#21635=CARTESIAN_POINT('Ctrl Pts',(-3.45282933167017,-1.88320434535348,
60.0871559892709));
#21636=CARTESIAN_POINT('Ctrl Pts',(-3.39778369812136,-1.9841297592984,60.0929537467692));
#21637=CARTESIAN_POINT('Ctrl Pts',(-3.33828536876333,-2.08268334678356,
60.0987515042675));
#21638=CARTESIAN_POINT('Ctrl Pts',(-3.27457566431122,-2.17844972829322,
60.1045492617658));
#21639=CARTESIAN_POINT('Ctrl Pts',(-3.210871814503,-2.27420730929021,60.1103464864755));
#21640=CARTESIAN_POINT('Ctrl Pts',(-3.14295759308554,-2.36717784261953,
60.1161437111852));
#21641=CARTESIAN_POINT('Ctrl Pts',(-3.07111794389987,-2.45697447578446,
60.1219409358949));
#21642=CARTESIAN_POINT('Ctrl Pts',(-2.99926670133485,-2.546785600201,60.1277390961524));
#21643=CARTESIAN_POINT('Ctrl Pts',(-2.92348903631433,-2.63342147777904,
60.1335372564098));
#21644=CARTESIAN_POINT('Ctrl Pts',(-2.84410997024081,-2.71652857102164,
60.1393354166673));
#21645=CARTESIAN_POINT('Ctrl Pts',(-2.76465456865678,-2.79971558486175,
60.1451391527717));
#21646=CARTESIAN_POINT('Ctrl Pts',(-2.68159114425714,-2.87936673488443,
60.1509428888762));
#21647=CARTESIAN_POINT('Ctrl Pts',(-2.59528131529041,-2.95516562894613,
60.1567466249806));
#21648=CARTESIAN_POINT('Ctrl Pts',(-2.50892457566129,-3.03100572082239,
60.162553515501));
#21649=CARTESIAN_POINT('Ctrl Pts',(-2.41931824729355,-3.10298912474427,
60.1683604060214));
#21650=CARTESIAN_POINT('Ctrl Pts',(-2.32685530004097,-3.170841120692,60.1741672965419));
#21651=CARTESIAN_POINT('Ctrl Pts',(-2.23426054396859,-3.23878984177961,
60.1799824649661));
#21652=CARTESIAN_POINT('Ctrl Pts',(-2.13880139026995,-3.30259516485508,
60.1857976333904));
#21653=CARTESIAN_POINT('Ctrl Pts',(-2.04089794694587,-3.36202685446624,
60.1916128018147));
#21654=CARTESIAN_POINT('Ctrl Pts',(-1.99464847917838,-3.39010231248604,
60.1943598803184));
#21655=CARTESIAN_POINT('Ctrl Pts',(-1.94785387496363,-3.41720242601197,
60.1971069588222));
#21656=CARTESIAN_POINT('Ctrl Pts',(-1.9005600208235,-3.44330663857395,60.199854037326));
#21657=CARTESIAN_POINT('',(-3.89175630324296,-0.568086152065691,60.1999356690201));
#21658=CARTESIAN_POINT('Origin',(-1.16499385964724E-14,0.,60.1999356690201));
#21659=CARTESIAN_POINT('',(-3.93059892528386,-0.000146120431290349,60.171099191055));
#21660=CARTESIAN_POINT('Origin',(0.0100450429162835,0.000746738084422618,
60.1858575446646));
#21661=CARTESIAN_POINT('',(-3.92955718600433,-0.000499007535493628,58.9210993909857));
#21662=CARTESIAN_POINT('Ctrl Pts',(-3.93059892528386,-0.000146120431290349,
60.171099191055));
#21663=CARTESIAN_POINT('Ctrl Pts',(-3.92287704520062,1.1109806906551,60.1148744759824));
#21664=CARTESIAN_POINT('Ctrl Pts',(-2.86359348088526,3.52391769303499,59.9928128865155));
#21665=CARTESIAN_POINT('Ctrl Pts',(1.23859575814269,4.47568193655585,59.8049144226543));
#21666=CARTESIAN_POINT('Ctrl Pts',(4.42193931558343,1.40645034585021,59.6074037994715));
#21667=CARTESIAN_POINT('Ctrl Pts',(3.59560445921063,-2.93448714587229,59.4098931762886));
#21668=CARTESIAN_POINT('Ctrl Pts',(-0.494193783132457,-4.61514490705407,
59.2123825531056));
#21669=CARTESIAN_POINT('Ctrl Pts',(-3.4976014503324,-2.5464335831811,59.0494513447149));
#21670=CARTESIAN_POINT('Ctrl Pts',(-3.92754117139867,-0.620745692192471,
58.9523570107183));
#21671=CARTESIAN_POINT('Ctrl Pts',(-3.92679976020224,-0.000501837635528756,
58.921099551116));
#21672=CARTESIAN_POINT('',(-3.93299855748857,0.00336850010244687,57.6710991910917));
#21673=CARTESIAN_POINT('Ctrl Pts',(-3.93299996879044,-0.000495474015325462,
58.921099191055));
#21674=CARTESIAN_POINT('Ctrl Pts',(-3.93301517740518,0.120228276276205,
58.915024855076));
#21675=CARTESIAN_POINT('Ctrl Pts',(-3.92746761809961,0.240871097188488,
58.9089505190969));
#21676=CARTESIAN_POINT('Ctrl Pts',(-3.91640559202178,0.3609102918741,58.9028761831179));
#21677=CARTESIAN_POINT('Ctrl Pts',(-3.90533220422532,0.481072777857684,
58.8967956082369));
#21678=CARTESIAN_POINT('Ctrl Pts',(-3.88873309117169,0.600630037137997,
58.8907150333559));
#21679=CARTESIAN_POINT('Ctrl Pts',(-3.86670805303361,0.719067335237196,
58.8846344584749));
#21680=CARTESIAN_POINT('Ctrl Pts',(-3.84463785679102,0.837747466236466,
58.8785414165446));
#21681=CARTESIAN_POINT('Ctrl Pts',(-3.81711956975119,0.955302685984484,
58.8724483746144));
#21682=CARTESIAN_POINT('Ctrl Pts',(-3.78430378778388,1.07123006014799,58.8663553326841));
#21683=CARTESIAN_POINT('Ctrl Pts',(-3.75145232548691,1.18728348119134,58.8602556658395));
#21684=CARTESIAN_POINT('Ctrl Pts',(-3.71329199556078,1.30170517931389,58.8541559989948));
#21685=CARTESIAN_POINT('Ctrl Pts',(-3.67002215593741,1.41401074074019,58.8480563321502));
#21686=CARTESIAN_POINT('Ctrl Pts',(-3.62665914886438,1.52655811546717,58.8419435316677));
#21687=CARTESIAN_POINT('Ctrl Pts',(-3.57816478743509,1.6369799095776,58.8358307311853));
#21688=CARTESIAN_POINT('Ctrl Pts',(-3.52478565957446,1.74481375913256,58.8297179307028));
#21689=CARTESIAN_POINT('Ctrl Pts',(-3.48881819467131,1.81747343632637,58.8255990560485));
#21690=CARTESIAN_POINT('Ctrl Pts',(-3.4506338904148,1.88895865836186,58.8214801813942));
#21691=CARTESIAN_POINT('Ctrl Pts',(-3.41031921957498,1.95913547785689,58.8173613067399));
#21692=CARTESIAN_POINT('Ctrl Pts',(-3.35279979340985,2.05926107241989,58.8114846543544));
#21693=CARTESIAN_POINT('Ctrl Pts',(-3.29077262038089,2.15701597551455,58.8056080019689));
#21694=CARTESIAN_POINT('Ctrl Pts',(-3.22445836314778,2.25196742079596,58.7997313495834));
#21695=CARTESIAN_POINT('Ctrl Pts',(-3.15822898990627,2.34679732573266,58.7938622194674));
#21696=CARTESIAN_POINT('Ctrl Pts',(-3.08772367999684,2.43883057417248,58.7879930893513));
#21697=CARTESIAN_POINT('Ctrl Pts',(-3.01320858671637,2.52765959198204,58.7821239592353));
#21698=CARTESIAN_POINT('Ctrl Pts',(-2.93876903204692,2.61639856064413,58.7762607788661));
#21699=CARTESIAN_POINT('Ctrl Pts',(-2.86032804329177,2.70193944562605,58.7703975984968));
#21700=CARTESIAN_POINT('Ctrl Pts',(-2.77819421823987,2.7839047910693,58.7645344181275));
#21701=CARTESIAN_POINT('Ctrl Pts',(-2.69374468321311,2.86818109631402,58.7585059291871));
#21702=CARTESIAN_POINT('Ctrl Pts',(-2.6053912299711,2.94867687489402,58.7524774402467));
#21703=CARTESIAN_POINT('Ctrl Pts',(-2.51351297430408,3.02501926076597,58.7464489513062));
#21704=CARTESIAN_POINT('Ctrl Pts',(-2.4242550254769,3.09918441248804,58.7405923908672));
#21705=CARTESIAN_POINT('Ctrl Pts',(-2.33167094470829,3.1694295916815,58.7347358304281));
#21706=CARTESIAN_POINT('Ctrl Pts',(-2.23614404117579,3.23545187371317,58.728879269989));
#21707=CARTESIAN_POINT('Ctrl Pts',(-2.14063102923534,3.30146455473638,58.7230235612152));
#21708=CARTESIAN_POINT('Ctrl Pts',(-2.04217638487188,3.3632553251924,58.7171678524414));
#21709=CARTESIAN_POINT('Ctrl Pts',(-1.94119363630154,3.42056373517326,58.7113121436677));
#21710=CARTESIAN_POINT('Ctrl Pts',(-1.84020122523329,3.47787762868868,58.7054558745925));
#21711=CARTESIAN_POINT('Ctrl Pts',(-1.73668058797224,3.53070810546995,58.6995996055173));
#21712=CARTESIAN_POINT('Ctrl Pts',(-1.63107053890545,3.57884030058827,58.6937433364422));
#21713=CARTESIAN_POINT('Ctrl Pts',(-1.52002420268137,3.62945010495387,58.6875856153684));
#21714=CARTESIAN_POINT('Ctrl Pts',(-1.40666808240071,3.67486484255668,58.6814278942946));
#21715=CARTESIAN_POINT('Ctrl Pts',(-1.29153552513395,3.71489232513097,58.6752701732209));
#21716=CARTESIAN_POINT('Ctrl Pts',(-1.18187620852402,3.75301695719783,58.6694051815899));
#21717=CARTESIAN_POINT('Ctrl Pts',(-1.0706058879835,3.78625469001799,58.6635401899589));
#21718=CARTESIAN_POINT('Ctrl Pts',(-0.958199284731031,3.81449120207938,
58.6576751983279));
#21719=CARTESIAN_POINT('Ctrl Pts',(-0.845715406440705,3.84274712561193,
58.6518061747501));
#21720=CARTESIAN_POINT('Ctrl Pts',(-0.732094093138896,3.8659948998238,58.6459371511722));
#21721=CARTESIAN_POINT('Ctrl Pts',(-0.617818407258544,3.88417165115711,
58.6400681275944));
#21722=CARTESIAN_POINT('Ctrl Pts',(-0.503380588905055,3.90237419136777,
58.634190777142));
#21723=CARTESIAN_POINT('Ctrl Pts',(-0.388286953575217,3.91549130603822,
58.6283134266895));
#21724=CARTESIAN_POINT('Ctrl Pts',(-0.273023805755644,3.92351207484961,
58.6224360762371));
#21725=CARTESIAN_POINT('Ctrl Pts',(-0.256122737773672,3.92468816245015,
58.6215742786771));
#21726=CARTESIAN_POINT('Ctrl Pts',(-0.239218020856951,3.92575476767173,
58.620712481117));
#21727=CARTESIAN_POINT('Ctrl Pts',(-0.222311181945052,3.92671195001393,
58.619850683557));
#21728=CARTESIAN_POINT('Ctrl Pts',(-0.10700287394539,3.93324014117381,58.6139730372979));
#21729=CARTESIAN_POINT('Ctrl Pts',(0.00878214788636485,3.93469566846353,
58.6080953910388));
#21730=CARTESIAN_POINT('Ctrl Pts',(0.12456068974397,3.9310270457694,58.6022177447797));
#21731=CARTESIAN_POINT('Ctrl Pts',(0.240191292869419,3.92736311074348,58.5963476088202));
#21732=CARTESIAN_POINT('Ctrl Pts',(0.355815023882455,3.91858806008751,58.5904774728607));
#21733=CARTESIAN_POINT('Ctrl Pts',(0.470944954097746,3.90470227420861,58.5846073369012));
#21734=CARTESIAN_POINT('Ctrl Pts',(0.585958402026291,3.89083053722289,58.5787431400303));
#21735=CARTESIAN_POINT('Ctrl Pts',(0.700478635806685,3.87185839966145,58.5728789431595));
#21736=CARTESIAN_POINT('Ctrl Pts',(0.814020779895871,3.84783824632711,58.5670147462886));
#21737=CARTESIAN_POINT('Ctrl Pts',(0.930736634853405,3.82314668571657,58.5609866343755));
#21738=CARTESIAN_POINT('Ctrl Pts',(1.0464184703894,3.7931207520833,58.5549585224624));
#21739=CARTESIAN_POINT('Ctrl Pts',(1.16054710083434,3.7578743229045,58.5489304105493));
#21740=CARTESIAN_POINT('Ctrl Pts',(1.2714474159559,3.72362489672985,58.5430728136593));
#21741=CARTESIAN_POINT('Ctrl Pts',(1.38088079823322,3.68444648681156,58.5372152167694));
#21742=CARTESIAN_POINT('Ctrl Pts',(1.48838400030628,3.64049475588583,58.5313576198794));
#21743=CARTESIAN_POINT('Ctrl Pts',(1.59587167488188,3.59654937323975,58.5255008690463));
#21744=CARTESIAN_POINT('Ctrl Pts',(1.7014293419421,3.5478321966265,58.5196441182132));
#21745=CARTESIAN_POINT('Ctrl Pts',(1.80461282742488,3.49454740175227,58.51378736738));
#21746=CARTESIAN_POINT('Ctrl Pts',(1.90780626312105,3.44125746850656,58.5079300517674));
#21747=CARTESIAN_POINT('Ctrl Pts',(2.00862469561104,3.3833992306576,58.5020727361547));
#21748=CARTESIAN_POINT('Ctrl Pts',(2.10664832181308,3.32122294466994,58.4962154205421));
#21749=CARTESIAN_POINT('Ctrl Pts',(2.20967519125197,3.255873106607,58.4900591405281));
#21750=CARTESIAN_POINT('Ctrl Pts',(2.30961398712476,3.18575304982132,58.4839028605141));
#21751=CARTESIAN_POINT('Ctrl Pts',(2.40601279290025,3.11120417851357,58.4777465805001));
#21752=CARTESIAN_POINT('Ctrl Pts',(2.4978668396267,3.04016994262838,58.4718805406927));
#21753=CARTESIAN_POINT('Ctrl Pts',(2.58650678668462,2.96511527905143,58.4660145008853));
#21754=CARTESIAN_POINT('Ctrl Pts',(2.67157741437195,2.88637542932614,58.4601484610779));
#21755=CARTESIAN_POINT('Ctrl Pts',(2.75670652072071,2.80758145279894,58.454278388878));
#21756=CARTESIAN_POINT('Ctrl Pts',(2.83826113280519,2.72509753832912,58.4484083166782));
#21757=CARTESIAN_POINT('Ctrl Pts',(2.91592456261376,2.63929402400447,58.4425382444783));
#21758=CARTESIAN_POINT('Ctrl Pts',(2.99369808532546,2.55336887768372,58.4366598510738));
#21759=CARTESIAN_POINT('Ctrl Pts',(3.06756915737192,2.46411505804202,58.4307814576694));
#21760=CARTESIAN_POINT('Ctrl Pts',(3.13726283111843,2.37193400592906,58.4249030642649));
#21761=CARTESIAN_POINT('Ctrl Pts',(3.14739174133141,2.35853689898954,58.4240487296347));
#21762=CARTESIAN_POINT('Ctrl Pts',(3.15743249326628,2.34507800797624,58.4231943950044));
#21763=CARTESIAN_POINT('Ctrl Pts',(3.16738432269095,2.33155861010859,58.4223400603742));
#21764=CARTESIAN_POINT('Ctrl Pts',(3.23584973491808,2.23854946489792,58.4164625106149));
#21765=CARTESIAN_POINT('Ctrl Pts',(3.30032708879234,2.14236967624017,58.4105849608556));
#21766=CARTESIAN_POINT('Ctrl Pts',(3.36050927456826,2.04339580491412,58.4047074110963));
#21767=CARTESIAN_POINT('Ctrl Pts',(3.42061456906435,1.94454838674922,58.3988373707407));
#21768=CARTESIAN_POINT('Ctrl Pts',(3.47643539673698,1.84291433477424,58.392967330385));
#21769=CARTESIAN_POINT('Ctrl Pts',(3.5277060482717,1.73890167548002,58.3870972900293));
#21770=CARTESIAN_POINT('Ctrl Pts',(3.57892483490984,1.6349942343887,58.3812331877498));
#21771=CARTESIAN_POINT('Ctrl Pts',(3.62560242006638,1.5287133401183,58.3753690854704));
#21772=CARTESIAN_POINT('Ctrl Pts',(3.6675177727531,1.42049371224939,58.3695049831909));
#21773=CARTESIAN_POINT('Ctrl Pts',(3.71060568748356,1.30924669179295,58.3634768354409));
#21774=CARTESIAN_POINT('Ctrl Pts',(3.74866075799241,1.19595124278602,58.3574486876909));
#21775=CARTESIAN_POINT('Ctrl Pts',(3.78149470033579,1.08110444977914,58.3514205399409));
#21776=CARTESIAN_POINT('Ctrl Pts',(3.81339919314155,0.969508691860899,58.3455630344818));
#21777=CARTESIAN_POINT('Ctrl Pts',(3.84037406709065,0.856448664069443,58.3397055290227));
#21778=CARTESIAN_POINT('Ctrl Pts',(3.86229661013189,0.74239739719614,58.3338480235635));
#21779=CARTESIAN_POINT('Ctrl Pts',(3.88421599171271,0.628362577710646,58.327991362818));
#21780=CARTESIAN_POINT('Ctrl Pts',(3.9010844133856,0.51333720836378,58.3221347020726));
#21781=CARTESIAN_POINT('Ctrl Pts',(3.91283021632444,0.397804849415293,58.3162780413271));
#21782=CARTESIAN_POINT('Ctrl Pts',(3.92457715486367,0.28226132063941,58.3104208143516));
#21783=CARTESIAN_POINT('Ctrl Pts',(3.93120044840834,0.166211115206717,58.3045635873761));
#21784=CARTESIAN_POINT('Ctrl Pts',(3.93268034856764,0.0501425566743083,
58.2987063604006));
#21785=CARTESIAN_POINT('Ctrl Pts',(3.9342358410513,-0.0718547072982891,
58.2925499501331));
#21786=CARTESIAN_POINT('Ctrl Pts',(3.930108598929,-0.193871740764238,58.2863935398657));
#21787=CARTESIAN_POINT('Ctrl Pts',(3.92033767649031,-0.315343467175775,
58.2802371295982));
#21788=CARTESIAN_POINT('Ctrl Pts',(3.91102773847,-0.431084253289698,58.2743711739142));
#21789=CARTESIAN_POINT('Ctrl Pts',(3.89659460221075,-0.546329601463841,
58.2685052182301));
#21790=CARTESIAN_POINT('Ctrl Pts',(3.87712498607451,-0.660598851313416,
58.2626392625461));
#21791=CARTESIAN_POINT('Ctrl Pts',(3.85764198086495,-0.774946683059798,
58.2567692728991));
#21792=CARTESIAN_POINT('Ctrl Pts',(3.83311568603728,-0.888316677816104,
58.2508992832521));
#21793=CARTESIAN_POINT('Ctrl Pts',(3.80368326664931,-1.00024127439931,58.245029293605));
#21794=CARTESIAN_POINT('Ctrl Pts',(3.77420911060816,-1.11232458569804,58.239150980017));
#21795=CARTESIAN_POINT('Ctrl Pts',(3.73981506972742,-1.22295801685179,58.233272666429));
#21796=CARTESIAN_POINT('Ctrl Pts',(3.70068716363292,-1.33169197524145,58.227394352841));
#21797=CARTESIAN_POINT('Ctrl Pts',(3.6949962015805,-1.34750679624183,58.2265393809577));
#21798=CARTESIAN_POINT('Ctrl Pts',(3.68920517855682,-1.3632814753923,58.2256844090745));
#21799=CARTESIAN_POINT('Ctrl Pts',(3.68331474828411,-1.37901467181196,58.2248294371912));
#21800=CARTESIAN_POINT('Ctrl Pts',(3.64282202938542,-1.48716974207072,58.2189520845137));
#21801=CARTESIAN_POINT('Ctrl Pts',(3.59749515991606,-1.59371713921449,58.2130747318362));
#21802=CARTESIAN_POINT('Ctrl Pts',(3.5474816969102,-1.69819392593632,58.2071973791587));
#21803=CARTESIAN_POINT('Ctrl Pts',(3.4975321651715,-1.80253716195077,58.2013275393903));
#21804=CARTESIAN_POINT('Ctrl Pts',(3.4429081306282,-1.90481468264517,58.1954576996219));
#21805=CARTESIAN_POINT('Ctrl Pts',(3.38380612520998,-2.0045810302882,58.1895878598536));
#21806=CARTESIAN_POINT('Ctrl Pts',(3.3247639414653,-2.10424639675748,58.1837239614003));
#21807=CARTESIAN_POINT('Ctrl Pts',(3.26125301177638,-2.20140529327224,58.1778600629471));
#21808=CARTESIAN_POINT('Ctrl Pts',(3.19351663681391,-2.29563509521715,58.1719961644938));
#21809=CARTESIAN_POINT('Ctrl Pts',(3.12388208013346,-2.39250550625047,58.1659679415569));
#21810=CARTESIAN_POINT('Ctrl Pts',(3.04978194281888,-2.48627982715329,58.1599397186201));
#21811=CARTESIAN_POINT('Ctrl Pts',(2.97152969563647,-2.57652872445671,58.1539114956832));
#21812=CARTESIAN_POINT('Ctrl Pts',(2.8954962623307,-2.66421864725272,58.148054200805));
#21813=CARTESIAN_POINT('Ctrl Pts',(2.8155433064224,-2.7485800521487,58.1421969059269));
#21814=CARTESIAN_POINT('Ctrl Pts',(2.73199993873066,-2.82925172700762,58.1363396110487));
#21815=CARTESIAN_POINT('Ctrl Pts',(2.64846864993749,-2.90991173816414,58.1304831630322));
#21816=CARTESIAN_POINT('Ctrl Pts',(2.56134827829891,-2.98688279362739,58.1246267150157));
#21817=CARTESIAN_POINT('Ctrl Pts',(2.47100464841073,-3.05984068662611,58.1187702669991));
#21818=CARTESIAN_POINT('Ctrl Pts',(2.38065231330698,-3.13280560960786,58.1129132546745));
#21819=CARTESIAN_POINT('Ctrl Pts',(2.28707642349239,-3.20175634222721,58.1070562423499));
#21820=CARTESIAN_POINT('Ctrl Pts',(2.19067515603937,-3.26640955189514,58.1011992300252));
#21821=CARTESIAN_POINT('Ctrl Pts',(2.0893412712699,-3.33437090833333,58.0950425286905));
#21822=CARTESIAN_POINT('Ctrl Pts',(1.984885638255,-3.39758302382534,58.0888858273558));
#21823=CARTESIAN_POINT('Ctrl Pts',(1.87780296866296,-3.4557698145103,58.082729126021));
#21824=CARTESIAN_POINT('Ctrl Pts',(1.77578098223335,-3.51120672126896,58.076863387873));
#21825=CARTESIAN_POINT('Ctrl Pts',(1.67137499028506,-3.56208229837883,58.0709976497249));
#21826=CARTESIAN_POINT('Ctrl Pts',(1.56503492400638,-3.60820657482915,58.0651319115768));
#21827=CARTESIAN_POINT('Ctrl Pts',(1.45862174356419,-3.65436256404784,58.0592621404377));
#21828=CARTESIAN_POINT('Ctrl Pts',(1.35027222518725,-3.69576060091199,58.0533923692985));
#21829=CARTESIAN_POINT('Ctrl Pts',(1.24045289060374,-3.7322601230612,58.0475225981594));
#21830=CARTESIAN_POINT('Ctrl Pts',(1.13047782222282,-3.76881140485009,58.0416445031513));
#21831=CARTESIAN_POINT('Ctrl Pts',(1.01902917364397,-3.80045019873225,58.0357664081432));
#21832=CARTESIAN_POINT('Ctrl Pts',(0.906585108639878,-3.82708667798267,
58.0298883131351));
#21833=CARTESIAN_POINT('Ctrl Pts',(0.890200836386732,-3.83096789063616,
58.0290318134262));
#21834=CARTESIAN_POINT('Ctrl Pts',(0.873795440348021,-3.83474298618914,
58.0281753137173));
#21835=CARTESIAN_POINT('Ctrl Pts',(0.857370408780441,-3.83841177860683,
58.0273188140084));
#21836=CARTESIAN_POINT('Ctrl Pts',(0.744658315171258,-3.86358781998696,
58.0214413290875));
#21837=CARTESIAN_POINT('Ctrl Pts',(0.63065162914066,-3.88383636445048,58.0155638441665));
#21838=CARTESIAN_POINT('Ctrl Pts',(0.515818730214368,-3.89902808883958,
58.0096863592455));
#21839=CARTESIAN_POINT('Ctrl Pts',(0.401132583598046,-3.91420039875192,
58.0038163855387));
#21840=CARTESIAN_POINT('Ctrl Pts',(0.285622729257893,-3.92432868717897,
57.9979464118318));
#21841=CARTESIAN_POINT('Ctrl Pts',(0.169769661463749,-3.92933420085979,
57.9920764381249));
#21842=CARTESIAN_POINT('Ctrl Pts',(0.0540338247757839,-3.93433464948782,
57.9862124042134));
#21843=CARTESIAN_POINT('Ctrl Pts',(-0.0620441248003556,-3.93422261693617,
57.9803483703019));
#21844=CARTESIAN_POINT('Ctrl Pts',(-0.177977267250961,-3.92897099662773,
57.9744843363903));
#21845=CARTESIAN_POINT('Ctrl Pts',(-0.297155467544944,-3.92357237942683,
57.9684561636584));
#21846=CARTESIAN_POINT('Ctrl Pts',(-0.416180194610486,-3.91274213832423,
57.9624279909266));
#21847=CARTESIAN_POINT('Ctrl Pts',(-0.534520622811124,-3.89650827072003,
57.9563998181947));
#21848=CARTESIAN_POINT('Ctrl Pts',(-0.649509225308236,-3.88073420451702,
57.9505423849524));
#21849=CARTESIAN_POINT('Ctrl Pts',(-0.763851336782283,-3.85985856348936,
57.9446849517101));
#21850=CARTESIAN_POINT('Ctrl Pts',(-0.877064594808982,-3.83395966287239,
57.9388275184679));
#21851=CARTESIAN_POINT('Ctrl Pts',(-0.990261500798051,-3.8080645029816,
57.9329709312481));
#21852=CARTESIAN_POINT('Ctrl Pts',(-1.10232947555789,-3.77714761821882,
57.9271143440284));
#21853=CARTESIAN_POINT('Ctrl Pts',(-1.21279709346778,-3.74133829131718,
57.9212577568086));
#21854=CARTESIAN_POINT('Ctrl Pts',(-1.32327536840394,-3.70552550982001,
57.9154006045925));
#21855=CARTESIAN_POINT('Ctrl Pts',(-1.43215258716842,-3.66481947512755,
57.9095434523764));
#21856=CARTESIAN_POINT('Ctrl Pts',(-1.53897388377433,-3.61939889830626,
57.9036863001603));
#21857=CARTESIAN_POINT('Ctrl Pts',(-1.65125477755385,-3.57165689251232,
57.8975297910491));
#21858=CARTESIAN_POINT('Ctrl Pts',(-1.76126356701952,-3.51870587739157,
57.8913732819378));
#21859=CARTESIAN_POINT('Ctrl Pts',(-1.86849879628884,-3.46080933428399,
57.8852167728266));
#21860=CARTESIAN_POINT('Ctrl Pts',(-1.97067176686375,-3.40564591610858,
57.879350894341));
#21861=CARTESIAN_POINT('Ctrl Pts',(-2.0703267274518,-3.34599349803455,57.8734850158554));
#21862=CARTESIAN_POINT('Ctrl Pts',(-2.16705873116568,-3.28212514320807,
57.8676191373699));
#21863=CARTESIAN_POINT('Ctrl Pts',(-2.26385724369535,-3.21821287521447,
57.8617492257555));
#21864=CARTESIAN_POINT('Ctrl Pts',(-2.35772846466131,-3.15007914011432,
57.8558793141411));
#21865=CARTESIAN_POINT('Ctrl Pts',(-2.44829976530984,-3.07803789112217,
57.8500094025267));
#21866=CARTESIAN_POINT('Ctrl Pts',(-2.53899949121711,-3.00589449149317,
57.8441311676917));
#21867=CARTESIAN_POINT('Ctrl Pts',(-2.62638965040602,-2.92983279183208,
57.8382529328567));
#21868=CARTESIAN_POINT('Ctrl Pts',(-2.71013374720078,-2.85020421589112,
57.8323746980217));
#21869=CARTESIAN_POINT('Ctrl Pts',(-2.72232163654136,-2.83861528832415,
57.8315191956229));
#21870=CARTESIAN_POINT('Ctrl Pts',(-2.73443236750762,-2.8269508679733,57.8306636932242));
#21871=CARTESIAN_POINT('Ctrl Pts',(-2.74646497456436,-2.8152120956495,57.8298081908255));
#21872=CARTESIAN_POINT('Ctrl Pts',(-2.82794572414756,-2.73572109560111,
57.8240150176262));
#21873=CARTESIAN_POINT('Ctrl Pts',(-2.90612486115895,-2.65254083708072,
57.8182218444269));
#21874=CARTESIAN_POINT('Ctrl Pts',(-2.98064291111864,-2.56598067732363,
57.8124286712277));
#21875=CARTESIAN_POINT('Ctrl Pts',(-3.05639009447922,-2.47799275632479,
57.8065399428887));
#21876=CARTESIAN_POINT('Ctrl Pts',(-3.12835396610249,-2.38651268154054,
57.8006512145497));
#21877=CARTESIAN_POINT('Ctrl Pts',(-3.19619303340045,-2.29190730467933,
57.7947624862107));
#21878=CARTESIAN_POINT('Ctrl Pts',(-3.26276773572902,-2.19906515554492,
57.788983510292));
#21879=CARTESIAN_POINT('Ctrl Pts',(-3.3253697733291,-2.10321354037534,57.7832045343732));
#21880=CARTESIAN_POINT('Ctrl Pts',(-3.38371523795364,-2.00473444337159,
57.7774255584545));
#21881=CARTESIAN_POINT('Ctrl Pts',(-3.44202433386364,-1.90631673174185,
57.7716501847683));
#21882=CARTESIAN_POINT('Ctrl Pts',(-3.49608191299239,-1.80527515762795,
57.765874811082));
#21883=CARTESIAN_POINT('Ctrl Pts',(-3.54564713371219,-1.70202097613356,
57.7600994373957));
#21884=CARTESIAN_POINT('Ctrl Pts',(-3.59519422532281,-1.59880456116783,
57.7543261761258));
#21885=CARTESIAN_POINT('Ctrl Pts',(-3.64025204133391,-1.49337753088417,
57.7485529148558));
#21886=CARTESIAN_POINT('Ctrl Pts',(-3.68062591401499,-1.3861752706932,57.7427796535858));
#21887=CARTESIAN_POINT('Ctrl Pts',(-3.72239921064247,-1.27525720619475,
57.7368062817113));
#21888=CARTESIAN_POINT('Ctrl Pts',(-3.75915775084489,-1.16243904347894,
57.7308329098368));
#21889=CARTESIAN_POINT('Ctrl Pts',(-3.79074071049323,-1.04822414864825,
57.7248595379623));
#21890=CARTESIAN_POINT('Ctrl Pts',(-3.82127793970969,-0.937790976386587,
57.7190839479556));
#21891=CARTESIAN_POINT('Ctrl Pts',(-3.84697683654312,-0.826052543186788,
57.7133083579489));
#21892=CARTESIAN_POINT('Ctrl Pts',(-3.86774353520111,-0.713476661082976,
57.7075327679422));
#21893=CARTESIAN_POINT('Ctrl Pts',(-3.88957694992897,-0.595118131265251,
57.7014605051338));
#21894=CARTESIAN_POINT('Ctrl Pts',(-3.90595789921607,-0.475834354316848,
57.6953882423254));
#21895=CARTESIAN_POINT('Ctrl Pts',(-3.91683895899895,-0.356176317668844,
57.6893159795169));
#21896=CARTESIAN_POINT('Ctrl Pts',(-3.92772001878182,-0.236518281020859,
57.6832437167085));
#21897=CARTESIAN_POINT('Ctrl Pts',(-3.93310120987238,-0.116486528897887,
57.6771714539001));
#21898=CARTESIAN_POINT('Ctrl Pts',(-3.93299855748857,0.00336850010244591,
57.6710991910917));
#21899=CARTESIAN_POINT('',(-3.93299907365457,-0.00269937629320533,56.4210991910142));
#21900=CARTESIAN_POINT('Ctrl Pts',(-3.93299855748795,0.00336850082684063,
57.671099191055));
#21901=CARTESIAN_POINT('Ctrl Pts',(-3.9328558021228,0.170046994925479,57.6626546924876));
#21902=CARTESIAN_POINT('Ctrl Pts',(-3.92211403768641,0.336283765188421,
57.6542101939203));
#21903=CARTESIAN_POINT('Ctrl Pts',(-3.90096089477367,0.50099211315819,57.6457656953529));
#21904=CARTESIAN_POINT('Ctrl Pts',(-3.88971518144716,0.588556541356485,
57.6412763194495));
#21905=CARTESIAN_POINT('Ctrl Pts',(-3.87552761345545,0.675689581232063,
57.636786943546));
#21906=CARTESIAN_POINT('Ctrl Pts',(-3.858431409569,0.762230973951766,57.6322975676426));
#21907=CARTESIAN_POINT('Ctrl Pts',(-3.8360492483995,0.875530008787236,57.6264201263294));
#21908=CARTESIAN_POINT('Ctrl Pts',(-3.8086358013275,0.988028091084555,57.6205426850162));
#21909=CARTESIAN_POINT('Ctrl Pts',(-3.77626146368769,1.0992444486407,57.614665243703));
#21910=CARTESIAN_POINT('Ctrl Pts',(-3.74392850205911,1.21031866616882,57.6087953140516));
#21911=CARTESIAN_POINT('Ctrl Pts',(-3.70664737336858,1.32011402420501,57.6029253844003));
#21912=CARTESIAN_POINT('Ctrl Pts',(-3.6645396368435,1.42815904226489,57.5970554547489));
#21913=CARTESIAN_POINT('Ctrl Pts',(-3.6224745120357,1.53609472213322,57.5911914652835));
#21914=CARTESIAN_POINT('Ctrl Pts',(-3.57559264416276,1.64228320328672,57.5853274758181));
#21915=CARTESIAN_POINT('Ctrl Pts',(-3.52406544918945,1.74626793758267,57.5794634863526));
#21916=CARTESIAN_POINT('Ctrl Pts',(-3.47109542180087,1.8531643876321,57.5734352971071));
#21917=CARTESIAN_POINT('Ctrl Pts',(-3.41321619063103,1.95773142287339,57.5674071078616));
#21918=CARTESIAN_POINT('Ctrl Pts',(-3.35066730421711,2.05949450507899,57.561378918616));
#21919=CARTESIAN_POINT('Ctrl Pts',(-3.28989066153756,2.15837425881672,57.5555215305027));
#21920=CARTESIAN_POINT('Ctrl Pts',(-3.22470565853247,2.25460644459599,57.5496641423894));
#21921=CARTESIAN_POINT('Ctrl Pts',(-3.15537835721852,2.34778117012575,57.5438067542762));
#21922=CARTESIAN_POINT('Ctrl Pts',(-3.08606107138802,2.44094243501441,57.5379502123601));
#21923=CARTESIAN_POINT('Ctrl Pts',(-3.01260292340981,2.53104678712965,57.5320936704441));
#21924=CARTESIAN_POINT('Ctrl Pts',(-2.93531221328044,2.61771488336044,57.5262371285281));
#21925=CARTESIAN_POINT('Ctrl Pts',(-2.85801404835942,2.70439133884422,57.5203800217409));
#21926=CARTESIAN_POINT('Ctrl Pts',(-2.77688286100864,2.78763057171334,57.5145229149536));
#21927=CARTESIAN_POINT('Ctrl Pts',(-2.69226551450583,2.86708831384782,57.5086658081663));
#21928=CARTESIAN_POINT('Ctrl Pts',(-2.60332180850111,2.95060861256073,57.5025092361908));
#21929=CARTESIAN_POINT('Ctrl Pts',(-2.51052639543604,3.02995015524354,57.4963526642153));
#21930=CARTESIAN_POINT('Ctrl Pts',(-2.4143225195777,3.10476017937941,57.4901960922397));
#21931=CARTESIAN_POINT('Ctrl Pts',(-2.32266178896912,3.17603736450276,57.4843302590777));
#21932=CARTESIAN_POINT('Ctrl Pts',(-2.22790754001856,3.24320104916634,57.4784644259157));
#21933=CARTESIAN_POINT('Ctrl Pts',(-2.1304728699342,3.30599067610216,57.4725985927537));
#21934=CARTESIAN_POINT('Ctrl Pts',(-2.03297120669935,3.36882347529813,57.4667287264211));
#21935=CARTESIAN_POINT('Ctrl Pts',(-1.93278580784402,3.42727602089232,57.4608588600886));
#21936=CARTESIAN_POINT('Ctrl Pts',(-1.83035416860492,3.48113381206047,57.454988993756));
#21937=CARTESIAN_POINT('Ctrl Pts',(-1.72777727987114,3.5350679743285,57.449110803871));
#21938=CARTESIAN_POINT('Ctrl Pts',(-1.62294816661977,3.58439420652273,57.443232613986));
#21939=CARTESIAN_POINT('Ctrl Pts',(-1.51632405508477,3.62894617760739,57.437354424101));
#21940=CARTESIAN_POINT('Ctrl Pts',(-1.5008002719141,3.63543265734436,57.436498597554));
#21941=CARTESIAN_POINT('Ctrl Pts',(-1.48523846411807,3.6418180214223,57.4356427710069));
#21942=CARTESIAN_POINT('Ctrl Pts',(-1.46964006652609,3.64810184546172,57.4347869444598));
#21943=CARTESIAN_POINT('Ctrl Pts',(-1.36251680246636,3.69125651810747,57.4289094860445));
#21944=CARTESIAN_POINT('Ctrl Pts',(-1.2533155386513,3.72975956588389,57.4230320276292));
#21945=CARTESIAN_POINT('Ctrl Pts',(-1.14247741335656,3.76340728063947,57.4171545692138));
#21946=CARTESIAN_POINT('Ctrl Pts',(-1.03178093991715,3.79701199339361,57.4112846222292));
#21947=CARTESIAN_POINT('Ctrl Pts',(-0.919452156525088,3.82577359489109,
57.4054146752445));
#21948=CARTESIAN_POINT('Ctrl Pts',(-0.80595237216699,3.84953630633592,57.3995447282598));
#21949=CARTESIAN_POINT('Ctrl Pts',(-0.692567441683296,3.87327497157228,
57.3936807212525));
#21950=CARTESIAN_POINT('Ctrl Pts',(-0.578014268759466,3.8920247249762,57.3878167142452));
#21951=CARTESIAN_POINT('Ctrl Pts',(-0.46276889460642,3.90567970399324,57.3819527072379));
#21952=CARTESIAN_POINT('Ctrl Pts',(-0.344296973369605,3.91971698410523,
57.3759245244895));
#21953=CARTESIAN_POINT('Ctrl Pts',(-0.225093942451591,3.92836986148459,
57.3698963417412));
#21954=CARTESIAN_POINT('Ctrl Pts',(-0.105688128444879,3.93157971043521,
57.3638681589928));
#21955=CARTESIAN_POINT('Ctrl Pts',(0.0103349531106322,3.93469862528602,
57.3580107529321));
#21956=CARTESIAN_POINT('Ctrl Pts',(0.126549042989509,3.93267875871053,57.3521533468714));
#21957=CARTESIAN_POINT('Ctrl Pts',(0.242465467586941,3.92551900989256,57.3462959408106));
#21958=CARTESIAN_POINT('Ctrl Pts',(0.358365148542804,3.91836029527028,57.3404393808277));
#21959=CARTESIAN_POINT('Ctrl Pts',(0.473966838107189,3.90606320018148,57.3345828208447));
#21960=CARTESIAN_POINT('Ctrl Pts',(0.588784372830718,3.8886786910608,57.3287262608618));
#21961=CARTESIAN_POINT('Ctrl Pts',(0.703612983784414,3.87129250488944,57.3228691359075));
#21962=CARTESIAN_POINT('Ctrl Pts',(0.817656881652661,3.84881799082884,57.3170120109533));
#21963=CARTESIAN_POINT('Ctrl Pts',(0.930438211397646,3.82135757745479,57.3111548859991));
#21964=CARTESIAN_POINT('Ctrl Pts',(1.04898503590869,3.79249336018926,57.3049983389389));
#21965=CARTESIAN_POINT('Ctrl Pts',(1.16613629525132,3.75812010673744,57.2988417918787));
#21966=CARTESIAN_POINT('Ctrl Pts',(1.28135437336183,3.71841632551635,57.2926852448185));
#21967=CARTESIAN_POINT('Ctrl Pts',(1.39113216272645,3.6805872503977,57.2868193934047));
#21968=CARTESIAN_POINT('Ctrl Pts',(1.49915478884817,3.63791974173285,57.2809535419908));
#21969=CARTESIAN_POINT('Ctrl Pts',(1.60497832242048,3.59061743778982,57.2750876905769));
#21970=CARTESIAN_POINT('Ctrl Pts',(1.71087461733806,3.5432826100862,57.2692178059653));
#21971=CARTESIAN_POINT('Ctrl Pts',(1.81456844114516,3.49130682586045,57.2633479213537));
#21972=CARTESIAN_POINT('Ctrl Pts',(1.91564110956707,3.43493932105599,57.257478036742));
#21973=CARTESIAN_POINT('Ctrl Pts',(2.0168570987733,3.37849188727444,57.2515998286491));
#21974=CARTESIAN_POINT('Ctrl Pts',(2.1154441667018,3.31764052242658,57.2457216205561));
#21975=CARTESIAN_POINT('Ctrl Pts',(2.21101319397238,3.25267730586359,57.2398434124632));
#21976=CARTESIAN_POINT('Ctrl Pts',(2.22492527986198,3.2432205406929,57.2389877154011));
#21977=CARTESIAN_POINT('Ctrl Pts',(2.23877346964332,3.23367670964208,57.2381320183389));
#21978=CARTESIAN_POINT('Ctrl Pts',(2.25255662447517,3.22404678215639,57.2372763212768));
#21979=CARTESIAN_POINT('Ctrl Pts',(2.34722781773659,3.15790251132625,57.231398867027));
#21980=CARTESIAN_POINT('Ctrl Pts',(2.4391383294844,3.08747638841646,57.2255214127772));
#21981=CARTESIAN_POINT('Ctrl Pts',(2.527876527007,3.01302659533682,57.2196439585274));
#21982=CARTESIAN_POINT('Ctrl Pts',(2.61650131605382,2.9386719499815,57.2137740157343));
#21983=CARTESIAN_POINT('Ctrl Pts',(2.70196154059394,2.8603041240086,57.2079040729412));
#21984=CARTESIAN_POINT('Ctrl Pts',(2.78387469118082,2.77822437967181,57.2020341301481));
#21985=CARTESIAN_POINT('Ctrl Pts',(2.86570495101809,2.69622769466661,57.1961701273531));
#21986=CARTESIAN_POINT('Ctrl Pts',(2.94399498712891,2.61052685334184,57.1903061245581));
#21987=CARTESIAN_POINT('Ctrl Pts',(3.01839604878882,2.5214627287858,57.1844421217631));
#21988=CARTESIAN_POINT('Ctrl Pts',(3.09488020627214,2.42990496903508,57.1784139374436));
#21989=CARTESIAN_POINT('Ctrl Pts',(3.16725405893758,2.3347930928646,57.172385753124));
#21990=CARTESIAN_POINT('Ctrl Pts',(3.23517985254074,2.23653757440254,57.1663575688045));
#21991=CARTESIAN_POINT('Ctrl Pts',(3.30118126296445,2.1410657005177,57.1605001669799));
#21992=CARTESIAN_POINT('Ctrl Pts',(3.36298301382916,2.04262627764838,57.1546427651554));
#21993=CARTESIAN_POINT('Ctrl Pts',(3.42031719664761,1.94162799586238,57.1487853633309));
#21994=CARTESIAN_POINT('Ctrl Pts',(3.47764309776422,1.84064430288911,57.1429288075855));
#21995=CARTESIAN_POINT('Ctrl Pts',(3.53050251048839,1.73710284463135,57.1370722518401));
#21996=CARTESIAN_POINT('Ctrl Pts',(3.57867250704671,1.63143865569869,57.1312156960947));
#21997=CARTESIAN_POINT('Ctrl Pts',(3.62684715050414,1.52576427347434,57.1253585753747));
#21998=CARTESIAN_POINT('Ctrl Pts',(3.67033130738617,1.41796712884944,57.1195014546547));
#21999=CARTESIAN_POINT('Ctrl Pts',(3.70894969170015,1.30850341399527,57.1136443339347));
#22000=CARTESIAN_POINT('Ctrl Pts',(3.74954235499959,1.19344361023822,57.107487780948));
#22001=CARTESIAN_POINT('Ctrl Pts',(3.78475840837375,1.0765428071426,57.1013312279613));
#22002=CARTESIAN_POINT('Ctrl Pts',(3.81445363598056,0.958348819039591,57.0951746749745));
#22003=CARTESIAN_POINT('Ctrl Pts',(3.84274668712548,0.845735822948172,57.089308827747));
#22004=CARTESIAN_POINT('Ctrl Pts',(3.86602834745813,0.731949401313737,57.0834429805194));
#22005=CARTESIAN_POINT('Ctrl Pts',(3.88422663529618,0.617472627454558,57.0775771332918));
#22006=CARTESIAN_POINT('Ctrl Pts',(3.90243743583728,0.502917142131395,57.0717072528494));
#22007=CARTESIAN_POINT('Ctrl Pts',(3.91555785758935,0.387670768125196,57.065837372407));
#22008=CARTESIAN_POINT('Ctrl Pts',(3.92356790214797,0.272220346840702,57.0599674919646));
#22009=CARTESIAN_POINT('Ctrl Pts',(3.93158930500471,0.156606216067098,57.0540892879914));
#22010=CARTESIAN_POINT('Ctrl Pts',(3.93448586071822,0.0407878711960379,
57.0482110840183));
#22011=CARTESIAN_POINT('Ctrl Pts',(3.93228960745753,-0.0747492012093419,
57.0423328800452));
#22012=CARTESIAN_POINT('Ctrl Pts',(3.93196988498466,-0.0915686633171382,
57.0414771527281));
#22013=CARTESIAN_POINT('Ctrl Pts',(3.93154232262271,-0.108382176773632,
57.0406214254111));
#22014=CARTESIAN_POINT('Ctrl Pts',(3.9310071101537,-0.125188257919694,57.039765698094));
#22015=CARTESIAN_POINT('Ctrl Pts',(3.92733107263806,-0.240618649326302,
57.033888245862));
#22016=CARTESIAN_POINT('Ctrl Pts',(3.9185604458126,-0.356076202066446,57.02801079363));
#22017=CARTESIAN_POINT('Ctrl Pts',(3.90468657600241,-0.471075092937918,
57.022133341398));
#22018=CARTESIAN_POINT('Ctrl Pts',(3.8908304372731,-0.585927012945289,57.0162634006666));
#22019=CARTESIAN_POINT('Ctrl Pts',(3.87188407528563,-0.700321030955226,
57.0103934599351));
#22020=CARTESIAN_POINT('Ctrl Pts',(3.84789083010248,-0.813772179183578,
57.0045235192037));
#22021=CARTESIAN_POINT('Ctrl Pts',(3.82392186469027,-0.92710852143751,56.9986595185114));
#22022=CARTESIAN_POINT('Ctrl Pts',(3.79491625992438,-1.03950349058538,56.9927955178191));
#22023=CARTESIAN_POINT('Ctrl Pts',(3.76096897627802,-1.1504787522915,56.9869315171268));
#22024=CARTESIAN_POINT('Ctrl Pts',(3.72607121279863,-1.26456117713076,56.9809033320345));
#22025=CARTESIAN_POINT('Ctrl Pts',(3.68595100804219,-1.37714277801046,56.9748751469422));
#22026=CARTESIAN_POINT('Ctrl Pts',(3.64076762548157,-1.48771640350074,56.9688469618499));
#22027=CARTESIAN_POINT('Ctrl Pts',(3.59686434043458,-1.59515735022638,56.962989562217));
#22028=CARTESIAN_POINT('Ctrl Pts',(3.54818108370429,-1.70070216370797,56.9571321625841));
#22029=CARTESIAN_POINT('Ctrl Pts',(3.49491378453669,-1.80390316776022,56.9512747629511));
#22030=CARTESIAN_POINT('Ctrl Pts',(3.44165417989455,-1.90708926430326,56.9454182094267));
#22031=CARTESIAN_POINT('Ctrl Pts',(3.38381203870854,-2.00793185820569,56.9395616559022));
#22032=CARTESIAN_POINT('Ctrl Pts',(3.32162993049593,-2.10600655384391,56.9337051023777));
#22033=CARTESIAN_POINT('Ctrl Pts',(3.25944182393749,-2.20409071017684,56.9278479839056));
#22034=CARTESIAN_POINT('Ctrl Pts',(3.19291313900253,-2.29940608907504,56.9219908654335));
#22035=CARTESIAN_POINT('Ctrl Pts',(3.12233019496086,-2.39155663818268,56.9161337469614));
#22036=CARTESIAN_POINT('Ctrl Pts',(3.04813879009114,-2.48841826375861,56.9099771909572));
#22037=CARTESIAN_POINT('Ctrl Pts',(2.96946792831302,-2.58178249751481,56.903820634953));
#22038=CARTESIAN_POINT('Ctrl Pts',(2.88669764384709,-2.67122925130128,56.8976640789488));
#22039=CARTESIAN_POINT('Ctrl Pts',(2.807835752015,-2.75645235120187,56.8917982340167));
#22040=CARTESIAN_POINT('Ctrl Pts',(2.72525307953862,-2.8381192281285,56.8859323890847));
#22041=CARTESIAN_POINT('Ctrl Pts',(2.63931490051718,-2.91590566649677,56.8800665441526));
#22042=CARTESIAN_POINT('Ctrl Pts',(2.55331763269417,-2.99374558874696,56.8741966660219));
#22043=CARTESIAN_POINT('Ctrl Pts',(2.46396058114437,-3.06769949738339,56.8683267878912));
#22044=CARTESIAN_POINT('Ctrl Pts',(2.37164057700697,-3.137484657093,56.8624569097604));
#22045=CARTESIAN_POINT('Ctrl Pts',(2.27918966256364,-3.20736877256733,56.8565787081082));
#22046=CARTESIAN_POINT('Ctrl Pts',(2.18376775017054,-3.27307211086288,56.850700506456));
#22047=CARTESIAN_POINT('Ctrl Pts',(2.08579896637717,-3.33435626048865,56.8448223048037));
#22048=CARTESIAN_POINT('Ctrl Pts',(2.07153675914799,-3.34327795174564,56.8439665615062));
#22049=CARTESIAN_POINT('Ctrl Pts',(2.05722061393766,-3.35210606738391,56.8431108182086));
#22050=CARTESIAN_POINT('Ctrl Pts',(2.04285187715921,-3.36083995572342,56.8422550749111));
#22051=CARTESIAN_POINT('Ctrl Pts',(1.94416387664794,-3.42082643819612,56.8363776205261));
#22052=CARTESIAN_POINT('Ctrl Pts',(1.84266969904448,-3.47656074588849,56.8305001661411));
#22053=CARTESIAN_POINT('Ctrl Pts',(1.73877152162544,-3.52777020164073,56.8246227117562));
#22054=CARTESIAN_POINT('Ctrl Pts',(1.63500612754906,-3.57891421098305,56.8187527688412));
#22055=CARTESIAN_POINT('Ctrl Pts',(1.52884321051815,-3.6255446882666,56.8128828259262));
#22056=CARTESIAN_POINT('Ctrl Pts',(1.42071263806928,-3.6674329714434,56.8070128830112));
#22057=CARTESIAN_POINT('Ctrl Pts',(1.31269148692994,-3.7092788663234,56.8011488801076));
#22058=CARTESIAN_POINT('Ctrl Pts',(1.20270702352047,-3.7463919645691,56.7952848772041));
#22059=CARTESIAN_POINT('Ctrl Pts',(1.09121176224109,-3.77859046338005,56.7894208743005));
#22060=CARTESIAN_POINT('Ctrl Pts',(0.976594837299304,-3.81169046134503,
56.7833926900267));
#22061=CARTESIAN_POINT('Ctrl Pts',(0.860381661439289,-3.83959639243075,
56.7773645057528));
#22062=CARTESIAN_POINT('Ctrl Pts',(0.74308401614705,-3.86216456730507,56.771336321479));
#22063=CARTESIAN_POINT('Ctrl Pts',(0.629109489314705,-3.88409337113026,
56.7654789195801));
#22064=CARTESIAN_POINT('Ctrl Pts',(0.514111547251461,-3.90098271963304,
56.7596215176812));
#22065=CARTESIAN_POINT('Ctrl Pts',(0.398572190586897,-3.91275212719778,
56.7537641157823));
#22066=CARTESIAN_POINT('Ctrl Pts',(0.283049523391554,-3.92451983469104,
56.7479075599755));
#22067=CARTESIAN_POINT('Ctrl Pts',(0.166986007382457,-3.93116903010421,
56.7420510041686));
#22068=CARTESIAN_POINT('Ctrl Pts',(0.05086962625867,-3.93267101104635,56.7361944483618));
#22069=CARTESIAN_POINT('Ctrl Pts',(-0.0652579562082603,-3.93417313687936,
56.7303373275933));
#22070=CARTESIAN_POINT('Ctrl Pts',(-0.181438001445452,-3.93052705584168,
56.7244802068249));
#22071=CARTESIAN_POINT('Ctrl Pts',(-0.297182362219594,-3.92175619379706,
56.7186230860565));
#22072=CARTESIAN_POINT('Ctrl Pts',(-0.418843892450566,-3.9125369412075,
56.7124665331958));
#22073=CARTESIAN_POINT('Ctrl Pts',(-0.540023505878393,-3.89765509485266,
56.7063099803351));
#22074=CARTESIAN_POINT('Ctrl Pts',(-0.660161724269143,-3.87719944003529,
56.7001534274744));
#22075=CARTESIAN_POINT('Ctrl Pts',(-0.774627148834287,-3.85770967861889,
56.694287580232));
#22076=CARTESIAN_POINT('Ctrl Pts',(-0.888146879067335,-3.83316060599723,
56.6884217329896));
#22077=CARTESIAN_POINT('Ctrl Pts',(-1.00024979820838,-3.80368102516288,
56.6825558857472));
#22078=CARTESIAN_POINT('Ctrl Pts',(-1.11242979638612,-3.77418117493937,
56.6766860053015));
#22079=CARTESIAN_POINT('Ctrl Pts',(-1.22319065087741,-3.73974418817955,
56.6708161248559));
#22080=CARTESIAN_POINT('Ctrl Pts',(-1.33207874584417,-3.70054796143358,
56.6649462444102));
#22081=CARTESIAN_POINT('Ctrl Pts',(-1.44112124456879,-3.66129615427999,
56.6590680404504));
#22082=CARTESIAN_POINT('Ctrl Pts',(-1.54828530500223,-3.61727179706604,
56.6531898364907));
#22083=CARTESIAN_POINT('Ctrl Pts',(-1.65313952220212,-3.56869986411486,
56.6473116325309));
#22084=CARTESIAN_POINT('Ctrl Pts',(-1.66840380674172,-3.56162894388862,
56.6464559055966));
#22085=CARTESIAN_POINT('Ctrl Pts',(-1.68361918720646,-3.55446172620473,
56.6456001786624));
#22086=CARTESIAN_POINT('Ctrl Pts',(-1.6987843822387,-3.54719898267096,56.6447444517282));
#22087=CARTESIAN_POINT('Ctrl Pts',(-1.80294463275982,-3.49731573459276,
56.6388669980155));
#22088=CARTESIAN_POINT('Ctrl Pts',(-1.90507659828325,-3.44275897953083,
56.6329895443029));
#22089=CARTESIAN_POINT('Ctrl Pts',(-2.00473216674064,-3.38371658677783,
56.6271120905902));
#22090=CARTESIAN_POINT('Ctrl Pts',(-2.10426037385781,-3.32474965110553,
56.6212421483532));
#22091=CARTESIAN_POINT('Ctrl Pts',(-2.20131812632969,-3.26130868710462,
56.6153722061163));
#22092=CARTESIAN_POINT('Ctrl Pts',(-2.29547904868907,-3.19362880388902,
56.6095022638793));
#22093=CARTESIAN_POINT('Ctrl Pts',(-2.38954468605381,-3.12601740850412,
56.6036382616587));
#22094=CARTESIAN_POINT('Ctrl Pts',(-2.48071899135305,-3.05417586585131,
56.597774259438));
#22095=CARTESIAN_POINT('Ctrl Pts',(-2.56860246330661,-2.97838385462574,
56.5919102572174));
#22096=CARTESIAN_POINT('Ctrl Pts',(-2.65894652627984,-2.90046979316662,
56.5858820726894));
#22097=CARTESIAN_POINT('Ctrl Pts',(-2.74581237212719,-2.81838100309495,
56.5798538881614));
#22098=CARTESIAN_POINT('Ctrl Pts',(-2.8288000410369,-2.73246762612655,56.5738257036334));
#22099=CARTESIAN_POINT('Ctrl Pts',(-2.90943660249154,-2.64898824427737,
56.567968302425));
#22100=CARTESIAN_POINT('Ctrl Pts',(-2.98641147531313,-2.5618983896874,56.5621109012166));
#22101=CARTESIAN_POINT('Ctrl Pts',(-3.05939390736504,-2.47155779207724,
56.5562535000082));
#22102=CARTESIAN_POINT('Ctrl Pts',(-3.13236579720378,-2.38123024404369,
56.5503969448935));
#22103=CARTESIAN_POINT('Ctrl Pts',(-3.20134613390724,-2.28765320752724,
56.5445403897788));
#22104=CARTESIAN_POINT('Ctrl Pts',(-3.26604426790166,-2.1912197151602,56.538683834664));
#22105=CARTESIAN_POINT('Ctrl Pts',(-3.3307486430911,-2.09477692020289,56.5328267145886));
#22106=CARTESIAN_POINT('Ctrl Pts',(-3.39116976456058,-1.99547746418522,
56.5269695945132));
#22107=CARTESIAN_POINT('Ctrl Pts',(-3.44706055378369,-1.89374299696357,
56.5211124744378));
#22108=CARTESIAN_POINT('Ctrl Pts',(-3.50580864972638,-1.78680755511183,
56.5149559206134));
#22109=CARTESIAN_POINT('Ctrl Pts',(-3.55955070280624,-1.67718198904026,
56.508799366789));
#22110=CARTESIAN_POINT('Ctrl Pts',(-3.60805540492265,-1.56538340192061,
56.5026428129647));
#22111=CARTESIAN_POINT('Ctrl Pts',(-3.65426975598089,-1.45886384963962,
56.4967769664109));
#22112=CARTESIAN_POINT('Ctrl Pts',(-3.6957299657723,-1.35037221803497,56.4909111198572));
#22113=CARTESIAN_POINT('Ctrl Pts',(-3.73228651975144,-1.24037346572788,
56.4850452733035));
#22114=CARTESIAN_POINT('Ctrl Pts',(-3.76886820907414,-1.13029908111604,
56.479175393545));
#22115=CARTESIAN_POINT('Ctrl Pts',(-3.80053941657034,-1.01871590810039,
56.4733055137865));
#22116=CARTESIAN_POINT('Ctrl Pts',(-3.8272013079809,-0.906101069522241,
56.467435634028));
#22117=CARTESIAN_POINT('Ctrl Pts',(-3.85390100609433,-0.793326542508052,
56.461557430749));
#22118=CARTESIAN_POINT('Ctrl Pts',(-3.8755771375722,-0.679517834267319,
56.45567922747));
#22119=CARTESIAN_POINT('Ctrl Pts',(-3.89218243339884,-0.565159185665073,
56.449801024191));
#22120=CARTESIAN_POINT('Ctrl Pts',(-3.89459978447921,-0.548511183387055,
56.4489452923091));
#22121=CARTESIAN_POINT('Ctrl Pts',(-3.89690976096515,-0.531851528853973,
56.4480895604272));
#22122=CARTESIAN_POINT('Ctrl Pts',(-3.89911230905229,-0.515181716869908,
56.4472338285453));
#22123=CARTESIAN_POINT('Ctrl Pts',(-3.9215347511864,-0.345479226930439,
56.4385222827152));
#22124=CARTESIAN_POINT('Ctrl Pts',(-3.93288130956813,-0.17428194010258,
56.4298107368851));
#22125=CARTESIAN_POINT('Ctrl Pts',(-3.93299907365402,-0.00269937709636038,
56.421099191055));
#22126=CARTESIAN_POINT('',(-3.93299991625273,-0.000811637929910356,55.1710991910932));
#22127=CARTESIAN_POINT('Ctrl Pts',(-3.93299907365457,-0.00269937629318175,
56.4210991910142));
#22128=CARTESIAN_POINT('Ctrl Pts',(-3.93307733299134,0.111324703940528,
56.4153099896917));
#22129=CARTESIAN_POINT('Ctrl Pts',(-3.92819278913474,0.22553690514298,56.4095207883691));
#22130=CARTESIAN_POINT('Ctrl Pts',(-3.91832287188957,0.339462621840942,
56.4037315870465));
#22131=CARTESIAN_POINT('Ctrl Pts',(-3.90846364095589,0.453264989409994,
56.3979486537814));
#22132=CARTESIAN_POINT('Ctrl Pts',(-3.8936298028039,0.566781068380818,56.3921657205164));
#22133=CARTESIAN_POINT('Ctrl Pts',(-3.87385082285357,0.679535725533855,
56.3863827872513));
#22134=CARTESIAN_POINT('Ctrl Pts',(-3.85408757408983,0.792200703413459,
56.3806044534348));
#22135=CARTESIAN_POINT('Ctrl Pts',(-3.82938707706054,0.904105046395576,
56.3748261196184));
#22136=CARTESIAN_POINT('Ctrl Pts',(-3.79983058608534,1.01477904838956,56.3690477858019));
#22137=CARTESIAN_POINT('Ctrl Pts',(-3.77028658968899,1.12540626455076,56.3632718946925));
#22138=CARTESIAN_POINT('Ctrl Pts',(-3.73589078724557,1.23480376284223,56.357496003583));
#22139=CARTESIAN_POINT('Ctrl Pts',(-3.69677531831842,1.34251303378098,56.3517201124736));
#22140=CARTESIAN_POINT('Ctrl Pts',(-3.65766632269399,1.45020447968183,56.3459451772287));
#22141=CARTESIAN_POINT('Ctrl Pts',(-3.61383935817217,1.55620785387354,56.3401702419838));
#22142=CARTESIAN_POINT('Ctrl Pts',(-3.56547584208702,1.6600816303706,56.334395306739));
#22143=CARTESIAN_POINT('Ctrl Pts',(-3.5171078883149,1.76396493800482,56.3286198416039));
#22144=CARTESIAN_POINT('Ctrl Pts',(-3.46420273621944,1.86571787446573,56.3228443764688));
#22145=CARTESIAN_POINT('Ctrl Pts',(-3.40698879950162,1.96492145391886,56.3170689113337));
#22146=CARTESIAN_POINT('Ctrl Pts',(-3.34971954438805,2.06422095026187,56.311287862079));
#22147=CARTESIAN_POINT('Ctrl Pts',(-3.28813339752779,2.16096579784075,56.3055068128243));
#22148=CARTESIAN_POINT('Ctrl Pts',(-3.2225033644604,2.2547640821251,56.2997257635696));
#22149=CARTESIAN_POINT('Ctrl Pts',(-3.15684142882249,2.34860796148597,56.2939419041634));
#22150=CARTESIAN_POINT('Ctrl Pts',(-3.08713195244681,2.43950208873545,56.2881580447573));
#22151=CARTESIAN_POINT('Ctrl Pts',(-3.01368847512405,2.52708740943097,56.2823741853511));
#22152=CARTESIAN_POINT('Ctrl Pts',(-2.94012722295438,2.61481318300418,56.2765810508782));
#22153=CARTESIAN_POINT('Ctrl Pts',(-2.86282029676006,2.69921923792204,56.2707879164053));
#22154=CARTESIAN_POINT('Ctrl Pts',(-2.78211857535195,2.77998295546604,56.2649947819324));
#22155=CARTESIAN_POINT('Ctrl Pts',(-2.71120460390429,2.85095140396986,56.2599042564091));
#22156=CARTESIAN_POINT('Ctrl Pts',(-2.63767004399989,2.91910790852508,56.2548137308858));
#22157=CARTESIAN_POINT('Ctrl Pts',(-2.56177270149997,2.98426031469267,56.2497232053624));
#22158=CARTESIAN_POINT('Ctrl Pts',(-2.4741426282765,3.05948442577611,56.2438457515589));
#22159=CARTESIAN_POINT('Ctrl Pts',(-2.38305277740475,3.1309688112403,56.2379682977553));
#22160=CARTESIAN_POINT('Ctrl Pts',(-2.28885567755934,3.19837907185881,56.2320908439518));
#22161=CARTESIAN_POINT('Ctrl Pts',(-2.19477896305574,3.26570318112787,56.2262209016246));
#22162=CARTESIAN_POINT('Ctrl Pts',(-2.09760322962568,3.32896328266626,56.2203509592973));
#22163=CARTESIAN_POINT('Ctrl Pts',(-1.99771547979881,3.3878639083901,56.2144810169701));
#22164=CARTESIAN_POINT('Ctrl Pts',(-1.89792881017084,3.44670493033897,56.2086170146599));
#22165=CARTESIAN_POINT('Ctrl Pts',(-1.79543593648024,3.50119504340813,56.2027530123498));
#22166=CARTESIAN_POINT('Ctrl Pts',(-1.69065382084452,3.55108133644723,56.1968890100396));
#22167=CARTESIAN_POINT('Ctrl Pts',(-1.58293798252598,3.6023643616344,56.1908608255455));
#22168=CARTESIAN_POINT('Ctrl Pts',(-1.472803176436,3.64878169596722,56.1848326410513));
#22169=CARTESIAN_POINT('Ctrl Pts',(-1.36073103707832,3.69010840555285,56.1788044565571));
#22170=CARTESIAN_POINT('Ctrl Pts',(-1.2518339894023,3.73026429701554,56.1729470552616));
#22171=CARTESIAN_POINT('Ctrl Pts',(-1.14110831956745,3.76561398212311,56.1670896539662));
#22172=CARTESIAN_POINT('Ctrl Pts',(-1.02901654604823,3.79599972971008,56.1612322526707));
#22173=CARTESIAN_POINT('Ctrl Pts',(-0.916940964053141,3.82638108811174,
56.1553756974699));
#22174=CARTESIAN_POINT('Ctrl Pts',(-0.803500068803967,3.85179982693971,
56.1495191422691));
#22175=CARTESIAN_POINT('Ctrl Pts',(-0.689170696037995,3.87214833803181,
56.1436625870683));
#22176=CARTESIAN_POINT('Ctrl Pts',(-0.574830294353475,3.89249881206717,
56.137805466908));
#22177=CARTESIAN_POINT('Ctrl Pts',(-0.459601650906687,3.90777801378501,
56.1319483467476));
#22178=CARTESIAN_POINT('Ctrl Pts',(-0.34397023255161,3.91792974402533,56.1260912265873));
#22179=CARTESIAN_POINT('Ctrl Pts',(-0.222427389465489,3.92860046114706,
56.1199346728867));
#22180=CARTESIAN_POINT('Ctrl Pts',(-0.10044000590948,3.93360552608599,56.113778119186));
#22181=CARTESIAN_POINT('Ctrl Pts',(0.0214254481688518,3.93294164082952,
56.1076215654854));
#22182=CARTESIAN_POINT('Ctrl Pts',(0.137536522395278,3.93230910365255,56.1017557188505));
#22183=CARTESIAN_POINT('Ctrl Pts',(0.253536501168739,3.92653082887976,56.0958898722156));
#22184=CARTESIAN_POINT('Ctrl Pts',(0.368939600224272,3.9156573613362,56.0900240255807));
#22185=CARTESIAN_POINT('Ctrl Pts',(0.484422047447499,3.90477641747932,56.0841541457424));
#22186=CARTESIAN_POINT('Ctrl Pts',(0.59930639031804,3.88879336160765,56.078284265904));
#22187=CARTESIAN_POINT('Ctrl Pts',(0.713116136264978,3.86781002328171,56.0724143860656));
#22188=CARTESIAN_POINT('Ctrl Pts',(0.827087264985156,3.84679693047998,56.0665361827091));
#22189=CARTESIAN_POINT('Ctrl Pts',(0.939980356082507,3.82076949932781,56.0606579793525));
#22190=CARTESIAN_POINT('Ctrl Pts',(1.05133318359121,3.78987962039429,56.054779775996));
#22191=CARTESIAN_POINT('Ctrl Pts',(1.06754359533752,3.78538276416253,56.0539240447239));
#22192=CARTESIAN_POINT('Ctrl Pts',(1.08372139884249,3.78078294314022,56.0530683134517));
#22193=CARTESIAN_POINT('Ctrl Pts',(1.09986520438379,3.77608071049677,56.0522125821796));
#22194=CARTESIAN_POINT('Ctrl Pts',(1.21074635684578,3.74378417587136,56.0463351284772));
#22195=CARTESIAN_POINT('Ctrl Pts',(1.32038552345773,3.70654668199652,56.0404576747747));
#22196=CARTESIAN_POINT('Ctrl Pts',(1.42831002183767,3.66448079289796,56.0345802210723));
#22197=CARTESIAN_POINT('Ctrl Pts',(1.53609659102824,3.62246866466065,56.0287102788472));
#22198=CARTESIAN_POINT('Ctrl Pts',(1.6421724691666,3.5756405618185,56.0228403366221));
#22199=CARTESIAN_POINT('Ctrl Pts',(1.74607874615064,3.52415919223876,56.016970394397));
#22200=CARTESIAN_POINT('Ctrl Pts',(1.84987987641872,3.47272991861609,56.0111063921898));
#22201=CARTESIAN_POINT('Ctrl Pts',(1.9515154052644,3.41665692696112,56.0052423899826));
#22202=CARTESIAN_POINT('Ctrl Pts',(2.05054569804127,3.35615126897528,55.9993783877755));
#22203=CARTESIAN_POINT('Ctrl Pts',(2.15234867458703,3.29395155302879,55.993350203243));
#22204=CARTESIAN_POINT('Ctrl Pts',(2.25139795879813,3.22706744470576,55.9873220187106));
#22205=CARTESIAN_POINT('Ctrl Pts',(2.34724201481534,3.15577944791545,55.9812938341781));
#22206=CARTESIAN_POINT('Ctrl Pts',(2.44037073123758,3.08651109770913,55.9754364329872));
#22207=CARTESIAN_POINT('Ctrl Pts',(2.53047304201592,3.01308530289735,55.9695790317962));
#22208=CARTESIAN_POINT('Ctrl Pts',(2.6171641414872,2.93580327278813,55.9637216306052));
#22209=CARTESIAN_POINT('Ctrl Pts',(2.70384271852548,2.8585324059823,55.9578650755093));
#22210=CARTESIAN_POINT('Ctrl Pts',(2.7871107562618,2.77740668596996,55.9520085204134));
#22211=CARTESIAN_POINT('Ctrl Pts',(2.86661760768431,2.69276669827043,55.9461519653175));
#22212=CARTESIAN_POINT('Ctrl Pts',(2.94613212882622,2.60811854567763,55.9402948452624));
#22213=CARTESIAN_POINT('Ctrl Pts',(3.02188445995336,2.51995575214908,55.9344377252072));
#22214=CARTESIAN_POINT('Ctrl Pts',(3.09356229642685,2.42865421954755,55.928580605152));
#22215=CARTESIAN_POINT('Ctrl Pts',(3.16890452190235,2.33268507491432,55.9224240513057));
#22216=CARTESIAN_POINT('Ctrl Pts',(3.23974431383181,2.23324817505333,55.9162674974595));
#22217=CARTESIAN_POINT('Ctrl Pts',(3.30576941926725,2.13081616913271,55.9101109436132));
#22218=CARTESIAN_POINT('Ctrl Pts',(3.36867687452289,2.03322091674044,55.9042450970832));
#22219=CARTESIAN_POINT('Ctrl Pts',(3.42721378332237,1.93290734142136,55.8983792505531));
#22220=CARTESIAN_POINT('Ctrl Pts',(3.48115707180607,1.83030993042558,55.8925134040231));
#22221=CARTESIAN_POINT('Ctrl Pts',(3.53513745029254,1.72764197611729,55.8866435242895));
#22222=CARTESIAN_POINT('Ctrl Pts',(3.58451774412173,1.62268743150759,55.8807736445559));
#22223=CARTESIAN_POINT('Ctrl Pts',(3.62912290984797,1.51590102091677,55.8749037648223));
#22224=CARTESIAN_POINT('Ctrl Pts',(3.67379132592364,1.40896318665845,55.8690255615697));
#22225=CARTESIAN_POINT('Ctrl Pts',(3.71367096145326,1.30018868876741,55.863147358317));
#22226=CARTESIAN_POINT('Ctrl Pts',(3.74863649650455,1.19004765327864,55.8572691550644));
#22227=CARTESIAN_POINT('Ctrl Pts',(3.75372667912401,1.17401363624696,55.8564134230419));
#22228=CARTESIAN_POINT('Ctrl Pts',(3.75871280715739,1.15795067565749,55.8555576910193));
#22229=CARTESIAN_POINT('Ctrl Pts',(3.7635945846407,1.14186023770998,55.8547019589967));
#22230=CARTESIAN_POINT('Ctrl Pts',(3.7971242648828,1.03134572917699,55.8488245053053));
#22231=CARTESIAN_POINT('Ctrl Pts',(3.825837050582,0.919171963622134,55.8429470516138));
#22232=CARTESIAN_POINT('Ctrl Pts',(3.84956897070611,0.805796338895009,55.8370695979224));
#22233=CARTESIAN_POINT('Ctrl Pts',(3.873270561065,0.692565609990109,55.8311996557087));
#22234=CARTESIAN_POINT('Ctrl Pts',(3.89200386175915,0.578136476797947,55.8253297134951));
#22235=CARTESIAN_POINT('Ctrl Pts',(3.90565442457242,0.462982198165142,55.8194597712814));
#22236=CARTESIAN_POINT('Ctrl Pts',(3.9192911738607,0.347944448537503,55.8135957690861));
#22237=CARTESIAN_POINT('Ctrl Pts',(3.92785536810784,0.232183420396551,55.8077317668907));
#22238=CARTESIAN_POINT('Ctrl Pts',(3.9312835809627,0.116182640927894,55.8018677646954));
#22239=CARTESIAN_POINT('Ctrl Pts',(3.93480777809496,-0.00306596808511381,
55.7958395801587));
#22240=CARTESIAN_POINT('Ctrl Pts',(3.93290404981569,-0.122567518241643,
55.7898113956219));
#22241=CARTESIAN_POINT('Ctrl Pts',(3.92556063774814,-0.241790569217127,
55.7837832110852));
#22242=CARTESIAN_POINT('Ctrl Pts',(3.91842527050216,-0.357635934432931,
55.7779258099071));
#22243=CARTESIAN_POINT('Ctrl Pts',(3.90615432996575,-0.473217930074345,
55.7720684087289));
#22244=CARTESIAN_POINT('Ctrl Pts',(3.88878985773621,-0.588049693791152,
55.7662110075508));
#22245=CARTESIAN_POINT('Ctrl Pts',(3.87142789378636,-0.70286487018093,55.760354452468));
#22246=CARTESIAN_POINT('Ctrl Pts',(3.84897392287386,-0.81692962238403,55.7544978973853));
#22247=CARTESIAN_POINT('Ctrl Pts',(3.82152162899223,-0.929764184696576,
55.7486413423026));
#22248=CARTESIAN_POINT('Ctrl Pts',(3.79406668689527,-1.04260963171762,55.7427842222609));
#22249=CARTESIAN_POINT('Ctrl Pts',(3.76161256084109,-1.15422425211548,55.7369271022192));
#22250=CARTESIAN_POINT('Ctrl Pts',(3.72430346262254,-1.26414109904617,55.7310699821776));
#22251=CARTESIAN_POINT('Ctrl Pts',(3.6850870096299,-1.37967723008603,55.7249134283139));
#22252=CARTESIAN_POINT('Ctrl Pts',(3.64050621031212,-1.49333692218658,55.7187568744503));
#22253=CARTESIAN_POINT('Ctrl Pts',(3.59078633611034,-1.60460041393589,55.7126003205866));
#22254=CARTESIAN_POINT('Ctrl Pts',(3.54341419297414,-1.71061013623707,55.7067344740708));
#22255=CARTESIAN_POINT('Ctrl Pts',(3.49137745245901,-1.81444443054335,55.700868627555));
#22256=CARTESIAN_POINT('Ctrl Pts',(3.43491814617481,-1.91567907778911,55.6950027810391));
#22257=CARTESIAN_POINT('Ctrl Pts',(3.37842001994147,-2.01698333134276,55.6891329013199));
#22258=CARTESIAN_POINT('Ctrl Pts',(3.31749348899304,-2.11568402856839,55.6832630216008));
#22259=CARTESIAN_POINT('Ctrl Pts',(3.25242377604221,-2.21138612210425,55.6773931418816));
#22260=CARTESIAN_POINT('Ctrl Pts',(3.18726179391393,-2.30722392168598,55.6715149386437));
#22261=CARTESIAN_POINT('Ctrl Pts',(3.1179451524688,-2.40005430407117,55.6656367354058));
#22262=CARTESIAN_POINT('Ctrl Pts',(3.04479914065971,-2.48951545346435,55.6597585321679));
#22263=CARTESIAN_POINT('Ctrl Pts',(3.03415075218513,-2.50253895329107,55.6589028000499));
#22264=CARTESIAN_POINT('Ctrl Pts',(3.02342127162262,-2.51549111473446,55.6580470679318));
#22265=CARTESIAN_POINT('Ctrl Pts',(3.0126117652989,-2.5283708888497,55.6571913358138));
#22266=CARTESIAN_POINT('Ctrl Pts',(2.93836846900302,-2.61683347513477,55.6513138820907));
#22267=CARTESIAN_POINT('Ctrl Pts',(2.86010374146197,-2.7021681710333,55.6454364283676));
#22268=CARTESIAN_POINT('Ctrl Pts',(2.77811109404059,-2.78398774228058,55.6395589746444));
#22269=CARTESIAN_POINT('Ctrl Pts',(2.6962232344979,-2.86570274684322,55.6336890323986));
#22270=CARTESIAN_POINT('Ctrl Pts',(2.61061721958203,-2.94391127222344,55.6278190901527));
#22271=CARTESIAN_POINT('Ctrl Pts',(2.52162690192179,-3.01825889669926,55.6219491479068));
#22272=CARTESIAN_POINT('Ctrl Pts',(2.4327266369501,-3.09253128598494,55.6160851456789));
#22273=CARTESIAN_POINT('Ctrl Pts',(2.34044919628267,-3.16295028308159,55.610221143451));
#22274=CARTESIAN_POINT('Ctrl Pts',(2.24516490864606,-3.22919858989568,55.604357141223));
#22275=CARTESIAN_POINT('Ctrl Pts',(2.14721281963813,-3.29730173897339,55.5983289566983));
#22276=CARTESIAN_POINT('Ctrl Pts',(2.04608333297791,-3.36099688426316,55.5923007721737));
#22277=CARTESIAN_POINT('Ctrl Pts',(1.94221513615544,-3.41998382523787,55.586272587649));
#22278=CARTESIAN_POINT('Ctrl Pts',(1.84128960883708,-3.47729961876171,55.5804151864373));
#22279=CARTESIAN_POINT('Ctrl Pts',(1.73777885005964,-3.5301701838976,55.5745577852256));
#22280=CARTESIAN_POINT('Ctrl Pts',(1.63211360431378,-3.5783647358275,55.5687003840139));
#22281=CARTESIAN_POINT('Ctrl Pts',(1.52646362179604,-3.62655232610758,55.5628438288974));
#22282=CARTESIAN_POINT('Ctrl Pts',(1.41866014637608,-3.67006507518796,55.5569872737808));
#22283=CARTESIAN_POINT('Ctrl Pts',(1.3091561935006,-3.70871932896236,55.5511307186643));
#22284=CARTESIAN_POINT('Ctrl Pts',(1.19964167720273,-3.74737731156297,55.5452735985885));
#22285=CARTESIAN_POINT('Ctrl Pts',(1.08842674634867,-3.78117572985175,55.5394164785128));
#22286=CARTESIAN_POINT('Ctrl Pts',(0.975981285700459,-3.80998025322474,
55.533559358437));
#22287=CARTESIAN_POINT('Ctrl Pts',(0.857787272085699,-3.84025735118928,
55.5274028046198));
#22288=CARTESIAN_POINT('Ctrl Pts',(0.738234074887739,-3.86501631056285,
55.5212462508027));
#22289=CARTESIAN_POINT('Ctrl Pts',(0.617880100977389,-3.88416183761904,
55.5150896969855));
#22290=CARTESIAN_POINT('Ctrl Pts',(0.503209139976766,-3.90240332907185,
55.5092238504353));
#22291=CARTESIAN_POINT('Ctrl Pts',(0.387811723368453,-3.91554940901367,
55.5033580038851));
#22292=CARTESIAN_POINT('Ctrl Pts',(0.272175392775181,-3.92357102083901,
55.4974921573349));
#22293=CARTESIAN_POINT('Ctrl Pts',(0.156459553650134,-3.93159814811589,
55.4916222775812));
#22294=CARTESIAN_POINT('Ctrl Pts',(0.0405048846693676,-3.93449378099791,
55.4857523978276));
#22295=CARTESIAN_POINT('Ctrl Pts',(-0.0752019080726868,-3.93228097584878,
55.4798825180739));
#22296=CARTESIAN_POINT('Ctrl Pts',(-0.191072773621905,-3.93006503293095,
55.4740043148016));
#22297=CARTESIAN_POINT('Ctrl Pts',(-0.306694651742633,-3.92272622381837,
55.4681261115293));
#22298=CARTESIAN_POINT('Ctrl Pts',(-0.421586779503249,-3.91033931869705,
55.4622479082569));
#22299=CARTESIAN_POINT('Ctrl Pts',(-0.438312444028915,-3.90853606878246,
55.4613921763816));
#22300=CARTESIAN_POINT('Ctrl Pts',(-0.455022663217249,-3.90662592396641,
55.4605364445063));
#22301=CARTESIAN_POINT('Ctrl Pts',(-0.471715975930993,-3.90460920426763,
55.459680712631));
#22302=CARTESIAN_POINT('Ctrl Pts',(-0.586371250022407,-3.89075769655348,
55.4538032589228));
#22303=CARTESIAN_POINT('Ctrl Pts',(-0.700603844411803,-3.87182908837603,
55.4479258052146));
#22304=CARTESIAN_POINT('Ctrl Pts',(-0.81392906842518,-3.8478576469995,55.4420483515063));
#22305=CARTESIAN_POINT('Ctrl Pts',(-0.927109461036369,-3.82391684149859,
55.4361784092755));
#22306=CARTESIAN_POINT('Ctrl Pts',(-1.03938438951155,-3.79494610458086,
55.4303084670447));
#22307=CARTESIAN_POINT('Ctrl Pts',(-1.15027460512398,-3.76103141874764,
55.4244385248139));
#22308=CARTESIAN_POINT('Ctrl Pts',(-1.26105260670441,-3.72715105247652,
55.4185745226012));
#22309=CARTESIAN_POINT('Ctrl Pts',(-1.37044829054053,-3.68833680898498,
55.4127105203885));
#22310=CARTESIAN_POINT('Ctrl Pts',(-1.47799357236597,-3.64472550407365,
55.4068465181757));
#22311=CARTESIAN_POINT('Ctrl Pts',(-1.58854994337173,-3.59989315509483,
55.4008183336454));
#22312=CARTESIAN_POINT('Ctrl Pts',(-1.69715032901682,-3.54999124256197,
55.3947901491151));
#22313=CARTESIAN_POINT('Ctrl Pts',(-1.80330361743498,-3.49522317790237,
55.3887619645848));
#22314=CARTESIAN_POINT('Ctrl Pts',(-1.90644949749864,-3.44200673672681,
55.3829045633885));
#22315=CARTESIAN_POINT('Ctrl Pts',(-2.0072846847053,-3.38419636745221,55.3770471621923));
#22316=CARTESIAN_POINT('Ctrl Pts',(-2.1053805464764,-3.32202675403417,55.371189760996));
#22317=CARTESIAN_POINT('Ctrl Pts',(-2.20346223840749,-3.25986612094882,
55.365333205895));
#22318=CARTESIAN_POINT('Ctrl Pts',(-2.29880504341771,-3.19334771663263,
55.3594766507939));
#22319=CARTESIAN_POINT('Ctrl Pts',(-2.39100763586765,-3.12275062808778,
55.3536200956929));
#22320=CARTESIAN_POINT('Ctrl Pts',(-2.48321912274417,-3.05214672931554,
55.3477629756327));
#22321=CARTESIAN_POINT('Ctrl Pts',(-2.57228946734184,-2.97746361494556,
55.3419058555725));
#22322=CARTESIAN_POINT('Ctrl Pts',(-2.65784943873237,-2.89902144887375,
55.3360487355123));
#22323=CARTESIAN_POINT('Ctrl Pts',(-2.74778349589481,-2.81656908087041,
55.3298921816736));
#22324=CARTESIAN_POINT('Ctrl Pts',(-2.83383838568118,-2.72996348587167,
55.3237356278349));
#22325=CARTESIAN_POINT('Ctrl Pts',(-2.91562920875397,-2.63962029789528,
55.3175790739962));
#22326=CARTESIAN_POINT('Ctrl Pts',(-2.99355793782203,-2.55354303941493,
55.3117132274616));
#22327=CARTESIAN_POINT('Ctrl Pts',(-3.06761586698334,-2.46407345665159,
55.3058473809269));
#22328=CARTESIAN_POINT('Ctrl Pts',(-3.13751229148755,-2.37160401854201,
55.2999815343923));
#22329=CARTESIAN_POINT('Ctrl Pts',(-3.20745677495527,-2.27907100085189,
55.2941116546541));
#22330=CARTESIAN_POINT('Ctrl Pts',(-3.27323382289168,-2.18353435947397,
55.2882417749159));
#22331=CARTESIAN_POINT('Ctrl Pts',(-3.33459683463049,-2.0854143354433,55.2823718951778));
#22332=CARTESIAN_POINT('Ctrl Pts',(-3.39604685942572,-1.9871551767296,55.2764936919209));
#22333=CARTESIAN_POINT('Ctrl Pts',(-3.45307015651262,-1.88630568322637,
55.270615488664));
#22334=CARTESIAN_POINT('Ctrl Pts',(-3.50546668555464,-1.78330937205708,
55.2647372854072));
#22335=CARTESIAN_POINT('Ctrl Pts',(-3.51309442211228,-1.76831546420914,
55.2638815534208));
#22336=CARTESIAN_POINT('Ctrl Pts',(-3.52062418949426,-1.75327609071389,
55.2630258214344));
#22337=CARTESIAN_POINT('Ctrl Pts',(-3.52805545744261,-1.73819265020005,
55.2621700894481));
#22338=CARTESIAN_POINT('Ctrl Pts',(-3.58270597932811,-1.62726704482021,
55.2558769238707));
#22339=CARTESIAN_POINT('Ctrl Pts',(-3.63218448513408,-1.51363371506473,
55.2495837582933));
#22340=CARTESIAN_POINT('Ctrl Pts',(-3.67623402409242,-1.39778124186345,
55.2432905927159));
#22341=CARTESIAN_POINT('Ctrl Pts',(-3.72014805511793,-1.28228516124943,
55.2370167865661));
#22342=CARTESIAN_POINT('Ctrl Pts',(-3.75866630602752,-1.16458384905882,
55.2307429804162));
#22343=CARTESIAN_POINT('Ctrl Pts',(-3.79157931829358,-1.0451867168542,55.2244691742664));
#22344=CARTESIAN_POINT('Ctrl Pts',(-3.82443080129216,-0.926012791751532,
55.2182070966905));
#22345=CARTESIAN_POINT('Ctrl Pts',(-3.85169783684823,-0.805149670778713,
55.2119450191145));
#22346=CARTESIAN_POINT('Ctrl Pts',(-3.87321950393292,-0.683124933195756,
55.2056829415386));
#22347=CARTESIAN_POINT('Ctrl Pts',(-3.89468073070556,-0.561442883434727,
55.1994384500503));
#22348=CARTESIAN_POINT('Ctrl Pts',(-3.9104287024252,-0.438606036713807,
55.193193958562));
#22349=CARTESIAN_POINT('Ctrl Pts',(-3.9203529112033,-0.315154012539693,
55.1869494670736));
#22350=CARTESIAN_POINT('Ctrl Pts',(-3.92874972239361,-0.21070202435307,
55.1816660417468));
#22351=CARTESIAN_POINT('Ctrl Pts',(-3.93297824814287,-0.105810025913677,
55.17638261642));
#22352=CARTESIAN_POINT('Ctrl Pts',(-3.93299991625273,-0.000811637929901232,
55.1710991910931));
#22353=CARTESIAN_POINT('',(-3.93299849539527,0.00344023525537216,53.9210991911024));
#22354=CARTESIAN_POINT('Ctrl Pts',(-3.93299991625288,-0.000811637171698235,
55.171099191055));
#22355=CARTESIAN_POINT('Ctrl Pts',(-3.93302469910098,0.119280126577695,
55.1650562805083));
#22356=CARTESIAN_POINT('Ctrl Pts',(-3.92754474829664,0.239305970276732,
55.1590133699616));
#22357=CARTESIAN_POINT('Ctrl Pts',(-3.91660425106563,0.358748018161383,
55.1529704594149));
#22358=CARTESIAN_POINT('Ctrl Pts',(-3.90565438845343,0.478292311884077,
55.1469223759625));
#22359=CARTESIAN_POINT('Ctrl Pts',(-3.88923469700456,0.597251441927818,
55.1408742925101));
#22360=CARTESIAN_POINT('Ctrl Pts',(-3.86744093349248,0.715115113773244,
55.1348262090577));
#22361=CARTESIAN_POINT('Ctrl Pts',(-3.84560602894256,0.833201282012232,
55.1287667083743));
#22362=CARTESIAN_POINT('Ctrl Pts',(-3.81837684731064,0.950187491230551,
55.122707207691));
#22363=CARTESIAN_POINT('Ctrl Pts',(-3.78590002041667,1.06557497878337,55.1166477070077));
#22364=CARTESIAN_POINT('Ctrl Pts',(-3.75339153151481,1.18107495883897,55.110582298852));
#22365=CARTESIAN_POINT('Ctrl Pts',(-3.71562531250432,1.29497275462065,55.1045168906962));
#22366=CARTESIAN_POINT('Ctrl Pts',(-3.67279687090257,1.40678788205201,55.0984514825405));
#22367=CARTESIAN_POINT('Ctrl Pts',(-3.62987684703792,1.5188421095303,55.0923731044101));
#22368=CARTESIAN_POINT('Ctrl Pts',(-3.58187311003354,1.62880442247361,55.0862947262797));
#22369=CARTESIAN_POINT('Ctrl Pts',(-3.52902855380103,1.73621613471858,55.0802163481492));
#22370=CARTESIAN_POINT('Ctrl Pts',(-3.48394544654873,1.82785194526426,55.0750307208546));
#22371=CARTESIAN_POINT('Ctrl Pts',(-3.43533991392117,1.91763167699019,55.0698450935599));
#22372=CARTESIAN_POINT('Ctrl Pts',(-3.38338756700251,2.00528740370375,55.0646594662652));
#22373=CARTESIAN_POINT('Ctrl Pts',(-3.32450413844372,2.10463748176254,55.0587820125514));
#22374=CARTESIAN_POINT('Ctrl Pts',(-3.26114449866947,2.20155463144174,55.0529045588376));
#22375=CARTESIAN_POINT('Ctrl Pts',(-3.19353534138345,2.29560907458891,55.0470271051238));
#22376=CARTESIAN_POINT('Ctrl Pts',(-3.12601258965375,2.38954331469244,55.0411571628874));
#22377=CARTESIAN_POINT('Ctrl Pts',(-3.0542513598767,2.48062179232339,55.035287220651));
#22378=CARTESIAN_POINT('Ctrl Pts',(-2.97852348231728,2.56844055124595,55.0294172784146));
#22379=CARTESIAN_POINT('Ctrl Pts',(-2.90287223668011,2.6561704430231,55.0235532761962));
#22380=CARTESIAN_POINT('Ctrl Pts',(-2.82326259561433,2.74064686703493,55.0176892739778));
#22381=CARTESIAN_POINT('Ctrl Pts',(-2.74000841260159,2.82149657077101,55.0118252717594));
#22382=CARTESIAN_POINT('Ctrl Pts',(-2.65442325092256,2.90460993175246,55.0057970872312));
#22383=CARTESIAN_POINT('Ctrl Pts',(-2.56498670439147,2.98389012328394,54.999768902703));
#22384=CARTESIAN_POINT('Ctrl Pts',(-2.47208285490105,3.0589696563556,54.9937407181748));
#22385=CARTESIAN_POINT('Ctrl Pts',(-2.38181104634603,3.13192212574219,54.9878833169729));
#22386=CARTESIAN_POINT('Ctrl Pts',(-2.28826610221537,3.20090848110424,54.982025915771));
#22387=CARTESIAN_POINT('Ctrl Pts',(-2.19183554554886,3.26563101731788,54.9761685145691));
#22388=CARTESIAN_POINT('Ctrl Pts',(-2.09541891817104,3.33034420443178,54.9703119594624));
#22389=CARTESIAN_POINT('Ctrl Pts',(-1.996117849541,3.39079456731503,54.9644554043558));
#22390=CARTESIAN_POINT('Ctrl Pts',(-1.8943494954736,3.44672728671692,54.9585988492491));
#22391=CARTESIAN_POINT('Ctrl Pts',(-1.79257132420814,3.50266540173112,54.9527417291833));
#22392=CARTESIAN_POINT('Ctrl Pts',(-1.68832575587778,3.55408480824334,54.9468846091175));
#22393=CARTESIAN_POINT('Ctrl Pts',(-1.58205460549139,3.60077661418249,54.9410274890516));
#22394=CARTESIAN_POINT('Ctrl Pts',(-1.47035055116756,3.64985544703733,54.9348709352209));
#22395=CARTESIAN_POINT('Ctrl Pts',(-1.35640879189321,3.6937103053147,54.9287143813901));
#22396=CARTESIAN_POINT('Ctrl Pts',(-1.24076483118586,3.73215643210361,54.9225578275593));
#22397=CARTESIAN_POINT('Ctrl Pts',(-1.13058148097809,3.7687871651415,54.9166919810191));
#22398=CARTESIAN_POINT('Ctrl Pts',(-1.01885343043069,3.80050822844357,54.9108261344789));
#22399=CARTESIAN_POINT('Ctrl Pts',(-0.906057021613535,3.82721173618404,
54.9049602879387));
#22400=CARTESIAN_POINT('Ctrl Pts',(-0.793183056920543,3.85393360456162,
54.8990904081951));
#22401=CARTESIAN_POINT('Ctrl Pts',(-0.679239675345709,3.87563097079524,
54.8932205284514));
#22402=CARTESIAN_POINT('Ctrl Pts',(-0.564710861801534,3.89224750530633,
54.8873506487078));
#22403=CARTESIAN_POINT('Ctrl Pts',(-0.450019645830238,3.90888760214599,
54.8814724454454));
#22404=CARTESIAN_POINT('Ctrl Pts',(-0.334741750038798,3.92043245027605,
54.8755942421831));
#22405=CARTESIAN_POINT('Ctrl Pts',(-0.21936369756515,3.92687771240595,54.8697160389208));
#22406=CARTESIAN_POINT('Ctrl Pts',(-0.202567292102037,3.92781599515322,
54.8688603069746));
#22407=CARTESIAN_POINT('Ctrl Pts',(-0.185768758550378,3.92864629385762,
54.8680045750285));
#22408=CARTESIAN_POINT('Ctrl Pts',(-0.168969590628545,3.92936868688124,
54.8671488430823));
#22409=CARTESIAN_POINT('Ctrl Pts',(-0.0535872770041763,3.93433032419565,
54.8612713893744));
#22410=CARTESIAN_POINT('Ctrl Pts',(0.0622028962169044,3.93421364901562,
54.8553939356666));
#22411=CARTESIAN_POINT('Ctrl Pts',(0.177917111223361,3.92897372115594,54.8495164819587));
#22412=CARTESIAN_POINT('Ctrl Pts',(0.293483441659719,3.92374049000572,54.8436465397283));
#22413=CARTESIAN_POINT('Ctrl Pts',(0.40897359852132,3.91339704624324,54.8377765974978));
#22414=CARTESIAN_POINT('Ctrl Pts',(0.523900730986083,3.89795036193026,54.8319066552674));
#22415=CARTESIAN_POINT('Ctrl Pts',(0.638711564309674,3.88251930870526,54.826042653055));
#22416=CARTESIAN_POINT('Ctrl Pts',(0.752960100088524,3.86199534194862,54.8201786508426));
#22417=CARTESIAN_POINT('Ctrl Pts',(0.866162244258594,3.83643740553927,54.8143146486302));
#22418=CARTESIAN_POINT('Ctrl Pts',(0.982533860363644,3.81016388937868,54.8082864640998));
#22419=CARTESIAN_POINT('Ctrl Pts',(1.09779918040499,3.77857036735483,54.8022582795693));
#22420=CARTESIAN_POINT('Ctrl Pts',(1.21144056831204,3.74177775254594,54.7962300950389));
#22421=CARTESIAN_POINT('Ctrl Pts',(1.32186240395243,3.70602750221875,54.7903726938429));
#22422=CARTESIAN_POINT('Ctrl Pts',(1.4307506685698,3.66536892867762,54.784515292647));
#22423=CARTESIAN_POINT('Ctrl Pts',(1.53764429402338,3.61996395355773,54.7786578914511));
#22424=CARTESIAN_POINT('Ctrl Pts',(1.64452247880962,3.57456553713686,54.7728013363504));
#22425=CARTESIAN_POINT('Ctrl Pts',(1.74940621780225,3.52442224372723,54.7669447812497));
#22426=CARTESIAN_POINT('Ctrl Pts',(1.85185417237748,3.46974424478924,54.761088226149));
#22427=CARTESIAN_POINT('Ctrl Pts',(1.95431200970947,3.4150609712768,54.7552311060892));
#22428=CARTESIAN_POINT('Ctrl Pts',(2.05433323159601,3.35584231686793,54.7493739860293));
#22429=CARTESIAN_POINT('Ctrl Pts',(2.15150149351262,3.29234419880621,54.7435168659694));
#22430=CARTESIAN_POINT('Ctrl Pts',(2.25363729230696,3.22559986395605,54.7373603121303));
#22431=CARTESIAN_POINT('Ctrl Pts',(2.3526202827518,3.15412720661996,54.7312037582911));
#22432=CARTESIAN_POINT('Ctrl Pts',(2.44800314821565,3.07827379976606,54.7250472044519));
#22433=CARTESIAN_POINT('Ctrl Pts',(2.53888211483149,3.00600212711658,54.7191813579176));
#22434=CARTESIAN_POINT('Ctrl Pts',(2.62649289859137,2.92975428334712,54.7133155113832));
#22435=CARTESIAN_POINT('Ctrl Pts',(2.71048488963366,2.84987028881449,54.7074496648488));
#22436=CARTESIAN_POINT('Ctrl Pts',(2.79453463138393,2.7699313681254,54.701579785111));
#22437=CARTESIAN_POINT('Ctrl Pts',(2.87496034062874,2.68635161476229,54.6957099053732));
#22438=CARTESIAN_POINT('Ctrl Pts',(2.95145041314914,2.59950561813621,54.6898400256353));
#22439=CARTESIAN_POINT('Ctrl Pts',(3.02804894897422,2.51253647345337,54.6839618223787));
#22440=CARTESIAN_POINT('Ctrl Pts',(3.10070045478603,2.42229216364554,54.6780836191221));
#22441=CARTESIAN_POINT('Ctrl Pts',(3.1691354861231,2.32917780999976,54.6722054158655));
#22442=CARTESIAN_POINT('Ctrl Pts',(3.17909806191479,2.31562248917406,54.6713496838768));
#22443=CARTESIAN_POINT('Ctrl Pts',(3.18897135756376,2.30200638890523,54.6704939518881));
#22444=CARTESIAN_POINT('Ctrl Pts',(3.19875462261016,2.28833080308116,54.6696382198994));
#22445=CARTESIAN_POINT('Ctrl Pts',(3.26594936136754,2.19440230247896,54.663760766191));
#22446=CARTESIAN_POINT('Ctrl Pts',(3.32911355679179,2.09735766200803,54.6578833124826));
#22447=CARTESIAN_POINT('Ctrl Pts',(3.38794523522725,1.99757755371372,54.6520058587742));
#22448=CARTESIAN_POINT('Ctrl Pts',(3.4467017258606,1.89792496595318,54.6461359165433));
#22449=CARTESIAN_POINT('Ctrl Pts',(3.50113650364579,1.79554421518162,54.6402659743123));
#22450=CARTESIAN_POINT('Ctrl Pts',(3.55098941731985,1.69084687600101,54.6343960320814));
#22451=CARTESIAN_POINT('Ctrl Pts',(3.60079188293217,1.58625548404477,54.6285320298685));
#22452=CARTESIAN_POINT('Ctrl Pts',(3.64602153101796,1.47935253706216,54.6226680276557));
#22453=CARTESIAN_POINT('Ctrl Pts',(3.68646324583839,1.37057569549537,54.6168040254428));
#22454=CARTESIAN_POINT('Ctrl Pts',(3.72803726146939,1.25875328312565,54.6107758409126));
#22455=CARTESIAN_POINT('Ctrl Pts',(3.76455104336783,1.1449508738046,54.6047476563823));
#22456=CARTESIAN_POINT('Ctrl Pts',(3.79582305288225,1.02966807817257,54.598719471852));
#22457=CARTESIAN_POINT('Ctrl Pts',(3.82620910112278,0.917651337202903,54.5928620706558));
#22458=CARTESIAN_POINT('Ctrl Pts',(3.8516462818897,0.804237389167053,54.5870046694595));
#22459=CARTESIAN_POINT('Ctrl Pts',(3.87201830941147,0.689900870837413,54.5811472682632));
#22460=CARTESIAN_POINT('Ctrl Pts',(3.892387394216,0.575580868293638,54.5752907131622));
#22461=CARTESIAN_POINT('Ctrl Pts',(3.90769270835451,0.460338966456682,54.5694341580612));
#22462=CARTESIAN_POINT('Ctrl Pts',(3.91786915725888,0.344659638773526,54.5635776029602));
#22463=CARTESIAN_POINT('Ctrl Pts',(3.92804658784575,0.22896915195495,54.5577204829));
#22464=CARTESIAN_POINT('Ctrl Pts',(3.93309413350725,0.112841566336625,54.5518633628399));
#22465=CARTESIAN_POINT('Ctrl Pts',(3.93299866990278,-0.00323458543118984,
54.5460062427797));
#22466=CARTESIAN_POINT('Ctrl Pts',(3.93289832590871,-0.125244902856397,
54.5398496889411));
#22467=CARTESIAN_POINT('Ctrl Pts',(3.92711520564665,-0.247197880111946,
54.5336931351025));
#22468=CARTESIAN_POINT('Ctrl Pts',(3.91569603009031,-0.368528967565535,
54.5275365812639));
#22469=CARTESIAN_POINT('Ctrl Pts',(3.90481605841775,-0.48413090292266,54.5216707347294));
#22470=CARTESIAN_POINT('Ctrl Pts',(3.88882024546085,-0.599167927744024,
54.5158048881948));
#22471=CARTESIAN_POINT('Ctrl Pts',(3.86780182215661,-0.713160616216218,
54.5099390416603));
#22472=CARTESIAN_POINT('Ctrl Pts',(3.84676894713138,-0.827231683095119,
54.5040691619223));
#22473=CARTESIAN_POINT('Ctrl Pts',(3.82070667763449,-0.940256582962956,
54.4981992821843));
#22474=CARTESIAN_POINT('Ctrl Pts',(3.78975850888195,-1.051769672674,54.4923294024463));
#22475=CARTESIAN_POINT('Ctrl Pts',(3.75876645547193,-1.16344088850185,54.4864511991895));
#22476=CARTESIAN_POINT('Ctrl Pts',(3.72287480551736,-1.27359562609761,54.4805729959328));
#22477=CARTESIAN_POINT('Ctrl Pts',(3.68227566039492,-1.38178687244562,54.4746947926761));
#22478=CARTESIAN_POINT('Ctrl Pts',(3.67636535318206,-1.39753704407438,54.4738390606896));
#22479=CARTESIAN_POINT('Ctrl Pts',(3.67035536153618,-1.41324564530154,54.4729833287031));
#22480=CARTESIAN_POINT('Ctrl Pts',(3.66424635914895,-1.42891134065888,54.4721275967165));
#22481=CARTESIAN_POINT('Ctrl Pts',(3.62228768587896,-1.53650858017229,54.4662501429928));
#22482=CARTESIAN_POINT('Ctrl Pts',(3.57551698132201,-1.6424325108648,54.460372689269));
#22483=CARTESIAN_POINT('Ctrl Pts',(3.52408809690542,-1.74622223249203,54.4544952355452));
#22484=CARTESIAN_POINT('Ctrl Pts',(3.47272493940417,-1.84987930923839,54.4486252932988));
#22485=CARTESIAN_POINT('Ctrl Pts',(3.41671562307969,-1.95140723502391,54.4427553510525));
#22486=CARTESIAN_POINT('Ctrl Pts',(3.35626273166703,-2.05036325465096,54.4368854088061));
#22487=CARTESIAN_POINT('Ctrl Pts',(3.29587101483622,-2.14921913691517,54.4310214065777));
#22488=CARTESIAN_POINT('Ctrl Pts',(3.23104488126119,-2.24550794006632,54.4251574043494));
#22489=CARTESIAN_POINT('Ctrl Pts',(3.16203336820224,-2.33881037674616,54.419293402121));
#22490=CARTESIAN_POINT('Ctrl Pts',(3.09108964771404,-2.43472512626092,54.4132652175965));
#22491=CARTESIAN_POINT('Ctrl Pts',(3.01572290971197,-2.52748341109336,54.407237033072));
#22492=CARTESIAN_POINT('Ctrl Pts',(2.93625242311743,-2.61666022015411,54.4012088485476));
#22493=CARTESIAN_POINT('Ctrl Pts',(2.859033399282,-2.70331057853889,54.3953514473358));
#22494=CARTESIAN_POINT('Ctrl Pts',(2.77794032268958,-2.78657934079926,54.389494046124));
#22495=CARTESIAN_POINT('Ctrl Pts',(2.69330719610779,-2.86610979332508,54.3836366449123));
#22496=CARTESIAN_POINT('Ctrl Pts',(2.60868629468924,-2.94562875776339,54.3777800897957));
#22497=CARTESIAN_POINT('Ctrl Pts',(2.52052666065431,-3.02141020385537,54.3719235346792));
#22498=CARTESIAN_POINT('Ctrl Pts',(2.4291985038431,-3.09313491928923,54.3660669795627));
#22499=CARTESIAN_POINT('Ctrl Pts',(2.33786153695993,-3.16486655372732,54.360209859487));
#22500=CARTESIAN_POINT('Ctrl Pts',(2.24335576411272,-3.2325404247759,54.3543527394114));
#22501=CARTESIAN_POINT('Ctrl Pts',(2.14608318887078,-3.29587863041802,54.3484956193358));
#22502=CARTESIAN_POINT('Ctrl Pts',(2.0438377445828,-3.36245487721909,54.342339065519));
#22503=CARTESIAN_POINT('Ctrl Pts',(1.93853554331856,-3.42424014600822,54.3361825117021));
#22504=CARTESIAN_POINT('Ctrl Pts',(1.83067495367516,-3.48096512679837,54.3300259578853));
#22505=CARTESIAN_POINT('Ctrl Pts',(1.72790744989947,-3.5350116019456,54.3241601113355));
#22506=CARTESIAN_POINT('Ctrl Pts',(1.62281805304736,-3.58446462863214,54.3182942647857));
#22507=CARTESIAN_POINT('Ctrl Pts',(1.51585924635706,-3.62914035898775,54.3124284182359));
#22508=CARTESIAN_POINT('Ctrl Pts',(1.40882689757588,-3.67384680721246,54.3065585384828));
#22509=CARTESIAN_POINT('Ctrl Pts',(1.29992296573686,-3.71376927683264,54.3006886587296));
#22510=CARTESIAN_POINT('Ctrl Pts',(1.18961585217552,-3.74877354934286,54.2948187789765));
#22511=CARTESIAN_POINT('Ctrl Pts',(1.07915232258203,-3.78382745808449,54.2889405757048));
#22512=CARTESIAN_POINT('Ctrl Pts',(0.967282037537844,-3.81394914705215,
54.2830623724331));
#22513=CARTESIAN_POINT('Ctrl Pts',(0.854484350536292,-3.8390552867455,54.2771841691615));
#22514=CARTESIAN_POINT('Ctrl Pts',(0.838063588640734,-3.84271016614046,
54.2763284372856));
#22515=CARTESIAN_POINT('Ctrl Pts',(0.82162318178757,-3.84625884217346,54.2754727054096));
#22516=CARTESIAN_POINT('Ctrl Pts',(0.805164616578459,-3.84970114946733,
54.2746169735337));
#22517=CARTESIAN_POINT('Ctrl Pts',(0.692121667573628,-3.87334407112761,
54.2687395198443));
#22518=CARTESIAN_POINT('Ctrl Pts',(0.577851158963191,-3.89204242967716,
54.2628620661548));
#22519=CARTESIAN_POINT('Ctrl Pts',(0.462823177736543,-3.90567327181241,
54.2569846124653));
#22520=CARTESIAN_POINT('Ctrl Pts',(0.347942204061899,-3.91928669351906,
54.2511146702532));
#22521=CARTESIAN_POINT('Ctrl Pts',(0.232306089007898,-3.92784543061053,
54.2452447280411));
#22522=CARTESIAN_POINT('Ctrl Pts',(0.116396346927415,-3.93127725941862,
54.239374785829));
#22523=CARTESIAN_POINT('Ctrl Pts',(0.000603898327194333,-3.9347056154285,
54.2335107836349));
#22524=CARTESIAN_POINT('Ctrl Pts',(-0.115461216568417,-3.93301737104643,
54.2276467814408));
#22525=CARTESIAN_POINT('Ctrl Pts',(-0.231311759198476,-3.92619203173463,
54.2217827792466));
#22526=CARTESIAN_POINT('Ctrl Pts',(-0.350405925026531,-3.91917559423354,
54.2157545947093));
#22527=CARTESIAN_POINT('Ctrl Pts',(-0.469272885050501,-3.90673009317892,
54.209726410172));
#22528=CARTESIAN_POINT('Ctrl Pts',(-0.587382235703046,-3.88889072991007,
54.2036982256347));
#22529=CARTESIAN_POINT('Ctrl Pts',(-0.702145452613,-3.8715567702782,54.1978408244568));
#22530=CARTESIAN_POINT('Ctrl Pts',(-0.816192976570165,-3.84913053608896,
54.1919834232789));
#22531=CARTESIAN_POINT('Ctrl Pts',(-0.929043557234587,-3.82169688342246,
54.186126022101));
#22532=CARTESIAN_POINT('Ctrl Pts',(-1.04187783675824,-3.79426719351655,
54.1802694670182));
#22533=CARTESIAN_POINT('Ctrl Pts',(-1.15351511607574,-3.761831620883,54.1744129119354));
#22534=CARTESIAN_POINT('Ctrl Pts',(-1.26348577260973,-3.72452583591694,
54.1685563568526));
#22535=CARTESIAN_POINT('Ctrl Pts',(-1.37346703758901,-3.68721645220563,
54.1626992368106));
#22536=CARTESIAN_POINT('Ctrl Pts',(-1.48178096953255,-3.64503605474311,
54.1568421167685));
#22537=CARTESIAN_POINT('Ctrl Pts',(-1.58797517510659,-3.59816951285584,
54.1509849967264));
#22538=CARTESIAN_POINT('Ctrl Pts',(-1.69959835203152,-3.54890701055015,
54.1448284428617));
#22539=CARTESIAN_POINT('Ctrl Pts',(-1.80887886874512,-3.4944667502624,54.1386718889971));
#22540=CARTESIAN_POINT('Ctrl Pts',(-1.91531887921463,-3.43511900680662,
54.1325153351325));
#22541=CARTESIAN_POINT('Ctrl Pts',(-2.01673288101222,-3.3785736143836,54.1266494886154));
#22542=CARTESIAN_POINT('Ctrl Pts',(-2.1155681723429,-3.31757387487189,54.1207836420982));
#22543=CARTESIAN_POINT('Ctrl Pts',(-2.21142355605467,-3.25239832365695,
54.1149177955811));
#22544=CARTESIAN_POINT('Ctrl Pts',(-2.30734484743756,-3.18717795942653,
54.1090479158604));
#22545=CARTESIAN_POINT('Ctrl Pts',(-2.40028182175256,-3.11777631243909,
54.1031780361396));
#22546=CARTESIAN_POINT('Ctrl Pts',(-2.48986615243409,-3.04451236538187,
54.0973081564188));
#22547=CARTESIAN_POINT('Ctrl Pts',(-2.57957751414965,-2.97114452967715,
54.0914299531789));
#22548=CARTESIAN_POINT('Ctrl Pts',(-2.66592643995281,-2.89390373942269,
54.085551749939));
#22549=CARTESIAN_POINT('Ctrl Pts',(-2.74858124202434,-2.81314595355307,
54.0796735466991));
#22550=CARTESIAN_POINT('Ctrl Pts',(-2.7606138931248,-2.80138946467812,54.078817814583));
#22551=CARTESIAN_POINT('Ctrl Pts',(-2.77256832580449,-2.78955849781866,
54.0779620824669));
#22552=CARTESIAN_POINT('Ctrl Pts',(-2.7844435893455,-2.77765420773588,54.0771063503508));
#22553=CARTESIAN_POINT('Ctrl Pts',(-2.86487758717835,-2.69702360619902,
54.0713102722314));
#22554=CARTESIAN_POINT('Ctrl Pts',(-2.94195621667249,-2.61274587632333,
54.0655141941119));
#22555=CARTESIAN_POINT('Ctrl Pts',(-3.01532404489709,-2.52513562096484,
54.0597181159925));
#22556=CARTESIAN_POINT('Ctrl Pts',(-3.08857726562201,-2.43766222112678,
54.0539310918962));
#22557=CARTESIAN_POINT('Ctrl Pts',(-3.1581309477068,-2.34686697586053,54.0481440678));
#22558=CARTESIAN_POINT('Ctrl Pts',(-3.2236657095407,-2.25310194912071,54.0423570437038));
#22559=CARTESIAN_POINT('Ctrl Pts',(-3.28914205744857,-2.15942049914507,
54.0365751778288));
#22560=CARTESIAN_POINT('Ctrl Pts',(-3.35060635987211,-2.06277487262656,
54.0307933119538));
#22561=CARTESIAN_POINT('Ctrl Pts',(-3.40777900761285,-1.96355067041145,
54.0250114460788));
#22562=CARTESIAN_POINT('Ctrl Pts',(-3.46491539869334,-1.86438939231005,
54.0192332468372));
#22563=CARTESIAN_POINT('Ctrl Pts',(-3.51776533204567,-1.76265315515072,
54.0134550475958));
#22564=CARTESIAN_POINT('Ctrl Pts',(-3.56609260362719,-1.65875632398357,
54.0076768483543));
#22565=CARTESIAN_POINT('Ctrl Pts',(-3.61440165302202,-1.55489866795281,
54.0019008278293));
#22566=CARTESIAN_POINT('Ctrl Pts',(-3.65819125215211,-1.44888242258307,
53.9961248073043));
#22567=CARTESIAN_POINT('Ctrl Pts',(-3.69727164606475,-1.34114554586955,
53.9903487867793));
#22568=CARTESIAN_POINT('Ctrl Pts',(-3.73636210810007,-1.23338091334337,
53.9845712782017));
#22569=CARTESIAN_POINT('Ctrl Pts',(-3.77074078579598,-1.1238951600797,53.9787937696241));
#22570=CARTESIAN_POINT('Ctrl Pts',(-3.80026663420399,-1.01314486079533,
53.9730162610465));
#22571=CARTESIAN_POINT('Ctrl Pts',(-3.82979492306188,-0.902385407479146,
53.9672382749307));
#22572=CARTESIAN_POINT('Ctrl Pts',(-3.85446948338104,-0.790361613535798,
53.9614602888149));
#22573=CARTESIAN_POINT('Ctrl Pts',(-3.87419996464605,-0.677542348445218,
53.9556823026991));
#22574=CARTESIAN_POINT('Ctrl Pts',(-3.89395032833318,-0.56460939528879,
53.949898494102));
#22575=CARTESIAN_POINT('Ctrl Pts',(-3.90874659429761,-0.450879790525878,
53.9441146855048));
#22576=CARTESIAN_POINT('Ctrl Pts',(-3.91855008018397,-0.336829733085216,
53.9383308769077));
#22577=CARTESIAN_POINT('Ctrl Pts',(-3.92828591345906,-0.223566720609123,
53.9325869816393));
#22578=CARTESIAN_POINT('Ctrl Pts',(-3.93309771233674,-0.109988077799192,
53.9268430863709));
#22579=CARTESIAN_POINT('Ctrl Pts',(-3.93299849539527,0.00344023525537207,
53.9210991911024));
#22580=CARTESIAN_POINT('',(-3.93299921172447,-0.00249009532928107,52.6710991910122));
#22581=CARTESIAN_POINT('Ctrl Pts',(-3.93299849539445,0.003440236192082,
53.921099191055));
#22582=CARTESIAN_POINT('Ctrl Pts',(-3.93285730429221,0.164854848927317,
53.9129253180124));
#22583=CARTESIAN_POINT('Ctrl Pts',(-3.92277566495795,0.325846686158594,
53.9047514449697));
#22584=CARTESIAN_POINT('Ctrl Pts',(-3.90292980314051,0.485415236429215,
53.8965775719271));
#22585=CARTESIAN_POINT('Ctrl Pts',(-3.88918603920976,0.5959205148528,53.8909169570073));
#22586=CARTESIAN_POINT('Ctrl Pts',(-3.87076040826518,0.705743982120764,
53.8852563420876));
#22587=CARTESIAN_POINT('Ctrl Pts',(-3.84772403021341,0.814560487206655,
53.8795957271679));
#22588=CARTESIAN_POINT('Ctrl Pts',(-3.8238052069376,0.927545382175443,53.8737182733602));
#22589=CARTESIAN_POINT('Ctrl Pts',(-3.79486641686709,1.03966105773686,53.8678408195524));
#22590=CARTESIAN_POINT('Ctrl Pts',(-3.76098458040149,1.15042774044366,53.8619633657447));
#22591=CARTESIAN_POINT('Ctrl Pts',(-3.72714604544839,1.26105286161199,53.856093423414));
#22592=CARTESIAN_POINT('Ctrl Pts',(-3.68837714723683,1.37033202765081,53.8502234810834));
#22593=CARTESIAN_POINT('Ctrl Pts',(-3.64480583910922,1.47779545106737,53.8443535387528));
#22594=CARTESIAN_POINT('Ctrl Pts',(-3.60127862244515,1.58515012815939,53.83848953644));
#22595=CARTESIAN_POINT('Ctrl Pts',(-3.55295881680666,1.69069233749325,53.8326255341273));
#22596=CARTESIAN_POINT('Ctrl Pts',(-3.50002402481952,1.79396789984834,53.8267615318145));
#22597=CARTESIAN_POINT('Ctrl Pts',(-3.445607147886,1.90013500386344,53.8207333473216));
#22598=CARTESIAN_POINT('Ctrl Pts',(-3.38631316709253,2.00390623425911,53.8147051628287));
#22599=CARTESIAN_POINT('Ctrl Pts',(-3.32238805348545,2.10481035299079,53.8086769783358));
#22600=CARTESIAN_POINT('Ctrl Pts',(-3.26027398850708,2.20285577886221,53.8028195770397));
#22601=CARTESIAN_POINT('Ctrl Pts',(-3.19378791043858,2.29819399583277,53.7969621757437));
#22602=CARTESIAN_POINT('Ctrl Pts',(-3.12320142531508,2.39041876183023,53.7911047744476));
#22603=CARTESIAN_POINT('Ctrl Pts',(-3.05262513633502,2.48263020605734,53.785248219247));
#22604=CARTESIAN_POINT('Ctrl Pts',(-2.97794986875202,2.57172876613824,53.7793916640464));
#22605=CARTESIAN_POINT('Ctrl Pts',(-2.89948904773072,2.65733932008874,53.7735351088458));
#22606=CARTESIAN_POINT('Ctrl Pts',(-2.82102065790323,2.74295813255197,53.7676779886864));
#22607=CARTESIAN_POINT('Ctrl Pts',(-2.73876626741577,2.82508796588879,53.7618208685269));
#22608=CARTESIAN_POINT('Ctrl Pts',(-2.65307738474624,2.90338929366148,53.7559637483675));
#22609=CARTESIAN_POINT('Ctrl Pts',(-2.56300782954424,2.98569362001629,53.749807194669));
#22610=CARTESIAN_POINT('Ctrl Pts',(-2.4691437019627,3.06376729023432,53.7436506409704));
#22611=CARTESIAN_POINT('Ctrl Pts',(-2.37193299098857,3.13726359846604,53.7374940872719));
#22612=CARTESIAN_POINT('Ctrl Pts',(-2.27931248453441,3.20728947547813,53.7316282406398));
#22613=CARTESIAN_POINT('Ctrl Pts',(-2.18365459889173,3.27316020083352,53.7257623940077));
#22614=CARTESIAN_POINT('Ctrl Pts',(-2.08537593326546,3.33462085055516,53.7198965473756));
#22615=CARTESIAN_POINT('Ctrl Pts',(-1.9870296937972,3.3961237590133,53.7140266675407));
#22616=CARTESIAN_POINT('Ctrl Pts',(-1.88605944427407,3.45321035146174,53.7081567877058));
#22617=CARTESIAN_POINT('Ctrl Pts',(-1.7829055542137,3.50567208745398,53.7022869078708));
#22618=CARTESIAN_POINT('Ctrl Pts',(-1.67960539145098,3.55820821443516,53.6964087045186));
#22619=CARTESIAN_POINT('Ctrl Pts',(-1.57411578352132,3.60610622928743,53.6905305011664));
#22620=CARTESIAN_POINT('Ctrl Pts',(-1.46689617496833,3.64920602485846,53.6846522978142));
#22621=CARTESIAN_POINT('Ctrl Pts',(-1.45128746479236,3.65548036428938,53.6837965665378));
#22622=CARTESIAN_POINT('Ctrl Pts',(-1.43564211492558,3.6616531036275,53.6829408352614));
#22623=CARTESIAN_POINT('Ctrl Pts',(-1.41996156534227,3.66772383815232,53.682085103985));
#22624=CARTESIAN_POINT('Ctrl Pts',(-1.3122622163181,3.70941970811829,53.6762076504611));
#22625=CARTESIAN_POINT('Ctrl Pts',(-1.20254823139564,3.74643617145609,53.6703301969372));
#22626=CARTESIAN_POINT('Ctrl Pts',(-1.09126347367353,3.77857552935309,53.6644527434132));
#22627=CARTESIAN_POINT('Ctrl Pts',(-0.980120939606572,3.8106738126497,53.6585828013665));
#22628=CARTESIAN_POINT('Ctrl Pts',(-0.867412017898489,3.8379072730176,53.6527128593198));
#22629=CARTESIAN_POINT('Ctrl Pts',(-0.75360008967137,3.86012641047509,53.646842917273));
#22630=CARTESIAN_POINT('Ctrl Pts',(-0.639903332063104,3.88232306354231,
53.6409789152439));
#22631=CARTESIAN_POINT('Ctrl Pts',(-0.525106190717566,3.89951540851951,
53.6351149132148));
#22632=CARTESIAN_POINT('Ctrl Pts',(-0.409686099805357,3.91160405711343,
53.6292509111857));
#22633=CARTESIAN_POINT('Ctrl Pts',(-0.291034433070842,3.92403116831133,
53.6232227265864));
#22634=CARTESIAN_POINT('Ctrl Pts',(-0.171724843581924,3.93106444109953,
53.6171945419871));
#22635=CARTESIAN_POINT('Ctrl Pts',(-0.0522864064142289,3.93265242955747,
53.6111663573878));
#22636=CARTESIAN_POINT('Ctrl Pts',(0.0637682384864407,3.93419542895501,
53.605308956373));
#22637=CARTESIAN_POINT('Ctrl Pts',(0.179944088795455,3.93059753512055,53.5994515553583));
#22638=CARTESIAN_POINT('Ctrl Pts',(0.295752501716406,3.92186428344078,53.5935941543435));
#22639=CARTESIAN_POINT('Ctrl Pts',(0.411544186260149,3.91313229326806,53.5877375994228));
#22640=CARTESIAN_POINT('Ctrl Pts',(0.526968127731309,3.89926645134358,53.5818810445021));
#22641=CARTESIAN_POINT('Ctrl Pts',(0.641538900322014,3.88032432141614,53.5760244895814));
#22642=CARTESIAN_POINT('Ctrl Pts',(0.756120725136563,3.86138036421062,53.5701673697003));
#22643=CARTESIAN_POINT('Ctrl Pts',(0.869848810469708,3.83735921282958,53.5643102498191));
#22644=CARTESIAN_POINT('Ctrl Pts',(0.982246737016988,3.80836977558895,53.558453129938));
#22645=CARTESIAN_POINT('Ctrl Pts',(1.10039079569383,3.77789830801322,53.5522965758434));
#22646=CARTESIAN_POINT('Ctrl Pts',(1.21706460083901,3.74193725081163,53.5461400217487));
#22647=CARTESIAN_POINT('Ctrl Pts',(1.33173300771971,3.70067239784202,53.5399834676541));
#22648=CARTESIAN_POINT('Ctrl Pts',(1.44098686090307,3.66135603939059,53.5341176212935));
#22649=CARTESIAN_POINT('Ctrl Pts',(1.5484200079586,3.61722553696908,53.5282517749329));
#22650=CARTESIAN_POINT('Ctrl Pts',(1.65359132669396,3.56849053862869,53.5223859285724));
#22651=CARTESIAN_POINT('Ctrl Pts',(1.7588349585249,3.51972203135606,53.5165160490066));
#22652=CARTESIAN_POINT('Ctrl Pts',(1.86181330011028,3.46634291336468,53.5106461694409));
#22653=CARTESIAN_POINT('Ctrl Pts',(1.96211109121973,3.40860808332558,53.5047762898751));
#22654=CARTESIAN_POINT('Ctrl Pts',(2.06255110516054,3.35079138497308,53.4988980867872));
#22655=CARTESIAN_POINT('Ctrl Pts',(2.16030263759414,3.28860687062497,53.4930198836992));
#22656=CARTESIAN_POINT('Ctrl Pts',(2.25498057231444,3.22235187688812,53.4871416806113));
#22657=CARTESIAN_POINT('Ctrl Pts',(2.26876353582098,3.21270665000924,53.4862859473416));
#22658=CARTESIAN_POINT('Ctrl Pts',(2.28248142121484,3.20297522571995,53.4854302140719));
#22659=CARTESIAN_POINT('Ctrl Pts',(2.29613310278219,3.1931585889692,53.4845744808022));
#22660=CARTESIAN_POINT('Ctrl Pts',(2.3898972809373,3.12573474285618,53.478697027072));
#22661=CARTESIAN_POINT('Ctrl Pts',(2.48084288367599,3.0540669316364,53.4728195733417));
#22662=CARTESIAN_POINT('Ctrl Pts',(2.56856182247688,2.97841890339727,53.4669421196115));
#22663=CARTESIAN_POINT('Ctrl Pts',(2.65616865508283,2.90286755453795,53.4610721773603));
#22664=CARTESIAN_POINT('Ctrl Pts',(2.74055671523021,2.82334637202897,53.4552022351091));
#22665=CARTESIAN_POINT('Ctrl Pts',(2.82134762001191,2.74016178483189,53.449332292858));
#22666=CARTESIAN_POINT('Ctrl Pts',(2.9020567693786,2.65706137530885,53.4434682906265));
#22667=CARTESIAN_POINT('Ctrl Pts',(2.97917571841164,2.57030522942354,53.437604288395));
#22668=CARTESIAN_POINT('Ctrl Pts',(3.05236037773252,2.48023892487166,53.4317402861635));
#22669=CARTESIAN_POINT('Ctrl Pts',(3.12759408556559,2.38765091387129,53.4257121016409));
#22670=CARTESIAN_POINT('Ctrl Pts',(3.19866960110609,2.29156493349301,53.4196839171182));
#22671=CARTESIAN_POINT('Ctrl Pts',(3.26525477551063,2.19239600688493,53.4136557325955));
#22672=CARTESIAN_POINT('Ctrl Pts',(3.32995353841542,2.09603661566131,53.4077983313847));
#22673=CARTESIAN_POINT('Ctrl Pts',(3.39041272939229,1.99676698273288,53.4019409301739));
#22674=CARTESIAN_POINT('Ctrl Pts',(3.44637001481703,1.89499939867272,53.3960835289631));
#22675=CARTESIAN_POINT('Ctrl Pts',(3.50231921725811,1.79324651485602,53.390226973849));
#22676=CARTESIAN_POINT('Ctrl Pts',(3.55376760858011,1.68899675879178,53.384370418735));
#22677=CARTESIAN_POINT('Ctrl Pts',(3.60049818948871,1.58268815231823,53.378513863621));
#22678=CARTESIAN_POINT('Ctrl Pts',(3.64723327830258,1.47636929069443,53.3726567435493));
#22679=CARTESIAN_POINT('Ctrl Pts',(3.68924948598868,1.3679915614872,53.3667996234777));
#22680=CARTESIAN_POINT('Ctrl Pts',(3.72637773796442,1.25801349515936,53.3609425034061));
#22681=CARTESIAN_POINT('Ctrl Pts',(3.76540409879904,1.14241301649401,53.3547859495905));
#22682=CARTESIAN_POINT('Ctrl Pts',(3.79902934229234,1.0250447242216,53.348629395775));
#22683=CARTESIAN_POINT('Ctrl Pts',(3.82711670531169,0.90645834097553,53.3424728419594));
#22684=CARTESIAN_POINT('Ctrl Pts',(3.85387780676215,0.793471506629281,53.3366069954173));
#22685=CARTESIAN_POINT('Ctrl Pts',(3.87561204479805,0.679379411978636,53.3307411488752));
#22686=CARTESIAN_POINT('Ctrl Pts',(3.89225400468771,0.564666063255461,53.3248753023331));
#22687=CARTESIAN_POINT('Ctrl Pts',(3.90890740715212,0.449873840644997,53.3190054225889));
#22688=CARTESIAN_POINT('Ctrl Pts',(3.920461518559,0.334459922704503,53.3131355428447));
#22689=CARTESIAN_POINT('Ctrl Pts',(3.92690295383275,0.218911377455589,53.3072656631005));
#22690=CARTESIAN_POINT('Ctrl Pts',(3.93335352309169,0.103198983832043,53.3013874598396));
#22691=CARTESIAN_POINT('Ctrl Pts',(3.93467694536156,-0.012648007394774,
53.2955092565786));
#22692=CARTESIAN_POINT('Ctrl Pts',(3.93091184894263,-0.128144589594604,
53.2896310533176));
#22693=CARTESIAN_POINT('Ctrl Pts',(3.93036373705076,-0.144958249360539,
53.2887753214182));
#22694=CARTESIAN_POINT('Ctrl Pts',(3.92970787483743,-0.161764496431242,
53.2879195895187));
#22695=CARTESIAN_POINT('Ctrl Pts',(3.92894447221929,-0.178561849837614,
53.2870638576193));
#22696=CARTESIAN_POINT('Ctrl Pts',(3.92370116635798,-0.293931720830033,
53.28118640321));
#22697=CARTESIAN_POINT('Ctrl Pts',(3.91336336805461,-0.409259562022228,
53.2753089488007));
#22698=CARTESIAN_POINT('Ctrl Pts',(3.89792902249375,-0.524059477159622,
53.2694314943914));
#22699=CARTESIAN_POINT('Ctrl Pts',(3.88251440225738,-0.638712676288338,
53.2635615514567));
#22700=CARTESIAN_POINT('Ctrl Pts',(3.86201624293027,-0.752838885977837,
53.2576916085221));
#22701=CARTESIAN_POINT('Ctrl Pts',(3.83648446702211,-0.865953771455513,
53.2518216655874));
#22702=CARTESIAN_POINT('Ctrl Pts',(3.81097852767865,-0.978954191724504,
53.2459576626689));
#22703=CARTESIAN_POINT('Ctrl Pts',(3.78044919428983,-1.09094492343176,53.2400936597504));
#22704=CARTESIAN_POINT('Ctrl Pts',(3.74499791492547,-1.20144896570924,53.2342296568319));
#22705=CARTESIAN_POINT('Ctrl Pts',(3.70855406463075,-1.3150469188982,53.2282014725654));
#22706=CARTESIAN_POINT('Ctrl Pts',(3.6669086386595,-1.4270732622134,53.2221732882989));
#22707=CARTESIAN_POINT('Ctrl Pts',(3.62022777324901,-1.5370230544128,53.2161451040324));
#22708=CARTESIAN_POINT('Ctrl Pts',(3.57486940698688,-1.64385789779391,53.2102877021302));
#22709=CARTESIAN_POINT('Ctrl Pts',(3.52475725730696,-1.74873186593735,53.2044303002279));
#22710=CARTESIAN_POINT('Ctrl Pts',(3.47009331534487,-1.85119998455024,53.1985728983256));
#22711=CARTESIAN_POINT('Ctrl Pts',(3.41543726953916,-1.95365330173717,53.1927163425197));
#22712=CARTESIAN_POINT('Ctrl Pts',(3.35623093302101,-2.05370109659577,53.1868597867138));
#22713=CARTESIAN_POINT('Ctrl Pts',(3.29272261672546,-2.15092230666395,53.1810032309079));
#22714=CARTESIAN_POINT('Ctrl Pts',(3.22920817405052,-2.24815289525218,53.1751461101448));
#22715=CARTESIAN_POINT('Ctrl Pts',(3.16139115222987,-2.34255601164886,53.1692889893816));
#22716=CARTESIAN_POINT('Ctrl Pts',(3.0895632229923,-2.43373952820209,53.1634318686185));
#22717=CARTESIAN_POINT('Ctrl Pts',(3.01406325291621,-2.52958459632918,53.15727531577));
#22718=CARTESIAN_POINT('Ctrl Pts',(2.9341317409814,-2.62187176497204,53.1511187629214));
#22719=CARTESIAN_POINT('Ctrl Pts',(2.85015439061182,-2.71018614668367,53.1449622100729));
#22720=CARTESIAN_POINT('Ctrl Pts',(2.77014235792697,-2.79433042088328,53.1390963628466));
#22721=CARTESIAN_POINT('Ctrl Pts',(2.6864581807883,-2.87486826708975,53.1332305156203));
#22722=CARTESIAN_POINT('Ctrl Pts',(2.59947150285008,-2.95148046001838,53.1273646683939));
#22723=CARTESIAN_POINT('Ctrl Pts',(2.51242501520104,-3.02814532943969,53.1214947879681));
#22724=CARTESIAN_POINT('Ctrl Pts',(2.42207182567495,-3.10087891295247,53.1156249075422));
#22725=CARTESIAN_POINT('Ctrl Pts',(2.32881256873694,-3.1694038902754,53.1097550271164));
#22726=CARTESIAN_POINT('Ctrl Pts',(2.23542106987779,-3.23802603623278,53.1038768231816));
#22727=CARTESIAN_POINT('Ctrl Pts',(2.13911562234646,-3.30242743961088,53.0979986192467));
#22728=CARTESIAN_POINT('Ctrl Pts',(2.04032355156761,-3.36237547054437,53.0921204153119));
#22729=CARTESIAN_POINT('Ctrl Pts',(2.02594177114823,-3.3711024808263,53.0912646883534));
#22730=CARTESIAN_POINT('Ctrl Pts',(2.01150733054545,-3.37973519521384,53.0904089613949));
#22731=CARTESIAN_POINT('Ctrl Pts',(1.99702158481975,-3.38827298040816,53.0895532344364));
#22732=CARTESIAN_POINT('Ctrl Pts',(1.8975280770807,-3.44691367543279,53.0836757823273));
#22733=CARTESIAN_POINT('Ctrl Pts',(1.79528639897419,-3.50126448233823,53.0777983302181));
#22734=CARTESIAN_POINT('Ctrl Pts',(1.69070239339066,-3.55105821086941,53.071920878109));
#22735=CARTESIAN_POINT('Ctrl Pts',(1.58625204782377,-3.60078830222637,53.0660509374768));
#22736=CARTESIAN_POINT('Ctrl Pts',(1.47946569731972,-3.64597272201073,53.0601809968447));
#22737=CARTESIAN_POINT('Ctrl Pts',(1.37077627475081,-3.68638866705347,53.0543110562125));
#22738=CARTESIAN_POINT('Ctrl Pts',(1.26219683913274,-3.72676371366787,53.048447055596));
#22739=CARTESIAN_POINT('Ctrl Pts',(1.15171854657812,-3.76237974113116,53.0425830549794));
#22740=CARTESIAN_POINT('Ctrl Pts',(1.03979633838236,-3.79306110874668,53.0367190543629));
#22741=CARTESIAN_POINT('Ctrl Pts',(0.924740451585198,-3.82460151539216,
53.0306908692334));
#22742=CARTESIAN_POINT('Ctrl Pts',(0.80815899767297,-3.85092665468197,53.0246626841038));
#22743=CARTESIAN_POINT('Ctrl Pts',(0.690565662773502,-3.87189980053696,
53.0186344989742));
#22744=CARTESIAN_POINT('Ctrl Pts',(0.576303884167373,-3.89227875271488,
53.0127770993584));
#22745=CARTESIAN_POINT('Ctrl Pts',(0.461087223141258,-3.90760481946477,
53.0069196997425));
#22746=CARTESIAN_POINT('Ctrl Pts',(0.345398728597537,-3.91780406838872,
53.0010623001266));
#22747=CARTESIAN_POINT('Ctrl Pts',(0.229726944965099,-3.92800184405688,
52.9952057465973));
#22748=CARTESIAN_POINT('Ctrl Pts',(0.113583874145427,-3.93307423829894,
52.989349193068));
#22749=CARTESIAN_POINT('Ctrl Pts',(-0.00254215567874407,-3.932999178419,
52.9834926395388));
#22750=CARTESIAN_POINT('Ctrl Pts',(-0.118679387937313,-3.93292411129818,
52.97763552104));
#22751=CARTESIAN_POINT('Ctrl Pts',(-0.234799163415466,-3.92770060319777,
52.9717784025413));
#22752=CARTESIAN_POINT('Ctrl Pts',(-0.35041369833918,-3.91735870709031,
52.9659212840426));
#22753=CARTESIAN_POINT('Ctrl Pts',(-0.471938876023687,-3.90648809499225,
52.9597647279769));
#22754=CARTESIAN_POINT('Ctrl Pts',(-0.592905280379541,-3.88996194967868,
52.9536081719111));
#22755=CARTESIAN_POINT('Ctrl Pts',(-0.712754689367659,-3.86787664653159,
52.9474516158453));
#22756=CARTESIAN_POINT('Ctrl Pts',(-0.82694483895059,-3.84683420592847,
52.941585770832));
#22757=CARTESIAN_POINT('Ctrl Pts',(-0.940120674119461,-3.82074576729556,
52.9357199258187));
#22758=CARTESIAN_POINT('Ctrl Pts',(-1.05181287110385,-3.78974651977943,
52.9298540808053));
#22759=CARTESIAN_POINT('Ctrl Pts',(-1.16358186502298,-3.75872595790784,
52.9239842025745));
#22760=CARTESIAN_POINT('Ctrl Pts',(-1.27386479835553,-3.72278799109742,
52.9181143243438));
#22761=CARTESIAN_POINT('Ctrl Pts',(-1.38221051337374,-3.6821166598465,52.912244446113));
#22762=CARTESIAN_POINT('Ctrl Pts',(-1.49070986372734,-3.64138765623062,
52.9063662443346));
#22763=CARTESIAN_POINT('Ctrl Pts',(-1.5972661367457,-3.59591205639966,52.9004880425563));
#22764=CARTESIAN_POINT('Ctrl Pts',(-1.7014510229078,-3.54592067263864,52.894609840778));
#22765=CARTESIAN_POINT('Ctrl Pts',(-1.716618162216,-3.53864297325589,52.8937540976032));
#22766=CARTESIAN_POINT('Ctrl Pts',(-1.73173509228498,-3.53126964581346,
52.8928983544283));
#22767=CARTESIAN_POINT('Ctrl Pts',(-1.74680054228167,-3.52380147929541,
52.8920426112535));
#22768=CARTESIAN_POINT('Ctrl Pts',(-1.85027375514464,-3.47250827637161,
52.8861651568326));
#22769=CARTESIAN_POINT('Ctrl Pts',(-1.95165540109902,-3.41656954182265,
52.8802877024118));
#22770=CARTESIAN_POINT('Ctrl Pts',(-2.05049996068643,-3.35617921321627,
52.8744102479909));
#22771=CARTESIAN_POINT('Ctrl Pts',(-2.14921819519744,-3.29586606450635,
52.8685403050597));
#22772=CARTESIAN_POINT('Ctrl Pts',(-2.2454054428876,-3.23111284935119,52.8626703621284));
#22773=CARTESIAN_POINT('Ctrl Pts',(-2.33863856043279,-3.16216044559047,
52.8568004191971));
#22774=CARTESIAN_POINT('Ctrl Pts',(-2.43177733164452,-3.09327781753444,
52.8509364162967));
#22775=CARTESIAN_POINT('Ctrl Pts',(-2.52196758939371,-3.02020469736552,
52.8450724133962));
#22776=CARTESIAN_POINT('Ctrl Pts',(-2.60881366733854,-2.94322616343149,
52.8392084104958));
#22777=CARTESIAN_POINT('Ctrl Pts',(-2.69809127679203,-2.86409237119243,
52.8331802262281));
#22778=CARTESIAN_POINT('Ctrl Pts',(-2.78383429546973,-2.78083147187155,
52.8271520419603));
#22779=CARTESIAN_POINT('Ctrl Pts',(-2.86564755563438,-2.69379900640095,
52.8211238576926));
#22780=CARTESIAN_POINT('Ctrl Pts',(-2.94514299240547,-2.6092322278381,52.8152664558444));
#22781=CARTESIAN_POINT('Ctrl Pts',(-3.0209280456164,-2.52110503640395,52.8094090539962));
#22782=CARTESIAN_POINT('Ctrl Pts',(-3.09267687884802,-2.42978162044224,
52.8035516521479));
#22783=CARTESIAN_POINT('Ctrl Pts',(-3.16441534786508,-2.33847139626965,
52.7976950964092));
#22784=CARTESIAN_POINT('Ctrl Pts',(-3.2321185015145,-2.2439661899538,52.7918385406705));
#22785=CARTESIAN_POINT('Ctrl Pts',(-3.29550105450613,-2.14666294507291,
52.7859819849317));
#22786=CARTESIAN_POINT('Ctrl Pts',(-3.35888972160454,-2.04935031397446,
52.7801248642488));
#22787=CARTESIAN_POINT('Ctrl Pts',(-3.4179567343685,-1.94923945340892,52.7742677435658));
#22788=CARTESIAN_POINT('Ctrl Pts',(-3.47246076316776,-1.84675532983134,
52.7684106228828));
#22789=CARTESIAN_POINT('Ctrl Pts',(-3.52975118875137,-1.73903193424627,
52.7622540699818));
#22790=CARTESIAN_POINT('Ctrl Pts',(-3.58199950153473,-1.62868664782208,
52.7560975170808));
#22791=CARTESIAN_POINT('Ctrl Pts',(-3.62898143730125,-1.51623966697981,
52.7499409641798));
#22792=CARTESIAN_POINT('Ctrl Pts',(-3.67374493674294,-1.40910231126998,
52.7440751170653));
#22793=CARTESIAN_POINT('Ctrl Pts',(-3.71372795068742,-1.30005762113249,
52.7382092699509));
#22794=CARTESIAN_POINT('Ctrl Pts',(-3.74878729262083,-1.18957254284247,
52.7323434228364));
#22795=CARTESIAN_POINT('Ctrl Pts',(-3.78387074035469,-1.07901149817362,
52.7264735425333));
#22796=CARTESIAN_POINT('Ctrl Pts',(-3.81402366807081,-0.967008490512607,
52.7206036622302));
#22797=CARTESIAN_POINT('Ctrl Pts',(-3.83915373006062,-0.854041940985162,
52.7147337819271));
#22798=CARTESIAN_POINT('Ctrl Pts',(-3.8643194264966,-0.740915204808353,
52.7088555781295));
#22799=CARTESIAN_POINT('Ctrl Pts',(-3.88444797384919,-0.626822604870012,
52.7029773743318));
#22800=CARTESIAN_POINT('Ctrl Pts',(-3.8994986835627,-0.51224897939661,52.6970991705342));
#22801=CARTESIAN_POINT('Ctrl Pts',(-3.90168971103587,-0.49556976852276,
52.6962434430463));
#22802=CARTESIAN_POINT('Ctrl Pts',(-3.90377321667196,-0.478880364767715,
52.6953877155585));
#22803=CARTESIAN_POINT('Ctrl Pts',(-3.90574916697184,-0.462182263505258,
52.6945319880707));
#22804=CARTESIAN_POINT('Ctrl Pts',(-3.9237852991702,-0.309764886484231,
52.6867210557321));
#22805=CARTESIAN_POINT('Ctrl Pts',(-3.93290184813808,-0.156271669277873,
52.6789101233936));
#22806=CARTESIAN_POINT('Ctrl Pts',(-3.93299921172394,-0.00249009617154345,
52.671099191055));
#22807=CARTESIAN_POINT('',(-3.93076159747888,-0.00108900750095069,51.4210992232121));
#22808=CARTESIAN_POINT('Ctrl Pts',(-3.93299921172447,-0.00249009532928107,
52.6710991910122));
#22809=CARTESIAN_POINT('Ctrl Pts',(-3.93307142957185,0.111574909923686,
52.6653055577425));
#22810=CARTESIAN_POINT('Ctrl Pts',(-3.92817727933913,0.22583195648946,52.6595119244728));
#22811=CARTESIAN_POINT('Ctrl Pts',(-3.91829309654896,0.339806135225414,
52.6537182912031));
#22812=CARTESIAN_POINT('Ctrl Pts',(-3.90841996795221,0.453652848429453,
52.6479311373707));
#22813=CARTESIAN_POINT('Ctrl Pts',(-3.89356793662517,0.567216902680455,
52.6421439835383));
#22814=CARTESIAN_POINT('Ctrl Pts',(-3.87376536650919,0.680022709351676,
52.6363568297059));
#22815=CARTESIAN_POINT('Ctrl Pts',(-3.85389952520209,0.793188941852033,
52.6305511853385));
#22816=CARTESIAN_POINT('Ctrl Pts',(-3.82905145330541,0.90559164150953,52.624745540971));
#22817=CARTESIAN_POINT('Ctrl Pts',(-3.79930239470142,1.01675479522654,52.6189398966036));
#22818=CARTESIAN_POINT('Ctrl Pts',(-3.76968670854771,1.12741957679704,52.6131602803881));
#22819=CARTESIAN_POINT('Ctrl Pts',(-3.73521399798968,1.23685548968949,52.6073806641725));
#22820=CARTESIAN_POINT('Ctrl Pts',(-3.69601554610006,1.34460331807814,52.6016010479569));
#22821=CARTESIAN_POINT('Ctrl Pts',(-3.65682487407717,1.45232976134301,52.5958225788439));
#22822=CARTESIAN_POINT('Ctrl Pts',(-3.61291046997645,1.55836838693821,52.5900441097309));
#22823=CARTESIAN_POINT('Ctrl Pts',(-3.56445294361742,1.66227681591761,52.5842656406178));
#22824=CARTESIAN_POINT('Ctrl Pts',(-3.51599259796712,1.76619129035884,52.5784868353096));
#22825=CARTESIAN_POINT('Ctrl Pts',(-3.46298878515761,1.86797493726591,52.5727080300014));
#22826=CARTESIAN_POINT('Ctrl Pts',(-3.40566918253362,1.96720777223476,52.5669292246932));
#22827=CARTESIAN_POINT('Ctrl Pts',(-3.34788488095486,2.0672451032674,52.5611035697094));
#22828=CARTESIAN_POINT('Ctrl Pts',(-3.28571470762259,2.16468969157742,52.5552779147256));
#22829=CARTESIAN_POINT('Ctrl Pts',(-3.21943707636124,2.25914008227702,52.5494522597418));
#22830=CARTESIAN_POINT('Ctrl Pts',(-3.15359986645065,2.35296284088024,52.5436653168059));
#22831=CARTESIAN_POINT('Ctrl Pts',(-3.08370993337709,2.44383077506574,52.5378783738701));
#22832=CARTESIAN_POINT('Ctrl Pts',(-3.01008058582062,2.53138378498122,52.5320914309342));
#22833=CARTESIAN_POINT('Ctrl Pts',(-2.93571241738874,2.61981533033913,52.5262464199265));
#22834=CARTESIAN_POINT('Ctrl Pts',(-2.85752968143504,2.70486473577434,52.5204014089187));
#22835=CARTESIAN_POINT('Ctrl Pts',(-2.77589224681784,2.78620014249814,52.514556397911));
#22836=CARTESIAN_POINT('Ctrl Pts',(-2.69425481220065,2.86753554922193,52.5087113869032));
#22837=CARTESIAN_POINT('Ctrl Pts',(-2.60916304801192,2.9451567104361,52.5028663758955));
#22838=CARTESIAN_POINT('Ctrl Pts',(-2.52100877130662,3.01877521107404,52.4970213648877));
#22839=CARTESIAN_POINT('Ctrl Pts',(-2.43236539580103,3.09280216291465,52.4911439245076));
#22840=CARTESIAN_POINT('Ctrl Pts',(-2.3403133601219,3.16304276857767,52.4852664841274));
#22841=CARTESIAN_POINT('Ctrl Pts',(-2.24520969962729,3.2291674476093,52.4793890437472));
#22842=CARTESIAN_POINT('Ctrl Pts',(-2.15022758345157,3.29520761802126,52.4735191148496));
#22843=CARTESIAN_POINT('Ctrl Pts',(-2.05220193435526,3.35714208973021,52.467649185952));
#22844=CARTESIAN_POINT('Ctrl Pts',(-1.95152372976844,3.41468067791861,52.4617792570543));
#22845=CARTESIAN_POINT('Ctrl Pts',(-1.85094740533806,3.47216104059148,52.4559152681641));
#22846=CARTESIAN_POINT('Ctrl Pts',(-1.74772422086267,3.52525416478485,52.4500512792738));
#22847=CARTESIAN_POINT('Ctrl Pts',(-1.64227453274059,3.57371282549559,52.4441872903835));
#22848=CARTESIAN_POINT('Ctrl Pts',(-1.53387209242361,3.62352840265933,52.4381591008552));
#22849=CARTESIAN_POINT('Ctrl Pts',(-1.42311697650877,3.66844587849009,52.432130911327));
#22850=CARTESIAN_POINT('Ctrl Pts',(-1.3104938323533,3.70824687896639,52.4261027217987));
#22851=CARTESIAN_POINT('Ctrl Pts',(-1.2010617303594,3.74692016567174,52.4202453338147));
#22852=CARTESIAN_POINT('Ctrl Pts',(-1.08986645002449,3.78076287615063,52.4143879458307));
#22853=CARTESIAN_POINT('Ctrl Pts',(-0.977372607493188,3.80962357538405,
52.4085305578467));
#22854=CARTESIAN_POINT('Ctrl Pts',(-0.864895013389615,3.83848010602501,
52.4026740158943));
#22855=CARTESIAN_POINT('Ctrl Pts',(-0.751119629522808,3.86235595386983,
52.3968174739419));
#22856=CARTESIAN_POINT('Ctrl Pts',(-0.636524707289445,3.88114999671619,
52.3909609319895));
#22857=CARTESIAN_POINT('Ctrl Pts',(-0.521918728982694,3.89994585280448,
52.3851038250002));
#22858=CARTESIAN_POINT('Ctrl Pts',(-0.406493462208433,3.91365886247838,
52.3792467180109));
#22859=CARTESIAN_POINT('Ctrl Pts',(-0.290735090501276,3.92223942501618,
52.3733896110216));
#22860=CARTESIAN_POINT('Ctrl Pts',(-0.169058159789764,3.93125869937171,
52.3672330385786));
#22861=CARTESIAN_POINT('Ctrl Pts',(-0.0470136672297076,3.93460677047019,
52.3610764661355));
#22862=CARTESIAN_POINT('Ctrl Pts',(0.0748319178295033,3.93228803422053,
52.3549198936924));
#22863=CARTESIAN_POINT('Ctrl Pts',(0.190923453384458,3.93007879823025,52.3490540599134));
#22864=CARTESIAN_POINT('Ctrl Pts',(0.306834022036394,3.922725829333,52.3431882261343));
#22865=CARTESIAN_POINT('Ctrl Pts',(0.422078572658463,3.91028626554407,52.3373223923553));
#22866=CARTESIAN_POINT('Ctrl Pts',(0.537402364764424,3.8978381483833,52.3314525252629));
#22867=CARTESIAN_POINT('Ctrl Pts',(0.652058820325884,3.88029653418258,52.3255826581706));
#22868=CARTESIAN_POINT('Ctrl Pts',(0.765572875668805,3.85776971474973,52.3197127910783));
#22869=CARTESIAN_POINT('Ctrl Pts',(0.879247899326109,3.83521095121848,52.3138346002361));
#22870=CARTESIAN_POINT('Ctrl Pts',(0.991776891409228,3.80765297422279,52.3079564093938));
#22871=CARTESIAN_POINT('Ctrl Pts',(1.10269973352898,3.77525393817093,52.3020782185516));
#22872=CARTESIAN_POINT('Ctrl Pts',(1.1188493639481,3.7705368533201,52.301222392936));
#22873=CARTESIAN_POINT('Ctrl Pts',(1.13496498330523,3.76571723345069,52.3003665673205));
#22874=CARTESIAN_POINT('Ctrl Pts',(1.15104520906026,3.7607956507499,52.2995107417049));
#22875=CARTESIAN_POINT('Ctrl Pts',(1.26147768457721,3.72699621476005,52.2936332781186));
#22876=CARTESIAN_POINT('Ctrl Pts',(1.37060118244447,3.68827312874922,52.2877558145322));
#22877=CARTESIAN_POINT('Ctrl Pts',(1.47794459146711,3.64474536621601,52.2818783509458));
#22878=CARTESIAN_POINT('Ctrl Pts',(1.58515081259428,3.60127323338742,52.2760083989232));
#22879=CARTESIAN_POINT('Ctrl Pts',(1.69058109043122,3.55300878965019,52.2701384469006));
#22880=CARTESIAN_POINT('Ctrl Pts',(1.79377876580033,3.50012096067605,52.264268494878));
#22881=CARTESIAN_POINT('Ctrl Pts',(1.89687200998751,3.44728665169128,52.2584044829701));
#22882=CARTESIAN_POINT('Ctrl Pts',(1.99773678082893,3.38983845113601,52.2525404710621));
#22883=CARTESIAN_POINT('Ctrl Pts',(2.09593634936964,3.3279933622817,52.2466764591542));
#22884=CARTESIAN_POINT('Ctrl Pts',(2.19688511427671,3.26441685753541,52.2406482782945));
#22885=CARTESIAN_POINT('Ctrl Pts',(2.29501682801645,3.19619379818832,52.2346200974348));
#22886=CARTESIAN_POINT('Ctrl Pts',(2.38988380759784,3.12361079300569,52.2285919165752));
#22887=CARTESIAN_POINT('Ctrl Pts',(2.48206333307946,3.05308396686144,52.2227345059818));
#22888=CARTESIAN_POINT('Ctrl Pts',(2.57116026332614,2.97844116882488,52.2168770953884));
#22889=CARTESIAN_POINT('Ctrl Pts',(2.6567939176076,2.89998880676516,52.211019684795));
#22890=CARTESIAN_POINT('Ctrl Pts',(2.74241520037575,2.82154777873584,52.2051631204231));
#22891=CARTESIAN_POINT('Ctrl Pts',(2.82457389804232,2.73929855968457,52.1993065560511));
#22892=CARTESIAN_POINT('Ctrl Pts',(2.90292402008163,2.65358646620626,52.1934499916792));
#22893=CARTESIAN_POINT('Ctrl Pts',(2.98128169842472,2.56786610641517,52.1875928624838));
#22894=CARTESIAN_POINT('Ctrl Pts',(3.05582979263931,2.47868251277184,52.1817357332885));
#22895=CARTESIAN_POINT('Ctrl Pts',(3.12626113059767,2.3864157943062,52.1758786040932));
#22896=CARTESIAN_POINT('Ctrl Pts',(3.2002928563174,2.289432482722,52.1697220636289));
#22897=CARTESIAN_POINT('Ctrl Pts',(3.26977549092988,2.18904289665158,52.1635655231647));
#22898=CARTESIAN_POINT('Ctrl Pts',(3.33440323090798,2.08572387762866,52.1574089827004));
#22899=CARTESIAN_POINT('Ctrl Pts',(3.39597952847646,1.98728313589773,52.1515431274539));
#22900=CARTESIAN_POINT('Ctrl Pts',(3.45314875494368,1.88618366667587,52.1456772722074));
#22901=CARTESIAN_POINT('Ctrl Pts',(3.50569375606319,1.78286294725632,52.1398114169609));
#22902=CARTESIAN_POINT('Ctrl Pts',(3.55827488439563,1.67947118987785,52.1339415286571));
#22903=CARTESIAN_POINT('Ctrl Pts',(3.60622528644685,1.57385551582131,52.1280716403532));
#22904=CARTESIAN_POINT('Ctrl Pts',(3.64937610872275,1.46647298545984,52.1222017520494));
#22905=CARTESIAN_POINT('Ctrl Pts',(3.69258811709727,1.35893819106849,52.1163235404844));
#22906=CARTESIAN_POINT('Ctrl Pts',(3.73098682975768,1.24963192870861,52.1104453289194));
#22907=CARTESIAN_POINT('Ctrl Pts',(3.76445332125774,1.13902598393165,52.1045671173544));
#22908=CARTESIAN_POINT('Ctrl Pts',(3.76932489620612,1.12292554658178,52.1037114510769));
#22909=CARTESIAN_POINT('Ctrl Pts',(3.77409204910857,1.10679758562085,52.1028557847995));
#22910=CARTESIAN_POINT('Ctrl Pts',(3.77875450399893,1.09064357079098,52.102000118522));
#22911=CARTESIAN_POINT('Ctrl Pts',(3.8107804355628,0.979683275069462,52.0961226333157));
#22912=CARTESIAN_POINT('Ctrl Pts',(3.83796732377089,0.867129288955818,52.0902451481093));
#22913=CARTESIAN_POINT('Ctrl Pts',(3.86015742648859,0.753441200575642,52.084367662903));
#22914=CARTESIAN_POINT('Ctrl Pts',(3.88231917084835,0.639898402532647,52.0784976889656));
#22915=CARTESIAN_POINT('Ctrl Pts',(3.89949675111667,0.525224785894342,52.0726277150282));
#22916=CARTESIAN_POINT('Ctrl Pts',(3.91158215895138,0.409895125334751,52.0667577410908));
#22917=CARTESIAN_POINT('Ctrl Pts',(3.92365533751389,0.294682167316825,52.0608937070034));
#22918=CARTESIAN_POINT('Ctrl Pts',(3.93064655066653,0.178814893778597,52.0550296729159));
#22919=CARTESIAN_POINT('Ctrl Pts',(3.93249894675403,0.0627776534951526,
52.0491656388285));
#22920=CARTESIAN_POINT('Ctrl Pts',(3.9344031927486,-0.0565075531206359,
52.0431374661831));
#22921=CARTESIAN_POINT('Ctrl Pts',(3.93087660300224,-0.175971946927321,
52.0371092935377));
#22922=CARTESIAN_POINT('Ctrl Pts',(3.92191463987212,-0.295083983903956,
52.0310811208923));
#22923=CARTESIAN_POINT('Ctrl Pts',(3.91320651152266,-0.410822342888443,
52.0252236876105));
#22924=CARTESIAN_POINT('Ctrl Pts',(3.89936680872289,-0.526227598819512,
52.0193662543286));
#22925=CARTESIAN_POINT('Ctrl Pts',(3.88044418295405,-0.640813500933015,
52.0135088210468));
#22926=CARTESIAN_POINT('Ctrl Pts',(3.86152429045182,-0.755382851758902,
52.0076522338382));
#22927=CARTESIAN_POINT('Ctrl Pts',(3.83752300214969,-0.86913267723255,52.0017956466296));
#22928=CARTESIAN_POINT('Ctrl Pts',(3.80854051076383,-0.981584524058269,
51.995939059421));
#22929=CARTESIAN_POINT('Ctrl Pts',(3.77955522363123,-1.09404721836014,51.9900819072667));
#22930=CARTESIAN_POINT('Ctrl Pts',(3.74558788117118,-1.20521128565554,51.9842247551123));
#22931=CARTESIAN_POINT('Ctrl Pts',(3.70678902513152,-1.31461177659582,51.978367602958));
#22932=CARTESIAN_POINT('Ctrl Pts',(3.66600717434945,-1.42960368492558,51.9722110939898));
#22933=CARTESIAN_POINT('Ctrl Pts',(3.61988704088369,-1.54264649743468,51.9660545850215));
#22934=CARTESIAN_POINT('Ctrl Pts',(3.56866092694071,-1.65322357487626,51.9598980760533));
#22935=CARTESIAN_POINT('Ctrl Pts',(3.51985304709199,-1.75858063389108,51.9540321977565));
#22936=CARTESIAN_POINT('Ctrl Pts',(3.46641049709761,-1.86169909325234,51.9481663194596));
#22937=CARTESIAN_POINT('Ctrl Pts',(3.408581048649,-1.96215805550695,51.9423004411628));
#22938=CARTESIAN_POINT('Ctrl Pts',(3.35071183955772,-2.06268608833042,51.9364305297808));
#22939=CARTESIAN_POINT('Ctrl Pts',(3.28844994683734,-2.16055063593432,51.9305606183988));
#22940=CARTESIAN_POINT('Ctrl Pts',(3.22208593325395,-2.25536055625857,51.9246907070167));
#22941=CARTESIAN_POINT('Ctrl Pts',(3.15562781972929,-2.35030491100672,51.9188124724745));
#22942=CARTESIAN_POINT('Ctrl Pts',(3.08505622921332,-2.44218567024063,51.9129342379323));
#22943=CARTESIAN_POINT('Ctrl Pts',(3.01070133586929,-2.53064546434202,51.9070560033901));
#22944=CARTESIAN_POINT('Ctrl Pts',(2.99987992166008,-2.5435196684432,51.9062005007065));
#22945=CARTESIAN_POINT('Ctrl Pts',(2.98897843458229,-2.55632147826902,51.9053449980228));
#22946=CARTESIAN_POINT('Ctrl Pts',(2.97799795422667,-2.56904986028331,51.9044894953391));
#22947=CARTESIAN_POINT('Ctrl Pts',(2.90256151038189,-2.65649447508698,51.898612149534));
#22948=CARTESIAN_POINT('Ctrl Pts',(2.82314659863413,-2.74075702202623,51.8927348037289));
#22949=CARTESIAN_POINT('Ctrl Pts',(2.74005194549637,-2.82145429450514,51.8868574579238));
#22950=CARTESIAN_POINT('Ctrl Pts',(2.65706349213867,-2.90204843119534,51.8809876237071));
#22951=CARTESIAN_POINT('Ctrl Pts',(2.57040494365269,-2.97908607059595,51.8751177894904));
#22952=CARTESIAN_POINT('Ctrl Pts',(2.48041491919786,-3.05221736261044,51.8692479552737));
#22953=CARTESIAN_POINT('Ctrl Pts',(2.39051596047105,-3.12527464915166,51.8633840610568));
#22954=CARTESIAN_POINT('Ctrl Pts',(2.29729255013922,-3.19443319290352,51.8575201668399));
#22955=CARTESIAN_POINT('Ctrl Pts',(2.20111927658947,-3.25938075870651,51.8516562726229));
#22956=CARTESIAN_POINT('Ctrl Pts',(2.10225082631248,-3.3261484265127,51.8456280476035));
#22957=CARTESIAN_POINT('Ctrl Pts',(2.00026504762229,-3.38846529382579,51.839599822584));
#22958=CARTESIAN_POINT('Ctrl Pts',(1.89560468220114,-3.4460371281832,51.8335715975646));
#22959=CARTESIAN_POINT('Ctrl Pts',(1.79391197486553,-3.50197650579307,51.8277143036388));
#22960=CARTESIAN_POINT('Ctrl Pts',(1.68969470443012,-3.55343611481209,51.821857009713));
#22961=CARTESIAN_POINT('Ctrl Pts',(1.58338669623113,-3.60019104634716,51.8159997157871));
#22962=CARTESIAN_POINT('Ctrl Pts',(1.4770940361507,-3.64693922768301,51.8101432675026));
#22963=CARTESIAN_POINT('Ctrl Pts',(1.36871161605367,-3.68898391617528,51.8042868192181));
#22964=CARTESIAN_POINT('Ctrl Pts',(1.25869489020222,-3.72614763172084,51.7984303709335));
#22965=CARTESIAN_POINT('Ctrl Pts',(1.14866754058109,-3.76331493598211,51.7925733571208));
#22966=CARTESIAN_POINT('Ctrl Pts',(1.0370059623169,-3.79560019830782,51.7867163433081));
#22967=CARTESIAN_POINT('Ctrl Pts',(0.924181807461963,-3.82287548669275,
51.7808593294954));
#22968=CARTESIAN_POINT('Ctrl Pts',(0.805584680066861,-3.85154639369386,
51.7747026247172));
#22969=CARTESIAN_POINT('Ctrl Pts',(0.685703346159854,-3.87468092942088,
51.7685459199389));
#22970=CARTESIAN_POINT('Ctrl Pts',(0.565097510560029,-3.89219138835166,
51.7623892151606));
#22971=CARTESIAN_POINT('Ctrl Pts',(0.450191432651099,-3.9088743137517,51.7565234724675));
#22972=CARTESIAN_POINT('Ctrl Pts',(0.334628190883094,-3.92045260275053,
51.7506577297744));
#22973=CARTESIAN_POINT('Ctrl Pts',(0.218895662112313,-3.92690382987773,
51.7447919870813));
#22974=CARTESIAN_POINT('Ctrl Pts',(0.103083540709917,-3.93335949370177,
51.7389222103461));
#22975=CARTESIAN_POINT('Ctrl Pts',(-0.0128976881731574,-3.93468106983234,
51.7330524336109));
#22976=CARTESIAN_POINT('Ctrl Pts',(-0.128561691980987,-3.93089822958506,
51.7271826568757));
#22977=CARTESIAN_POINT('Ctrl Pts',(-0.244389746367142,-3.92711002399412,
51.7213045548168));
#22978=CARTESIAN_POINT('Ctrl Pts',(-0.359899268433259,-3.91820298742322,
51.7154264527579));
#22979=CARTESIAN_POINT('Ctrl Pts',(-0.47461057168177,-3.90425841937338,
51.709548350699));
#22980=CARTESIAN_POINT('Ctrl Pts',(-0.491325050230513,-3.90222656918129,
51.7086918578514));
#22981=CARTESIAN_POINT('Ctrl Pts',(-0.508022602959161,-3.90008785421182,
51.7078353650038));
#22982=CARTESIAN_POINT('Ctrl Pts',(-0.524701769303992,-3.89784261525389,
51.7069788721562));
#22983=CARTESIAN_POINT('Ctrl Pts',(-0.63916023950688,-3.88243497370565,
51.7011013085509));
#22984=CARTESIAN_POINT('Ctrl Pts',(-0.753127073525721,-3.8619562765558,
51.6952237449456));
#22985=CARTESIAN_POINT('Ctrl Pts',(-0.866118077357017,-3.83644737694594,
51.6893461813402));
#22986=CARTESIAN_POINT('Ctrl Pts',(-0.978964668335136,-3.81097108004647,
51.6834761297996));
#22987=CARTESIAN_POINT('Ctrl Pts',(-1.09083751071811,-3.78047745655816,
51.677606078259));
#22988=CARTESIAN_POINT('Ctrl Pts',(-1.20125855487867,-3.74505899610818,
51.6717360267183));
#22989=CARTESIAN_POINT('Ctrl Pts',(-1.31156784853888,-3.70967638055269,
51.665871915904));
#22990=CARTESIAN_POINT('Ctrl Pts',(-1.4204278761091,-3.66937896757605,51.6600078050896));
#22991=CARTESIAN_POINT('Ctrl Pts',(-1.52737244212953,-3.62430992369904,
51.6541436942752));
#22992=CARTESIAN_POINT('Ctrl Pts',(-1.63730849496429,-3.57798019444538,
51.648115550721));
#22993=CARTESIAN_POINT('Ctrl Pts',(-1.74521990979877,-3.52660803868946,
51.6420874071667));
#22994=CARTESIAN_POINT('Ctrl Pts',(-1.85061840581349,-3.47040350911308,
51.6360592636125));
#22995=CARTESIAN_POINT('Ctrl Pts',(-1.95303343001351,-3.41578993800566,
51.6302017562349));
#22996=CARTESIAN_POINT('Ctrl Pts',(-2.05307550368128,-3.35661410648841,
51.6243442488574));
#22997=CARTESIAN_POINT('Ctrl Pts',(-2.15031920814855,-3.29311650311182,
51.6184867414798));
#22998=CARTESIAN_POINT('Ctrl Pts',(-2.2475488482417,-3.2296280834048,51.6126300812746));
#22999=CARTESIAN_POINT('Ctrl Pts',(-2.3419805786639,-3.1618193602502,51.6067734210694));
#23000=CARTESIAN_POINT('Ctrl Pts',(-2.43321688783559,-3.08997485050473,
51.6009167608641));
#23001=CARTESIAN_POINT('Ctrl Pts',(-2.52446197956638,-3.01812342488707,
51.595059536887));
#23002=CARTESIAN_POINT('Ctrl Pts',(-2.61251071449089,-2.94223569559399,
51.5892023129099));
#23003=CARTESIAN_POINT('Ctrl Pts',(-2.69699823013746,-2.86263681710333,
51.5833450889329));
#23004=CARTESIAN_POINT('Ctrl Pts',(-2.78580125776636,-2.77897213183307,
51.5771886856029));
#23005=CARTESIAN_POINT('Ctrl Pts',(-2.87066927267329,-2.69120750080115,
51.5710322822729));
#23006=CARTESIAN_POINT('Ctrl Pts',(-2.95122308578683,-2.59976370040027,
51.564875878943));
#23007=CARTESIAN_POINT('Ctrl Pts',(-3.02797640016931,-2.51263418425181,
51.5590099324162));
#23008=CARTESIAN_POINT('Ctrl Pts',(-3.10081308566887,-2.42216510162187,
51.5531439858895));
#23009=CARTESIAN_POINT('Ctrl Pts',(-3.16944777765645,-2.32875283890512,
51.5472780393627));
#23010=CARTESIAN_POINT('Ctrl Pts',(-3.23812964437753,-2.2352763710689,51.5414080609906));
#23011=CARTESIAN_POINT('Ctrl Pts',(-3.30260353793884,-2.13885303694543,
51.5355380826185));
#23012=CARTESIAN_POINT('Ctrl Pts',(-3.36262857005296,-2.03990639487788,
51.5296681042464));
#23013=CARTESIAN_POINT('Ctrl Pts',(-3.42273869087957,-1.94081949062167,
51.5237898048642));
#23014=CARTESIAN_POINT('Ctrl Pts',(-3.4783871690931,-1.83920250123322,51.5179115054819));
#23015=CARTESIAN_POINT('Ctrl Pts',(-3.52937998787692,-1.73550162811044,
51.5120332060996));
#23016=CARTESIAN_POINT('Ctrl Pts',(-3.53679678114902,-1.72041856432947,
51.5111782203909));
#23017=CARTESIAN_POINT('Ctrl Pts',(-3.54411516846418,-1.70529144587849,
51.5103232346821));
#23018=CARTESIAN_POINT('Ctrl Pts',(-3.55133463990173,-1.69012167474241,
51.5094682489733));
#23019=CARTESIAN_POINT('Ctrl Pts',(-3.60486774011933,-1.57763630991621,
51.5031284447331));
#23020=CARTESIAN_POINT('Ctrl Pts',(-3.65311231872581,-1.46248026746492,
51.4967886404929));
#23021=CARTESIAN_POINT('Ctrl Pts',(-3.69581538181708,-1.3451533977671,51.4904488362527));
#23022=CARTESIAN_POINT('Ctrl Pts',(-3.73837808187887,-1.22821217616282,
51.4841298706612));
#23023=CARTESIAN_POINT('Ctrl Pts',(-3.77543548111521,-1.10911464538009,
51.4778109050697));
#23024=CARTESIAN_POINT('Ctrl Pts',(-3.8067824973443,-0.988380502596623,
51.4714919394781));
#23025=CARTESIAN_POINT('Ctrl Pts',(-3.83806546245479,-0.867893054964066,
51.4651858853807));
#23026=CARTESIAN_POINT('Ctrl Pts',(-3.86366121578873,-0.745775955930149,
51.4588798312833));
#23027=CARTESIAN_POINT('Ctrl Pts',(-3.88341347034862,-0.622566316399284,
51.4525737771858));
#23028=CARTESIAN_POINT('Ctrl Pts',(-3.90310460269884,-0.499737941973974,
51.4462872368082));
#23029=CARTESIAN_POINT('Ctrl Pts',(-3.91698823758152,-0.375824071597219,
51.4400006964305));
#23030=CARTESIAN_POINT('Ctrl Pts',(-3.92495867402245,-0.251373043932732,
51.4337141560528));
#23031=CARTESIAN_POINT('Ctrl Pts',(-3.93028997762093,-0.168129646091341,
51.4295091848965));
#23032=CARTESIAN_POINT('Ctrl Pts',(-3.93297669174091,-0.0846462499726585,
51.4253042137402));
#23033=CARTESIAN_POINT('Ctrl Pts',(-3.93299984895417,-0.00109001217197362,
51.4210992425839));
#23034=CARTESIAN_POINT('',(-3.93427805355045,0.00340288565414877,50.1711036262703));
#23035=CARTESIAN_POINT('Ctrl Pts',(-3.92704610517626,-0.00108733974936265,
51.421099191055));
#23036=CARTESIAN_POINT('Ctrl Pts',(-3.92524730607414,0.72072979241773,51.3847186693002));
#23037=CARTESIAN_POINT('Ctrl Pts',(-3.3898856313511,2.75129080723824,51.2825012731509));
#23038=CARTESIAN_POINT('Ctrl Pts',(-0.136318537846259,4.63920340706317,
51.1144470026077));
#23039=CARTESIAN_POINT('Ctrl Pts',(3.81089992892979,2.6488745889284,50.9169363794247));
#23040=CARTESIAN_POINT('Ctrl Pts',(4.30110806150455,-1.74478063138574,50.719425756242));
#23041=CARTESIAN_POINT('Ctrl Pts',(0.887676967041259,-4.55539414744317,
50.5219151330588));
#23042=CARTESIAN_POINT('Ctrl Pts',(-3.01408004080397,-3.33156985104081,
50.3391410897352));
#23043=CARTESIAN_POINT('Ctrl Pts',(-3.92504487197984,-1.00631924839508,
50.2222039208056));
#23044=CARTESIAN_POINT('Ctrl Pts',(-3.93427805355045,0.00340288565414877,
50.1711036262703));
#23045=CARTESIAN_POINT('',(-3.89317704633887,0.578984810677012,50.1436634243168));
#23046=CARTESIAN_POINT('Ctrl Pts',(-3.93299849268476,0.00344333260814783,
50.1718402566183));
#23047=CARTESIAN_POINT('Ctrl Pts',(-3.93291481497374,0.099020597068333,
50.167553787606));
#23048=CARTESIAN_POINT('Ctrl Pts',(-3.92934717672993,0.194561546255428,
50.1632628550717));
#23049=CARTESIAN_POINT('Ctrl Pts',(-3.91516728110938,0.386429387633131,
50.1544929579965));
#23050=CARTESIAN_POINT('Ctrl Pts',(-3.90446908640162,0.482681821527946,
50.1500151960044));
#23051=CARTESIAN_POINT('Ctrl Pts',(-3.89023144643595,0.578436075258949,
50.1454016210458));
#23052=CARTESIAN_POINT('',(-2.81006454498411,-2.75173150089599,50.1419356690201));
#23053=CARTESIAN_POINT('Origin',(-1.041818884589E-14,0.,50.1419356690201));
#23054=CARTESIAN_POINT('',(-3.9296784706345,-0.000991769389231509,51.2377721674176));
#23055=CARTESIAN_POINT('Ctrl Pts',(-2.8100645449841,-2.751731500896,50.1419356690201));
#23056=CARTESIAN_POINT('Ctrl Pts',(-1.89942791543654,-3.68167241454335,
50.2077725434144));
#23057=CARTESIAN_POINT('Ctrl Pts',(0.902301753494953,-4.550726992117,50.3394462922028));
#23058=CARTESIAN_POINT('Ctrl Pts',(4.31098005768057,-1.72664187782764,50.5369569153859));
#23059=CARTESIAN_POINT('Ctrl Pts',(3.79825323790283,2.66550893609982,50.7344675385685));
#23060=CARTESIAN_POINT('Ctrl Pts',(-0.155736620608226,4.63846238854458,
50.9319781617517));
#23061=CARTESIAN_POINT('Ctrl Pts',(-3.39636166881464,2.73991008102441,51.0997463645569));
#23062=CARTESIAN_POINT('Ctrl Pts',(-3.92545006867067,0.715178458449969,
51.2016776929682));
#23063=CARTESIAN_POINT('Ctrl Pts',(-3.92705168969078,-0.00099070069027788,
51.2377721469851));
#23064=CARTESIAN_POINT('',(-3.93299916752078,-0.0025589609114662,52.4877721469424));
#23065=CARTESIAN_POINT('Ctrl Pts',(-3.9329998746137,-0.000993120693749547,
51.2377721932532));
#23066=CARTESIAN_POINT('Ctrl Pts',(-3.93296843644496,-0.125495927339958,
51.2440375667306));
#23067=CARTESIAN_POINT('Ctrl Pts',(-3.9270208887338,-0.249841356608365,
51.250302940208));
#23068=CARTESIAN_POINT('Ctrl Pts',(-3.91522722570074,-0.373476600514333,
51.2565683136855));
#23069=CARTESIAN_POINT('Ctrl Pts',(-3.90339148758525,-0.497552925623416,
51.2628560395147));
#23070=CARTESIAN_POINT('Ctrl Pts',(-3.88566793179864,-0.62091367922872,
51.269143765344));
#23071=CARTESIAN_POINT('Ctrl Pts',(-3.86217818230335,-0.74301324896671,
51.2754314911733));
#23072=CARTESIAN_POINT('Ctrl Pts',(-3.83864586316443,-0.865334095443862,
51.2817306120261));
#23073=CARTESIAN_POINT('Ctrl Pts',(-3.80932655851785,-0.986388887489586,
51.2880297328789));
#23074=CARTESIAN_POINT('Ctrl Pts',(-3.7743919075506,-1.10564674657713,51.2943288537316));
#23075=CARTESIAN_POINT('Ctrl Pts',(-3.73935297989382,-1.22526057930121,
51.3006467768753));
#23076=CARTESIAN_POINT('Ctrl Pts',(-3.698665276834,-1.34306644872994,51.306964700019));
#23077=CARTESIAN_POINT('Ctrl Pts',(-3.65254956116948,-1.45855089153609,
51.3132826231626));
#23078=CARTESIAN_POINT('Ctrl Pts',(-3.6191757588183,-1.54212662950981,51.3178548848142));
#23079=CARTESIAN_POINT('Ctrl Pts',(-3.58296010671762,-1.62448700139721,
51.3224271464657));
#23080=CARTESIAN_POINT('Ctrl Pts',(-3.54400104932148,-1.70544585443465,
51.3269994081173));
#23081=CARTESIAN_POINT('Ctrl Pts',(-3.49391243270941,-1.80953248337725,
51.3328778424589));
#23082=CARTESIAN_POINT('Ctrl Pts',(-3.43915265248908,-1.9115805427375,51.3387562768005));
#23083=CARTESIAN_POINT('Ctrl Pts',(-3.37991065530951,-2.01114220335742,
51.3446347111421));
#23084=CARTESIAN_POINT('Ctrl Pts',(-3.32074416718912,-2.11057696401308,
51.3505056529098));
#23085=CARTESIAN_POINT('Ctrl Pts',(-3.25710703292163,-2.20753127739272,
51.3563765946774));
#23086=CARTESIAN_POINT('Ctrl Pts',(-3.18923538862743,-2.30157916134261,
51.3622475364451));
#23087=CARTESIAN_POINT('Ctrl Pts',(-3.12143221147759,-2.39553217224034,
51.3681125557598));
#23088=CARTESIAN_POINT('Ctrl Pts',(-3.04940326135557,-2.48658425342008,
51.3739775750745));
#23089=CARTESIAN_POINT('Ctrl Pts',(-2.97342918260808,-2.57433639915508,
51.3798425943892));
#23090=CARTESIAN_POINT('Ctrl Pts',(-2.8953463533348,-2.66452420961294,51.3858704042605));
#23091=CARTESIAN_POINT('Ctrl Pts',(-2.81309640538219,-2.75122582878452,
51.3918982141318));
#23092=CARTESIAN_POINT('Ctrl Pts',(-2.72703019679274,-2.83404222018314,
51.3979260240031));
#23093=CARTESIAN_POINT('Ctrl Pts',(-2.64338206200348,-2.9145318430445,51.4037844794975));
#23094=CARTESIAN_POINT('Ctrl Pts',(-2.55612956890415,-2.99135134332138,
51.409642934992));
#23095=CARTESIAN_POINT('Ctrl Pts',(-2.46563325223476,-3.06417063256508,
51.4155013904864));
#23096=CARTESIAN_POINT('Ctrl Pts',(-2.37514981975917,-3.13697955433893,
51.4213590118975));
#23097=CARTESIAN_POINT('Ctrl Pts',(-2.28142380325412,-3.205789139162,51.4272166333085));
#23098=CARTESIAN_POINT('Ctrl Pts',(-2.18484895451548,-3.2703094725045,51.4330742547196));
#23099=CARTESIAN_POINT('Ctrl Pts',(-2.08826461186527,-3.33483614859925,
51.4389324519714));
#23100=CARTESIAN_POINT('Ctrl Pts',(-1.9888312231127,-3.39507250590266,51.4447906492233));
#23101=CARTESIAN_POINT('Ctrl Pts',(-1.88697106577822,-3.45077226094622,
51.4506488464751));
#23102=CARTESIAN_POINT('Ctrl Pts',(-1.77994849575477,-3.50929495608463,
51.4568039452106));
#23103=CARTESIAN_POINT('Ctrl Pts',(-1.6702471638846,-3.56280889739079,51.462959043946));
#23104=CARTESIAN_POINT('Ctrl Pts',(-1.55838412777636,-3.61108403534101,
51.4691141426814));
#23105=CARTESIAN_POINT('Ctrl Pts',(-1.45175807705138,-3.65709912206596,
51.4749810840126));
#23106=CARTESIAN_POINT('Ctrl Pts',(-1.34316855712051,-3.69835472153699,
51.4808480253438));
#23107=CARTESIAN_POINT('Ctrl Pts',(-1.2330809491863,-3.73470217992731,51.486714966675));
#23108=CARTESIAN_POINT('Ctrl Pts',(-1.12291755025563,-3.77107466211589,
51.492585947165));
#23109=CARTESIAN_POINT('Ctrl Pts',(-1.01125440538746,-3.80253216316647,
51.4984569276551));
#23110=CARTESIAN_POINT('Ctrl Pts',(-0.898568962357412,-3.82897673274309,
51.5043279081451));
#23111=CARTESIAN_POINT('Ctrl Pts',(-0.785723724867012,-3.85545880224527,
51.5102072140242));
#23112=CARTESIAN_POINT('Ctrl Pts',(-0.671853699931724,-3.87691367975029,
51.5160865199033));
#23113=CARTESIAN_POINT('Ctrl Pts',(-0.557443355508977,-3.89329499336987,
51.5219658257824));
#23114=CARTESIAN_POINT('Ctrl Pts',(-0.540940079127791,-3.89565793832485,
51.5228138942883));
#23115=CARTESIAN_POINT('Ctrl Pts',(-0.524425562563187,-3.89791540605198,
51.5236619627942));
#23116=CARTESIAN_POINT('Ctrl Pts',(-0.507901260517054,-3.90006734679867,
51.5245100313001));
#23117=CARTESIAN_POINT('Ctrl Pts',(-0.393396833325279,-3.91497912593838,
51.5303866848625));
#23118=CARTESIAN_POINT('Ctrl Pts',(-0.27804693711552,-3.9248684390782,51.5362633384249));
#23119=CARTESIAN_POINT('Ctrl Pts',(-0.162329551315805,-3.92964859965489,
51.5421399919873));
#23120=CARTESIAN_POINT('Ctrl Pts',(-0.0467602864631677,-3.93442264151478,
51.5480091232964));
#23121=CARTESIAN_POINT('Ctrl Pts',(0.0691751238794702,-3.93410051996893,
51.5538782546055));
#23122=CARTESIAN_POINT('Ctrl Pts',(0.184991176837534,-3.92864700176693,
51.5597473859146));
#23123=CARTESIAN_POINT('Ctrl Pts',(0.300689823238378,-3.9231990119764,51.5656105674915));
#23124=CARTESIAN_POINT('Ctrl Pts',(0.416268943145369,-3.91262999213387,
51.5714737490684));
#23125=CARTESIAN_POINT('Ctrl Pts',(0.531241274755709,-3.89695672390597,
51.5773369306452));
#23126=CARTESIAN_POINT('Ctrl Pts',(0.649455143636631,-3.88084156255125,
51.5833654191385));
#23127=CARTESIAN_POINT('Ctrl Pts',(0.767027055499234,-3.85933002829415,
51.5893939076317));
#23128=CARTESIAN_POINT('Ctrl Pts',(0.883430671087542,-3.83249778204525,
51.595422396125));
#23129=CARTESIAN_POINT('Ctrl Pts',(0.99651456511733,-3.8064307662051,51.6012789578003));
#23130=CARTESIAN_POINT('Ctrl Pts',(1.10849547073079,-3.77534251790644,51.6071355194757));
#23131=CARTESIAN_POINT('Ctrl Pts',(1.21890014683637,-3.73935441380491,51.6129920811511));
#23132=CARTESIAN_POINT('Ctrl Pts',(1.32928876797764,-3.7033715430662,51.6188477911697));
#23133=CARTESIAN_POINT('Ctrl Pts',(1.43810122319181,-3.66249036125565,51.6247035011883));
#23134=CARTESIAN_POINT('Ctrl Pts',(1.5448797500048,-3.61688202157951,51.6305592112069));
#23135=CARTESIAN_POINT('Ctrl Pts',(1.65166849401177,-3.57126931783067,51.6364154815341));
#23136=CARTESIAN_POINT('Ctrl Pts',(1.75642254325717,-3.52092871914075,51.6422717518613));
#23137=CARTESIAN_POINT('Ctrl Pts',(1.85870507712417,-3.46607911569727,51.6481280221885));
#23138=CARTESIAN_POINT('Ctrl Pts',(1.96625256103048,-3.40840615218548,51.6542857415464));
#23139=CARTESIAN_POINT('Ctrl Pts',(2.07106686250261,-3.34574786066241,51.6604434609043));
#23140=CARTESIAN_POINT('Ctrl Pts',(2.17267192079167,-3.27841207364227,51.6666011802621));
#23141=CARTESIAN_POINT('Ctrl Pts',(2.26944686453354,-3.21427730407056,51.672466173152));
#23142=CARTESIAN_POINT('Ctrl Pts',(2.36331036165917,-3.14589982114848,51.6783311660418));
#23143=CARTESIAN_POINT('Ctrl Pts',(2.45388381829003,-3.07358800204814,51.6841961589316));
#23144=CARTESIAN_POINT('Ctrl Pts',(2.54451954056608,-3.00122647145132,51.6900651837706));
#23145=CARTESIAN_POINT('Ctrl Pts',(2.63186040877973,-2.92492548975659,51.6959342086095));
#23146=CARTESIAN_POINT('Ctrl Pts',(2.71556370249527,-2.84503124371071,51.7018032334484));
#23147=CARTESIAN_POINT('Ctrl Pts',(2.7993857529864,-2.76502364509976,51.7076805851576));
#23148=CARTESIAN_POINT('Ctrl Pts',(2.87955964664603,-2.6814129060543,51.7135579368667));
#23149=CARTESIAN_POINT('Ctrl Pts',(2.95578202819155,-2.59457927260274,51.7194352885759));
#23150=CARTESIAN_POINT('Ctrl Pts',(2.9669584194391,-2.58184696693054,51.7202970772116));
#23151=CARTESIAN_POINT('Ctrl Pts',(2.97804992849274,-2.56904542094171,51.7211588658473));
#23152=CARTESIAN_POINT('Ctrl Pts',(2.98905567748977,-2.55617588535415,51.722020654483));
#23153=CARTESIAN_POINT('Ctrl Pts',(3.06411804358784,-2.46840195992251,51.727898300256));
#23154=CARTESIAN_POINT('Ctrl Pts',(3.13543388295215,-2.37717510774856,51.733775946029));
#23155=CARTESIAN_POINT('Ctrl Pts',(3.20266945456006,-2.282848519904,51.739653591802));
#23156=CARTESIAN_POINT('Ctrl Pts',(3.26981911428937,-2.1886424601396,51.7455237272709));
#23157=CARTESIAN_POINT('Ctrl Pts',(3.33289863769181,-2.09134487460477,51.7513938627398));
#23158=CARTESIAN_POINT('Ctrl Pts',(3.39161328128917,-1.9913433531621,51.7572639982087));
#23159=CARTESIAN_POINT('Ctrl Pts',(3.45026852051612,-1.89144300796878,51.7631281945851));
#23160=CARTESIAN_POINT('Ctrl Pts',(3.5045674567879,-1.78884452228466,51.7689923909614));
#23161=CARTESIAN_POINT('Ctrl Pts',(3.55425796100606,-1.68396536384363,51.7748565873378));
#23162=CARTESIAN_POINT('Ctrl Pts',(3.60533741168598,-1.57615462846809,51.7808846994348));
#23163=CARTESIAN_POINT('Ctrl Pts',(3.65154673786758,-1.46593419950273,51.7869128115318));
#23164=CARTESIAN_POINT('Ctrl Pts',(3.69266193913359,-1.35378609952757,51.7929409236288));
#23165=CARTESIAN_POINT('Ctrl Pts',(3.73261412492424,-1.24481030497198,51.7987985200177));
#23166=CARTESIAN_POINT('Ctrl Pts',(3.76775636436242,-1.13401484549651,51.8046561164067));
#23167=CARTESIAN_POINT('Ctrl Pts',(3.79793179280356,-1.02186256278029,51.8105137127956));
#23168=CARTESIAN_POINT('Ctrl Pts',(3.82810286277188,-0.909726479094201,
51.8163704631261));
#23169=CARTESIAN_POINT('Ctrl Pts',(3.85330844116812,-0.796234360075338,
51.8222272134567));
#23170=CARTESIAN_POINT('Ctrl Pts',(3.87344181331822,-0.681863269899464,
51.8280839637872));
#23171=CARTESIAN_POINT('Ctrl Pts',(3.89357712697097,-0.567481150683174,
51.8339412788963));
#23172=CARTESIAN_POINT('Ctrl Pts',(3.90863919053139,-0.452220298051512,
51.8397985940054));
#23173=CARTESIAN_POINT('Ctrl Pts',(3.91857271447358,-0.336566310529017,
51.8456559091144));
#23174=CARTESIAN_POINT('Ctrl Pts',(3.92901325945277,-0.215009180775335,
51.851812189827));
#23175=CARTESIAN_POINT('Ctrl Pts',(3.9337878535178,-0.0930182296759476,
51.8579684705397));
#23176=CARTESIAN_POINT('Ctrl Pts',(3.93289425801458,0.0288401677507168,
51.8641247512523));
#23177=CARTESIAN_POINT('Ctrl Pts',(3.93204279158699,0.144953480713162,51.8699907905582));
#23178=CARTESIAN_POINT('Ctrl Pts',(3.9260454836577,0.260946036023648,51.8758568298642));
#23179=CARTESIAN_POINT('Ctrl Pts',(3.91495378487565,0.376332117002756,51.8817228691702));
#23180=CARTESIAN_POINT('Ctrl Pts',(3.90385446151273,0.491797515904352,51.8875929408694));
#23181=CARTESIAN_POINT('Ctrl Pts',(3.88765383153072,0.606655203033215,51.8934630125686));
#23182=CARTESIAN_POINT('Ctrl Pts',(3.86645461305077,0.720428848130284,51.8993330842678));
#23183=CARTESIAN_POINT('Ctrl Pts',(3.84522534329854,0.834363774776051,51.9052114771758));
#23184=CARTESIAN_POINT('Ctrl Pts',(3.81898343906944,0.947211193118578,51.9110898700838));
#23185=CARTESIAN_POINT('Ctrl Pts',(3.78788165308817,1.05850913184438,51.9169682629918));
#23186=CARTESIAN_POINT('Ctrl Pts',(3.78336146448637,1.07468465547299,51.9178226012165));
#23187=CARTESIAN_POINT('Ctrl Pts',(3.77873870681719,1.09082748452661,51.9186769394411));
#23188=CARTESIAN_POINT('Ctrl Pts',(3.77401393306265,1.10693623711978,51.9195312776658));
#23189=CARTESIAN_POINT('Ctrl Pts',(3.74150913385129,1.21775884911978,51.9254088273422));
#23190=CARTESIAN_POINT('Ctrl Pts',(3.70406554225549,1.32733009494124,51.9312863770185));
#23191=CARTESIAN_POINT('Ctrl Pts',(3.66179663040747,1.43517749339113,51.9371639266948));
#23192=CARTESIAN_POINT('Ctrl Pts',(3.61958172310896,1.54288710144343,51.9430339669651));
#23193=CARTESIAN_POINT('Ctrl Pts',(3.57255390550052,1.64887686165038,51.9489040072354));
#23194=CARTESIAN_POINT('Ctrl Pts',(3.5208767670674,1.75268816140378,51.9547740475057));
#23195=CARTESIAN_POINT('Ctrl Pts',(3.46925190475028,1.85639444660502,51.9606381496975));
#23196=CARTESIAN_POINT('Ctrl Pts',(3.41298725985111,1.95792628777203,51.9665022518893));
#23197=CARTESIAN_POINT('Ctrl Pts',(3.35229472869644,2.05684444038775,51.972366354081));
#23198=CARTESIAN_POINT('Ctrl Pts',(3.28990435160217,2.15852978330803,51.978394501863));
#23199=CARTESIAN_POINT('Ctrl Pts',(3.22283485144771,2.25745262942961,51.984422649645));
#23200=CARTESIAN_POINT('Ctrl Pts',(3.15136757940517,2.35316199601174,51.990450797427));
#23201=CARTESIAN_POINT('Ctrl Pts',(3.08192337454572,2.44616205981633,51.9963083027932));
#23202=CARTESIAN_POINT('Ctrl Pts',(3.00832730189277,2.53612778339065,52.0021658081594));
#23203=CARTESIAN_POINT('Ctrl Pts',(2.93088130962389,2.62267492245938,52.0080233135255));
#23204=CARTESIAN_POINT('Ctrl Pts',(2.85344648590253,2.70920958049703,52.0138799741763));
#23205=CARTESIAN_POINT('Ctrl Pts',(2.77216312158727,2.79232632706189,52.019736634827));
#23206=CARTESIAN_POINT('Ctrl Pts',(2.68737247604201,2.87167515137276,52.0255932954777));
#23207=CARTESIAN_POINT('Ctrl Pts',(2.6025736328453,2.95103164721391,52.0314505223567));
#23208=CARTESIAN_POINT('Ctrl Pts',(2.51426713552821,3.02661921477329,52.0373077492357));
#23209=CARTESIAN_POINT('Ctrl Pts',(2.42282948697284,3.0981262526009,52.0431649761148));
#23210=CARTESIAN_POINT('Ctrl Pts',(2.326721260052,3.17328582556181,52.0493213865093));
#23211=CARTESIAN_POINT('Ctrl Pts',(2.22715395030478,3.24393667225648,52.0554777969038));
#23212=CARTESIAN_POINT('Ctrl Pts',(2.12460074935781,3.30976746250068,52.0616342072983));
#23213=CARTESIAN_POINT('Ctrl Pts',(2.02688593127163,3.37249240559151,52.0675001628824));
#23214=CARTESIAN_POINT('Ctrl Pts',(1.92646092773579,3.43084156162493,52.0733661184665));
#23215=CARTESIAN_POINT('Ctrl Pts',(1.8237606571654,3.48459266850167,52.0792320740506));
#23216=CARTESIAN_POINT('Ctrl Pts',(1.72098976059647,3.53838073950298,52.0851020635965));
#23217=CARTESIAN_POINT('Ctrl Pts',(1.61594085388379,3.58756429057839,52.0909720531424));
#23218=CARTESIAN_POINT('Ctrl Pts',(1.50906900213238,3.631969128008,52.0968420426884));
#23219=CARTESIAN_POINT('Ctrl Pts',(1.40204560072971,3.67643693372641,52.1027203561742));
#23220=CARTESIAN_POINT('Ctrl Pts',(1.29319448196287,3.71611236350754,52.10859866966));
#23221=CARTESIAN_POINT('Ctrl Pts',(1.18298601924968,3.75087097595475,52.1144769831458));
#23222=CARTESIAN_POINT('Ctrl Pts',(1.16695672571622,3.75592644980872,52.1153319557134));
#23223=CARTESIAN_POINT('Ctrl Pts',(1.15089873538002,3.76087800014745,52.1161869282811));
#23224=CARTESIAN_POINT('Ctrl Pts',(1.13481351104836,3.76572533453279,52.1170419008488));
#23225=CARTESIAN_POINT('Ctrl Pts',(1.02423857216309,3.79904745005716,52.1229192537206));
#23226=CARTESIAN_POINT('Ctrl Pts',(0.912013391930761,3.82754978012318,52.1287966065924));
#23227=CARTESIAN_POINT('Ctrl Pts',(0.798595653982026,3.8510691997731,52.1346739594642));
#23228=CARTESIAN_POINT('Ctrl Pts',(0.685322895731775,3.87455855500425,52.1405437994297));
#23229=CARTESIAN_POINT('Ctrl Pts',(0.570861011804716,3.89307758428636,52.1464136393951));
#23230=CARTESIAN_POINT('Ctrl Pts',(0.455683456048091,3.90651271441474,52.1522834793605));
#23231=CARTESIAN_POINT('Ctrl Pts',(0.340622480277015,3.91993424582361,52.1581473780134));
#23232=CARTESIAN_POINT('Ctrl Pts',(0.22484768097639,3.92828206641365,52.1640112766663));
#23233=CARTESIAN_POINT('Ctrl Pts',(0.108842686602906,3.93149364358803,52.1698751753191));
#23234=CARTESIAN_POINT('Ctrl Pts',(-0.010413119253216,3.93479521888716,
52.1759033981821));
#23235=CARTESIAN_POINT('Ctrl Pts',(-0.129911778455284,3.93266833168623,
52.1819316210452));
#23236=CARTESIAN_POINT('Ctrl Pts',(-0.249121807255898,3.92510220569472,
52.1879598439082));
#23237=CARTESIAN_POINT('Ctrl Pts',(-0.364951684713297,3.91775061409424,
52.1938171389909));
#23238=CARTESIAN_POINT('Ctrl Pts',(-0.48050864107356,3.905264121684,52.1996744340737));
#23239=CARTESIAN_POINT('Ctrl Pts',(-0.595305907292519,3.88768567103137,
52.2055317291565));
#23240=CARTESIAN_POINT('Ctrl Pts',(-0.710086575880422,3.87010976190824,
52.2113881773791));
#23241=CARTESIAN_POINT('Ctrl Pts',(-0.824107365082178,3.84744342093164,
52.2172446256018));
#23242=CARTESIAN_POINT('Ctrl Pts',(-0.936888698124418,3.81978121982487,
52.2231010738245));
#23243=CARTESIAN_POINT('Ctrl Pts',(-1.04968089843017,3.79211635327319,52.2289580863565));
#23244=CARTESIAN_POINT('Ctrl Pts',(-1.1612330045025,3.7594547679124,52.2348150988886));
#23245=CARTESIAN_POINT('Ctrl Pts',(-1.27107835219798,3.72194153938152,52.2406721114207));
#23246=CARTESIAN_POINT('Ctrl Pts',(-1.38654420853534,3.68250885381795,52.2468288124716));
#23247=CARTESIAN_POINT('Ctrl Pts',(-1.50012353867866,3.63771504765641,52.2529855135225));
#23248=CARTESIAN_POINT('Ctrl Pts',(-1.61129695160193,3.58778638351817,52.2591422145734));
#23249=CARTESIAN_POINT('Ctrl Pts',(-1.71721636315969,3.54021732373732,52.2650079529303));
#23250=CARTESIAN_POINT('Ctrl Pts',(-1.82095171208986,3.4879878901259,52.2708736912872));
#23251=CARTESIAN_POINT('Ctrl Pts',(-1.9220792453382,3.43134090038285,52.276739429644));
#23252=CARTESIAN_POINT('Ctrl Pts',(-2.02327630887592,3.37465496297181,52.2826092009924));
#23253=CARTESIAN_POINT('Ctrl Pts',(-2.12186163679519,3.3135456382147,52.2884789723409));
#23254=CARTESIAN_POINT('Ctrl Pts',(-2.21744072864956,3.24829888017192,52.2943487436893));
#23255=CARTESIAN_POINT('Ctrl Pts',(-2.31315536032801,3.18295959630644,52.300226838906));
#23256=CARTESIAN_POINT('Ctrl Pts',(-2.40585492077329,3.11347141802519,52.3061049341228));
#23257=CARTESIAN_POINT('Ctrl Pts',(-2.49517821624012,3.04016030320784,52.3119830293395));
#23258=CARTESIAN_POINT('Ctrl Pts',(-2.50819352846376,3.02947812848709,52.3128395275702));
#23259=CARTESIAN_POINT('Ctrl Pts',(-2.52113722270169,3.01871484990376,52.3136960258009));
#23260=CARTESIAN_POINT('Ctrl Pts',(-2.53400824918214,3.00787153865935,52.3145525240316));
#23261=CARTESIAN_POINT('Ctrl Pts',(-2.62112209425453,2.93448170162867,52.3203494862463));
#23262=CARTESIAN_POINT('Ctrl Pts',(-2.70520695291592,2.85716757218173,52.3261464484611));
#23263=CARTESIAN_POINT('Ctrl Pts',(-2.78588153773734,2.77621199797391,52.3319434106759));
#23264=CARTESIAN_POINT('Ctrl Pts',(-2.86645237806399,2.69536052960268,52.3377329182144));
#23265=CARTESIAN_POINT('Ctrl Pts',(-2.94362136416235,2.61087722211626,52.3435224257529));
#23266=CARTESIAN_POINT('Ctrl Pts',(-3.0170396055435,2.52308561459615,52.3493119332913));
#23267=CARTESIAN_POINT('Ctrl Pts',(-3.09037685056803,2.435390860395,52.3550950537384));
#23268=CARTESIAN_POINT('Ctrl Pts',(-3.15997131095199,2.34439539023446,52.3608781741855));
#23269=CARTESIAN_POINT('Ctrl Pts',(-3.22551105566922,2.25045938193865,52.3666612946326));
#23270=CARTESIAN_POINT('Ctrl Pts',(-3.29101068199178,2.15658087404768,52.3724408750978));
#23271=CARTESIAN_POINT('Ctrl Pts',(-3.35246028148819,2.05976575145766,52.378220455563));
#23272=CARTESIAN_POINT('Ctrl Pts',(-3.40958866854164,1.96040661888102,52.3840000360282));
#23273=CARTESIAN_POINT('Ctrl Pts',(-3.46669676108072,1.86108278303597,52.3897775633324));
#23274=CARTESIAN_POINT('Ctrl Pts',(-3.51948648055126,1.75921710129378,52.3955550906365));
#23275=CARTESIAN_POINT('Ctrl Pts',(-3.56773087095463,1.65522972195325,52.4013326179407));
#23276=CARTESIAN_POINT('Ctrl Pts',(-3.61597051469422,1.55125257371154,52.4071095768062));
#23277=CARTESIAN_POINT('Ctrl Pts',(-3.65966554066308,1.44515452875821,52.4128865356716));
#23278=CARTESIAN_POINT('Ctrl Pts',(-3.69863610549226,1.33737801654922,52.4186634945371));
#23279=CARTESIAN_POINT('Ctrl Pts',(-3.73763365884993,1.22952686519958,52.4244444541559));
#23280=CARTESIAN_POINT('Ctrl Pts',(-3.77190006757119,1.11999532388408,52.4302254137747));
#23281=CARTESIAN_POINT('Ctrl Pts',(-3.80130464568568,1.0092432762662,52.4360063733935));
#23282=CARTESIAN_POINT('Ctrl Pts',(-3.83071867342992,0.898455636712971,
52.4417891908159));
#23283=CARTESIAN_POINT('Ctrl Pts',(-3.85526766537381,0.786447124592048,
52.4475720082382));
#23284=CARTESIAN_POINT('Ctrl Pts',(-3.87487198407122,0.673688434708522,
52.4533548256605));
#23285=CARTESIAN_POINT('Ctrl Pts',(-3.89450369890896,0.56077216970399,52.4591457243062));
#23286=CARTESIAN_POINT('Ctrl Pts',(-3.90917687778931,0.447104054202614,
52.4649366229518));
#23287=CARTESIAN_POINT('Ctrl Pts',(-3.91886372212132,0.333160813184191,
52.4707275215975));
#23288=CARTESIAN_POINT('Ctrl Pts',(-3.92836763751898,0.221369306511939,
52.4764090633791));
#23289=CARTESIAN_POINT('Ctrl Pts',(-3.9330719559648,0.109313357446281,52.4820906051608));
#23290=CARTESIAN_POINT('Ctrl Pts',(-3.93299916752078,-0.00255896091143951,
52.4877721469424));
#23291=CARTESIAN_POINT('',(-3.93299851282984,0.00342024536944883,53.7377721470129));
#23292=CARTESIAN_POINT('Ctrl Pts',(-3.93299916752023,-0.00255896175136066,
52.4877721469851));
#23293=CARTESIAN_POINT('Ctrl Pts',(-3.93289543366542,-0.161992827610475,
52.4958691470615));
#23294=CARTESIAN_POINT('Ctrl Pts',(-3.9230971514168,-0.321109276650609,
52.503966147138));
#23295=CARTESIAN_POINT('Ctrl Pts',(-3.90371904854297,-0.479026711199759,
52.5120631472145));
#23296=CARTESIAN_POINT('Ctrl Pts',(-3.88965284348736,-0.593656044663781,
52.5179406092216));
#23297=CARTESIAN_POINT('Ctrl Pts',(-3.8705103217993,-0.707853182698984,
52.5238180712288));
#23298=CARTESIAN_POINT('Ctrl Pts',(-3.84632666030604,-0.821133498414874,
52.5296955332359));
#23299=CARTESIAN_POINT('Ctrl Pts',(-3.82217390497882,-0.934269044479273,
52.535565483981));
#23300=CARTESIAN_POINT('Ctrl Pts',(-3.79299290768883,-1.04648969857835,
52.5414354347262));
#23301=CARTESIAN_POINT('Ctrl Pts',(-3.75887055019978,-1.15731637283887,
52.5473053854714));
#23302=CARTESIAN_POINT('Ctrl Pts',(-3.72478272118824,-1.26803090137994,
52.5531693964024));
#23303=CARTESIAN_POINT('Ctrl Pts',(-3.68576359884078,-1.37735386398089,
52.5590334073333));
#23304=CARTESIAN_POINT('Ctrl Pts',(-3.64195087718146,-1.48481743261495,
52.5648974182643));
#23305=CARTESIAN_POINT('Ctrl Pts',(-3.59691156292701,-1.59528957986593,
52.5709255996032));
#23306=CARTESIAN_POINT('Ctrl Pts',(-3.54680636522229,-1.70379624693751,
52.5769537809421));
#23307=CARTESIAN_POINT('Ctrl Pts',(-3.49183961551256,-1.80984670608788,
52.582981962281));
#23308=CARTESIAN_POINT('Ctrl Pts',(-3.43843000629795,-1.9128928860087,52.5888393726479));
#23309=CARTESIAN_POINT('Ctrl Pts',(-3.38043079343676,-2.01361976233204,
52.5946967830148));
#23310=CARTESIAN_POINT('Ctrl Pts',(-3.31807746483069,-2.11159914221019,
52.6005541933816));
#23311=CARTESIAN_POINT('Ctrl Pts',(-3.25573314145588,-2.20956437164931,
52.606410757806));
#23312=CARTESIAN_POINT('Ctrl Pts',(-3.18903617419951,-2.30478254577666,
52.6122673222303));
#23313=CARTESIAN_POINT('Ctrl Pts',(-3.11826640271812,-2.39685286191695,
52.6181238866546));
#23314=CARTESIAN_POINT('Ctrl Pts',(-3.04748980263395,-2.48893206195786,
52.6239810161811));
#23315=CARTESIAN_POINT('Ctrl Pts',(-2.9726398684988,-2.57786247314646,52.6298381457076));
#23316=CARTESIAN_POINT('Ctrl Pts',(-2.89403745660768,-2.66327546448951,
52.6356952752341));
#23317=CARTESIAN_POINT('Ctrl Pts',(-2.81141695282054,-2.75305469905683,
52.6418518164977));
#23318=CARTESIAN_POINT('Ctrl Pts',(-2.72465051699632,-2.83894700917189,
52.6480083577613));
#23319=CARTESIAN_POINT('Ctrl Pts',(-2.63415450019974,-2.92056827844814,
52.6541648990249));
#23320=CARTESIAN_POINT('Ctrl Pts',(-2.54793131003757,-2.99833574790375,
52.6600307553012));
#23321=CARTESIAN_POINT('Ctrl Pts',(-2.45832304356354,-3.07222605884105,
52.6658966115776));
#23322=CARTESIAN_POINT('Ctrl Pts',(-2.36572271466626,-3.14194924168297,
52.6717624678539));
#23323=CARTESIAN_POINT('Ctrl Pts',(-2.27305871481266,-3.21172036540999,
52.6776323574278));
#23324=CARTESIAN_POINT('Ctrl Pts',(-2.17739889520996,-3.27731842298028,
52.6835022470017));
#23325=CARTESIAN_POINT('Ctrl Pts',(-2.07916395915626,-3.33849760085966,
52.6893721365756));
#23326=CARTESIAN_POINT('Ctrl Pts',(-1.98078972445159,-3.3997635317547,52.6952503497433));
#23327=CARTESIAN_POINT('Ctrl Pts',(-1.87983344487127,-3.4565978783223,52.7011285629109));
#23328=CARTESIAN_POINT('Ctrl Pts',(-1.7767390125329,-3.50880143087973,52.7070067760786));
#23329=CARTESIAN_POINT('Ctrl Pts',(-1.76173202460721,-3.5164004647474,52.7078624408515));
#23330=CARTESIAN_POINT('Ctrl Pts',(-1.74667976177442,-3.52390145991034,
52.7087181056243));
#23331=CARTESIAN_POINT('Ctrl Pts',(-1.7315836233202,-3.53130388885598,52.7095737703972));
#23332=CARTESIAN_POINT('Ctrl Pts',(-1.62789036507499,-3.58215013530697,
52.7154512117399));
#23333=CARTESIAN_POINT('Ctrl Pts',(-1.5217856557316,-3.62850859087834,52.7213286530825));
#23334=CARTESIAN_POINT('Ctrl Pts',(-1.4136946120197,-3.67014394049423,52.7272060944252));
#23335=CARTESIAN_POINT('Ctrl Pts',(-1.30574171402068,-3.71172607806908,
52.7330760241064));
#23336=CARTESIAN_POINT('Ctrl Pts',(-1.19580791189216,-3.74859696758625,
52.7389459537876));
#23337=CARTESIAN_POINT('Ctrl Pts',(-1.0843419325385,-3.78056762581212,52.7448158834688));
#23338=CARTESIAN_POINT('Ctrl Pts',(-0.972988753274336,-3.81250593073046,
52.7506798729645));
#23339=CARTESIAN_POINT('Ctrl Pts',(-0.860106875249662,-3.83955375533025,
52.7565438624603));
#23340=CARTESIAN_POINT('Ctrl Pts',(-0.746163356290465,-3.86157082619617,
52.762407851956));
#23341=CARTESIAN_POINT('Ctrl Pts',(-0.629029262716038,-3.8842044052062,
52.7684360411904));
#23342=CARTESIAN_POINT('Ctrl Pts',(-0.510773607508695,-3.90152116614789,
52.7744642304247));
#23343=CARTESIAN_POINT('Ctrl Pts',(-0.391919043644409,-3.91342413536137,
52.780492419659));
#23344=CARTESIAN_POINT('Ctrl Pts',(-0.27643207297672,-3.92498984905145,
52.7863498078034));
#23345=CARTESIAN_POINT('Ctrl Pts',(-0.160380114023787,-3.93144439402871,
52.7922071959478));
#23346=CARTESIAN_POINT('Ctrl Pts',(-0.0442504582975385,-3.93275105961977,
52.7980645840922));
#23347=CARTESIAN_POINT('Ctrl Pts',(0.0718624205706841,-3.93405753644128,
52.8039211260396));
#23348=CARTESIAN_POINT('Ctrl Pts',(0.188052561520881,-3.93021760809878,
52.8097776679869));
#23349=CARTESIAN_POINT('Ctrl Pts',(0.303831382016254,-3.92124667565075,
52.8156342099343));
#23350=CARTESIAN_POINT('Ctrl Pts',(0.419621369536783,-3.91227487794405,
52.8214913167531));
#23351=CARTESIAN_POINT('Ctrl Pts',(0.534999546451255,-3.89817112419895,
52.827348423572));
#23352=CARTESIAN_POINT('Ctrl Pts',(0.649481866172758,-3.87900274626259,
52.8332055303908));
#23353=CARTESIAN_POINT('Ctrl Pts',(0.769817495718348,-3.85885431782447,
52.8393621023232));
#23354=CARTESIAN_POINT('Ctrl Pts',(0.889162734770879,-3.83310975009962,
52.8455186742557));
#23355=CARTESIAN_POINT('Ctrl Pts',(1.00696837892769,-3.80190790049414,52.8516752461882));
#23356=CARTESIAN_POINT('Ctrl Pts',(1.11921075431069,-3.77217953101635,52.857541079382));
#23357=CARTESIAN_POINT('Ctrl Pts',(1.23005523955511,-3.737497713706,52.8634069125758));
#23358=CARTESIAN_POINT('Ctrl Pts',(1.33904424806304,-3.69803319370301,52.8692727457696));
#23359=CARTESIAN_POINT('Ctrl Pts',(1.44810819413825,-3.65854153908191,52.8751426121341));
#23360=CARTESIAN_POINT('Ctrl Pts',(1.55531374291774,-3.61426079075785,52.8810124784986));
#23361=CARTESIAN_POINT('Ctrl Pts',(1.66022516286428,-3.56540901000043,52.886882344863));
#23362=CARTESIAN_POINT('Ctrl Pts',(1.76528534866728,-3.51648795673666,52.8927605347799));
#23363=CARTESIAN_POINT('Ctrl Pts',(1.86804455018492,-3.46298312700869,52.8986387246967));
#23364=CARTESIAN_POINT('Ctrl Pts',(1.96809340004735,-3.40515746606379,52.9045169146135));
#23365=CARTESIAN_POINT('Ctrl Pts',(1.98265986360733,-3.39673842492396,52.9053727409357));
#23366=CARTESIAN_POINT('Ctrl Pts',(1.99716892846468,-3.38822786534177,52.906228567258));
#23367=CARTESIAN_POINT('Ctrl Pts',(2.0116193876095,-3.37962667160051,52.9070843935802));
#23368=CARTESIAN_POINT('Ctrl Pts',(2.11085911684612,-3.32055725868841,52.9129618519808));
#23369=CARTESIAN_POINT('Ctrl Pts',(2.20765753343926,-3.257016191809,52.9188393103813));
#23370=CARTESIAN_POINT('Ctrl Pts',(2.30158528416095,-3.18923096995714,52.9247167687819));
#23371=CARTESIAN_POINT('Ctrl Pts',(2.39539299459476,-3.12153237806801,52.9305867157516));
#23372=CARTESIAN_POINT('Ctrl Pts',(2.48633700384373,-3.04960065758682,52.9364566627214));
#23373=CARTESIAN_POINT('Ctrl Pts',(2.57401386514186,-2.97370839559924,52.9423266096912));
#23374=CARTESIAN_POINT('Ctrl Pts',(2.6616020035624,-2.89789293129545,52.9481906166834));
#23375=CARTESIAN_POINT('Ctrl Pts',(2.7459292603824,-2.81812516606789,52.9540546236756));
#23376=CARTESIAN_POINT('Ctrl Pts',(2.82662297125485,-2.73471965261055,52.9599186306678));
#23377=CARTESIAN_POINT('Ctrl Pts',(2.90957587988532,-2.64897901852271,52.9659468134218));
#23378=CARTESIAN_POINT('Ctrl Pts',(2.98868841453171,-2.55939418855801,52.9719749961758));
#23379=CARTESIAN_POINT('Ctrl Pts',(3.06359380707849,-2.46634993162573,52.9780031789297));
#23380=CARTESIAN_POINT('Ctrl Pts',(3.13637715108831,-2.37594159211652,52.9838605849751));
#23381=CARTESIAN_POINT('Ctrl Pts',(3.2051882516026,-2.28226754593297,52.9897179910205));
#23382=CARTESIAN_POINT('Ctrl Pts',(3.26973012950807,-2.18571587361831,52.9955753970659));
#23383=CARTESIAN_POINT('Ctrl Pts',(3.33426268460913,-2.08917814778903,53.0014319570335));
#23384=CARTESIAN_POINT('Ctrl Pts',(3.39452701418716,-1.9897639652298,53.0072885170011));
#23385=CARTESIAN_POINT('Ctrl Pts',(3.45026908043435,-1.88789095887411,53.0131450769686));
#23386=CARTESIAN_POINT('Ctrl Pts',(3.50601652401266,-1.78600812502327,53.0190022019074));
#23387=CARTESIAN_POINT('Ctrl Pts',(3.55724063901352,-1.68166635773221,53.0248593268462));
#23388=CARTESIAN_POINT('Ctrl Pts',(3.60373336091434,-1.57530786306453,53.030716451785));
#23389=CARTESIAN_POINT('Ctrl Pts',(3.65260283771765,-1.46351221472446,53.0368729988665));
#23390=CARTESIAN_POINT('Ctrl Pts',(3.69624417043921,-1.349488654406,53.043029545948));
#23391=CARTESIAN_POINT('Ctrl Pts',(3.73447360609827,-1.23377302829787,53.0491860930295));
#23392=CARTESIAN_POINT('Ctrl Pts',(3.77089795007778,-1.12352118448947,53.0550519444279));
#23393=CARTESIAN_POINT('Ctrl Pts',(3.80240973273049,-1.01173383485323,53.0609177958264));
#23394=CARTESIAN_POINT('Ctrl Pts',(3.8289019601574,-0.898887523276836,53.0667836472248));
#23395=CARTESIAN_POINT('Ctrl Pts',(3.85541240290985,-0.785963621686248,
53.072653531821));
#23396=CARTESIAN_POINT('Ctrl Pts',(3.87689634188851,-0.671979712553978,
53.0785234164173));
#23397=CARTESIAN_POINT('Ctrl Pts',(3.89329835365933,-0.557419886076462,
53.0843933010135));
#23398=CARTESIAN_POINT('Ctrl Pts',(3.90972362344108,-0.442697614056647,
53.0902715090911));
#23399=CARTESIAN_POINT('Ctrl Pts',(3.92105254676972,-0.327398203845943,
53.0961497171688));
#23400=CARTESIAN_POINT('Ctrl Pts',(3.92728169715956,-0.212008186529219,
53.1020279252464));
#23401=CARTESIAN_POINT('Ctrl Pts',(3.92818848138756,-0.195210735637382,
53.1028836224186));
#23402=CARTESIAN_POINT('Ctrl Pts',(3.92898728655392,-0.178411359029593,
53.1037393195908));
#23403=CARTESIAN_POINT('Ctrl Pts',(3.92967819380633,-0.16161155009135,53.104595016763));
#23404=CARTESIAN_POINT('Ctrl Pts',(3.93442376957651,-0.0462201340038854,
53.1104724710128));
#23405=CARTESIAN_POINT('Ctrl Pts',(3.93409027677237,0.0695696312581488,
53.1163499252626));
#23406=CARTESIAN_POINT('Ctrl Pts',(3.92863368139037,0.185273844471055,53.1222273795125));
#23407=CARTESIAN_POINT('Ctrl Pts',(3.92318405960244,0.30083018631742,53.1280973223056));
#23408=CARTESIAN_POINT('Ctrl Pts',(3.91262437565026,0.416300785173605,53.1339672650987));
#23409=CARTESIAN_POINT('Ctrl Pts',(3.89696251336728,0.531198804036748,53.1398372078918));
#23410=CARTESIAN_POINT('Ctrl Pts',(3.88131649986442,0.645980553620793,53.1457012106867));
#23411=CARTESIAN_POINT('Ctrl Pts',(3.86057863363714,0.760190469397612,53.1515652134817));
#23412=CARTESIAN_POINT('Ctrl Pts',(3.83480876508224,0.873344568454129,53.1574292162767));
#23413=CARTESIAN_POINT('Ctrl Pts',(3.80831738658687,0.989666778636287,53.1634574005962));
#23414=CARTESIAN_POINT('Ctrl Pts',(3.77650808360688,1.10487273239808,53.1694855849158));
#23415=CARTESIAN_POINT('Ctrl Pts',(3.73950273839359,1.21844502114242,53.1755137692353));
#23416=CARTESIAN_POINT('Ctrl Pts',(3.70354577936992,1.3287997309571,53.1813711710597));
#23417=CARTESIAN_POINT('Ctrl Pts',(3.66268337654109,1.43761168075823,53.1872285728841));
#23418=CARTESIAN_POINT('Ctrl Pts',(3.61707831474994,1.54442010637185,53.1930859747086));
#23419=CARTESIAN_POINT('Ctrl Pts',(3.57147984043455,1.65121310391924,53.1989425304538));
#23420=CARTESIAN_POINT('Ctrl Pts',(3.52114023135627,1.7560027734931,53.204799086199));
#23421=CARTESIAN_POINT('Ctrl Pts',(3.46627048514959,1.85834817076369,53.2106556419443));
#23422=CARTESIAN_POINT('Ctrl Pts',(3.41139544572767,1.96070344116572,53.2165127626641));
#23423=CARTESIAN_POINT('Ctrl Pts',(3.3519895953428,2.06061360696042,53.2223698833839));
#23424=CARTESIAN_POINT('Ctrl Pts',(3.28830963052443,2.15766280354466,53.2282270041037));
#23425=CARTESIAN_POINT('Ctrl Pts',(3.22137416916708,2.25967342440876,53.2343835570905));
#23426=CARTESIAN_POINT('Ctrl Pts',(3.14971629912284,2.35852238921075,53.2405401100774));
#23427=CARTESIAN_POINT('Ctrl Pts',(3.07368443022098,2.45376303326484,53.2466966630642));
#23428=CARTESIAN_POINT('Ctrl Pts',(3.00124270376511,2.54450651732878,53.2525625102915));
#23429=CARTESIAN_POINT('Ctrl Pts',(2.92483093237803,2.63197437799811,53.2584283575188));
#23430=CARTESIAN_POINT('Ctrl Pts',(2.84478979244263,2.71581664270881,53.2642942047462));
#23431=CARTESIAN_POINT('Ctrl Pts',(2.76469361815354,2.79971655533474,53.2701640851883));
#23432=CARTESIAN_POINT('Ctrl Pts',(2.68096340321106,2.87998562344194,53.2760339656304));
#23433=CARTESIAN_POINT('Ctrl Pts',(2.59397431994681,2.95631294477707,53.2819038460725));
#23434=CARTESIAN_POINT('Ctrl Pts',(2.50686188556649,3.03274849877679,53.2877820500453));
#23435=CARTESIAN_POINT('Ctrl Pts',(2.41648168233906,3.10523089601225,53.2936602540181));
#23436=CARTESIAN_POINT('Ctrl Pts',(2.32323933546826,3.17349145108868,53.2995384579909));
#23437=CARTESIAN_POINT('Ctrl Pts',(2.30966545749243,3.18342857168104,53.3003941853092));
#23438=CARTESIAN_POINT('Ctrl Pts',(2.29603096802954,3.19327629945579,53.3012499126276));
#23439=CARTESIAN_POINT('Ctrl Pts',(2.282337162349,3.20303388638969,53.3021056399459));
#23440=CARTESIAN_POINT('Ctrl Pts',(2.18828303191081,3.2700526082595,53.3079830921821));
#23441=CARTESIAN_POINT('Ctrl Pts',(2.09112031510791,3.3330349618521,53.3138605444183));
#23442=CARTESIAN_POINT('Ctrl Pts',(1.99123024842126,3.39167968678827,53.3197379966545));
#23443=CARTESIAN_POINT('Ctrl Pts',(1.89146784322042,3.45024946260318,53.3256079373901));
#23444=CARTESIAN_POINT('Ctrl Pts',(1.78898537272642,3.50449242759051,53.3314778781258));
#23445=CARTESIAN_POINT('Ctrl Pts',(1.68419489763579,3.55414920153579,53.3373478188615));
#23446=CARTESIAN_POINT('Ctrl Pts',(1.5795104644201,3.60375572570973,53.3432118195581));
#23447=CARTESIAN_POINT('Ctrl Pts',(1.47252304305926,3.64878511486443,53.3490758202546));
#23448=CARTESIAN_POINT('Ctrl Pts',(1.36367069574011,3.68902307306144,53.3549398209512));
#23449=CARTESIAN_POINT('Ctrl Pts',(1.25177062424374,3.73038764176396,53.3609680060419));
#23450=CARTESIAN_POINT('Ctrl Pts',(1.13790003310018,3.76668827743619,53.3669961911327));
#23451=CARTESIAN_POINT('Ctrl Pts',(1.02255887224883,3.79774437696709,53.3730243762234));
#23452=CARTESIAN_POINT('Ctrl Pts',(0.910485459841775,3.82792062129125,53.3788817758607));
#23453=CARTESIAN_POINT('Ctrl Pts',(0.797024109427844,3.85314539323487,53.3847391754981));
#23454=CARTESIAN_POINT('Ctrl Pts',(0.682649674448849,3.87330329589291,53.3905965751354));
#23455=CARTESIAN_POINT('Ctrl Pts',(0.56829176099391,3.89345828671778,53.3964531286643));
#23456=CARTESIAN_POINT('Ctrl Pts',(0.453021431388943,3.9085477921124,53.4023096821933));
#23457=CARTESIAN_POINT('Ctrl Pts',(0.33732327989459,3.91850762470116,53.4081662357222));
#23458=CARTESIAN_POINT('Ctrl Pts',(0.221613967672717,3.92846841805703,53.4140233541988));
#23459=CARTESIAN_POINT('Ctrl Pts',(0.10547716251848,3.93329851955016,53.4198804726754));
#23460=CARTESIAN_POINT('Ctrl Pts',(-0.0105985794115888,3.93298571954113,
53.425737591152));
#23461=CARTESIAN_POINT('Ctrl Pts',(-0.132608541830317,3.93265692804075,
53.43189414715));
#23462=CARTESIAN_POINT('Ctrl Pts',(-0.254550524003057,3.92664547323169,
53.4380507031481));
#23463=CARTESIAN_POINT('Ctrl Pts',(-0.375860063953985,3.91499913311925,
53.4442072591462));
#23464=CARTESIAN_POINT('Ctrl Pts',(-0.491441397236081,3.90390273032524,
53.4500731040828));
#23465=CARTESIAN_POINT('Ctrl Pts',(-0.606448242278903,3.88769155541726,
53.4559389490194));
#23466=CARTESIAN_POINT('Ctrl Pts',(-0.720401348885594,3.86645973682952,
53.461804793956));
#23467=CARTESIAN_POINT('Ctrl Pts',(-0.834432806611564,3.84521331980915,
53.4676746720912));
#23468=CARTESIAN_POINT('Ctrl Pts',(-0.947408682541798,3.81893947843412,
53.4735445502265));
#23469=CARTESIAN_POINT('Ctrl Pts',(-1.05886360324246,3.78778257952175,53.4794144283617));
#23470=CARTESIAN_POINT('Ctrl Pts',(-1.17047656767251,3.7565814999445,53.4852926300185));
#23471=CARTESIAN_POINT('Ctrl Pts',(-1.28056388315803,3.72048367430413,53.4911708316753));
#23472=CARTESIAN_POINT('Ctrl Pts',(-1.38867889737911,3.67968204060812,53.4970490333321));
#23473=CARTESIAN_POINT('Ctrl Pts',(-1.40441818308723,3.67374217578244,53.4979047765977));
#23474=CARTESIAN_POINT('Ctrl Pts',(-1.42011571071211,3.66770270190615,53.4987605198632));
#23475=CARTESIAN_POINT('Ctrl Pts',(-1.43577014599622,3.66156429519762,53.4996162631288));
#23476=CARTESIAN_POINT('Ctrl Pts',(-1.5432886424542,3.61940421417453,53.5054937175114));
#23477=CARTESIAN_POINT('Ctrl Pts',(-1.64912482168042,3.57243524253913,53.511371171894));
#23478=CARTESIAN_POINT('Ctrl Pts',(-1.75281807226117,3.52081209461037,53.5172486262766));
#23479=CARTESIAN_POINT('Ctrl Pts',(-1.85637880139806,3.4692549217963,53.5231185691892));
#23480=CARTESIAN_POINT('Ctrl Pts',(-1.95780168249082,3.41305558422226,53.5289885121017));
#23481=CARTESIAN_POINT('Ctrl Pts',(-2.05664434040339,3.35241749444886,53.5348584550143));
#23482=CARTESIAN_POINT('Ctrl Pts',(-2.15538697578883,3.29184076659254,53.5407224579154));
#23483=CARTESIAN_POINT('Ctrl Pts',(-2.25155423217577,3.22683443581695,53.5465864608165));
#23484=CARTESIAN_POINT('Ctrl Pts',(-2.34472728922019,3.15764832417832,53.5524504637176));
#23485=CARTESIAN_POINT('Ctrl Pts',(-2.44050902172943,3.08652512774648,53.5584786479924));
#23486=CARTESIAN_POINT('Ctrl Pts',(-2.53312601293964,3.0109848326888,53.5645068322671));
#23487=CARTESIAN_POINT('Ctrl Pts',(-2.62215385049671,2.93134750316733,53.5705350165419));
#23488=CARTESIAN_POINT('Ctrl Pts',(-2.70865947155471,2.85396635094919,53.5763924184383));
#23489=CARTESIAN_POINT('Ctrl Pts',(-2.79177624728224,2.77271748416481,53.5822498203347));
#23490=CARTESIAN_POINT('Ctrl Pts',(-2.87114809007967,2.68793557304335,53.5881072222311));
#23491=CARTESIAN_POINT('Ctrl Pts',(-2.95050846774535,2.6031659085291,53.5939637780354));
#23492=CARTESIAN_POINT('Ctrl Pts',(-3.02612470633072,2.51486451556273,53.5998203338398));
#23493=CARTESIAN_POINT('Ctrl Pts',(-3.09767828727034,2.42340220115729,53.6056768896442));
#23494=CARTESIAN_POINT('Ctrl Pts',(-3.16923877073477,2.33193106370083,53.6115340104101));
#23495=CARTESIAN_POINT('Ctrl Pts',(-3.23673556329017,2.2372987235491,53.617391131176));
#23496=CARTESIAN_POINT('Ctrl Pts',(-3.29989151612973,2.1399077040319,53.6232482519419));
#23497=CARTESIAN_POINT('Ctrl Pts',(-3.36627617471581,2.03753778814412,53.6294048048061));
#23498=CARTESIAN_POINT('Ctrl Pts',(-3.42786414134415,1.9321200930162,53.6355613576702));
#23499=CARTESIAN_POINT('Ctrl Pts',(-3.48438703987511,1.82415349034845,53.6417179105343));
#23500=CARTESIAN_POINT('Ctrl Pts',(-3.53824098958627,1.7212849513727,53.6475837577743));
#23501=CARTESIAN_POINT('Ctrl Pts',(-3.58749715010143,1.61610312423735,53.6534496050142));
#23502=CARTESIAN_POINT('Ctrl Pts',(-3.63197252110668,1.50906083572732,53.6593154522541));
#23503=CARTESIAN_POINT('Ctrl Pts',(-3.67647847221435,1.40194494773806,53.6651853326972));
#23504=CARTESIAN_POINT('Ctrl Pts',(-3.71619694748043,1.29296643767073,53.6710552131403));
#23505=CARTESIAN_POINT('Ctrl Pts',(-3.75099460567478,1.18259395745063,53.6769250935835));
#23506=CARTESIAN_POINT('Ctrl Pts',(-3.78584160708895,1.07206496860795,53.6828032975408));
#23507=CARTESIAN_POINT('Ctrl Pts',(-3.81575376210587,0.960138462149633,
53.6886815014981));
#23508=CARTESIAN_POINT('Ctrl Pts',(-3.84064863891855,0.847293946852686,
53.6945597054554));
#23509=CARTESIAN_POINT('Ctrl Pts',(-3.84427274199704,0.83086646426835,53.6954154324075));
#23510=CARTESIAN_POINT('Ctrl Pts',(-3.84779060633735,0.814419535852366,
53.6962711593596));
#23511=CARTESIAN_POINT('Ctrl Pts',(-3.85120206934889,0.797954648487541,
53.6971268863117));
#23512=CARTESIAN_POINT('Ctrl Pts',(-3.88411142825167,0.639122825967867,
53.7053818271666));
#23513=CARTESIAN_POINT('Ctrl Pts',(-3.90720373726939,0.478193253192053,
53.7136367680216));
#23514=CARTESIAN_POINT('Ctrl Pts',(-3.92027074357112,0.316174472562933,
53.7218917088766));
#23515=CARTESIAN_POINT('Ctrl Pts',(-3.9286499590609,0.212279958017212,53.7271851882461));
#23516=CARTESIAN_POINT('Ctrl Pts',(-3.93290762134356,0.107937899618637,
53.7324786676156));
#23517=CARTESIAN_POINT('Ctrl Pts',(-3.93299851282936,0.00342024591839455,
53.7377721469851));
#23518=CARTESIAN_POINT('',(-3.93299993366718,-0.000722339297042056,54.9877721470192));
#23519=CARTESIAN_POINT('Ctrl Pts',(-3.93299851282984,0.00342024536945145,
53.7377721470129));
#23520=CARTESIAN_POINT('Ctrl Pts',(-3.93309782495112,-0.110780457536849,
53.7435560413447));
#23521=CARTESIAN_POINT('Ctrl Pts',(-3.92821894975723,-0.225136164102259,
53.7493399356766));
#23522=CARTESIAN_POINT('Ctrl Pts',(-3.91834811321992,-0.339171142088976,
53.7551238300084));
#23523=CARTESIAN_POINT('Ctrl Pts',(-3.90842748530965,-0.453781345701163,
53.760936899987));
#23524=CARTESIAN_POINT('Ctrl Pts',(-3.89346434589926,-0.568067143825446,
53.7667499699656));
#23525=CARTESIAN_POINT('Ctrl Pts',(-3.87349782141296,-0.681545029700275,
53.7725630399442));
#23526=CARTESIAN_POINT('Ctrl Pts',(-3.85365782255742,-0.794303818914209,
53.778339273149));
#23527=CARTESIAN_POINT('Ctrl Pts',(-3.82887774495513,-0.906264481991354,
53.7841155063538));
#23528=CARTESIAN_POINT('Ctrl Pts',(-3.79924787160019,-1.01695850954772,
53.7898917395586));
#23529=CARTESIAN_POINT('Ctrl Pts',(-3.76962409111945,-1.12762977477982,
53.7956667849803));
#23530=CARTESIAN_POINT('Ctrl Pts',(-3.73515260675471,-1.23703451145412,
53.801441830402));
#23531=CARTESIAN_POINT('Ctrl Pts',(-3.69597431911322,-1.34471663649098,
53.8072168758238));
#23532=CARTESIAN_POINT('Ctrl Pts',(-3.65679400999867,-1.45240431757759,
53.8129922192192));
#23533=CARTESIAN_POINT('Ctrl Pts',(-3.6129065613013,-1.55836881101843,53.8187675626146));
#23534=CARTESIAN_POINT('Ctrl Pts',(-3.56450172826051,-1.66217220203803,
53.82454290601));
#23535=CARTESIAN_POINT('Ctrl Pts',(-3.51554478973708,-1.76715957444332,
53.830384122967));
#23536=CARTESIAN_POINT('Ctrl Pts',(-3.46196694765328,-1.86993582771499,
53.8362253399241));
#23537=CARTESIAN_POINT('Ctrl Pts',(-3.40401258402014,-1.9700729244961,53.8420665568811));
#23538=CARTESIAN_POINT('Ctrl Pts',(-3.34663156875354,-2.06921935487574,
53.8478499860895));
#23539=CARTESIAN_POINT('Ctrl Pts',(-3.2849605244318,-2.16577828798427,53.8536334152978));
#23540=CARTESIAN_POINT('Ctrl Pts',(-3.21927990030367,-2.25936405289206,
53.8594168445062));
#23541=CARTESIAN_POINT('Ctrl Pts',(-3.15261485968217,-2.35435247454594,
53.8652869553376));
#23542=CARTESIAN_POINT('Ctrl Pts',(-3.08181935582498,-2.44627752267562,
53.871157066169));
#23543=CARTESIAN_POINT('Ctrl Pts',(-3.00722764157043,-2.53477235896536,
53.8770271770004));
#23544=CARTESIAN_POINT('Ctrl Pts',(-2.93263592731587,-2.62326719525511,
53.8828972878317));
#23545=CARTESIAN_POINT('Ctrl Pts',(-2.85424835797467,-2.70833153463351,
53.8887673986631));
#23546=CARTESIAN_POINT('Ctrl Pts',(-2.77243547735778,-2.78963985558853,
53.8946375094945));
#23547=CARTESIAN_POINT('Ctrl Pts',(-2.69052025997408,-2.87104988217497,
53.9005149630348));
#23548=CARTESIAN_POINT('Ctrl Pts',(-2.6048819364985,-2.94898225367245,53.906392416575));
#23549=CARTESIAN_POINT('Ctrl Pts',(-2.51584772932693,-3.0230777698962,53.9122698701153));
#23550=CARTESIAN_POINT('Ctrl Pts',(-2.42692730930555,-3.09707859085731,
53.9181398121753));
#23551=CARTESIAN_POINT('Ctrl Pts',(-2.33461995102914,-3.16725204701039,
53.9240097542353));
#23552=CARTESIAN_POINT('Ctrl Pts',(-2.23929009614874,-3.23327525356104,
53.9298796962953));
#23553=CARTESIAN_POINT('Ctrl Pts',(-2.14405670922281,-3.29923164868424,
53.9357436983346));
#23554=CARTESIAN_POINT('Ctrl Pts',(-2.04580724688095,-3.36104591479999,
53.941607700374));
#23555=CARTESIAN_POINT('Ctrl Pts',(-1.94493913198957,-3.41843542762704,
53.9474717024134));
#23556=CARTESIAN_POINT('Ctrl Pts',(-1.84124687333006,-3.47743175381808,
53.9534998870077));
#23557=CARTESIAN_POINT('Ctrl Pts',(-1.73478749737503,-3.53175160520393,
53.9595280716021));
#23558=CARTESIAN_POINT('Ctrl Pts',(-1.62602496631928,-3.58113554740761,
53.9655562561964));
#23559=CARTESIAN_POINT('Ctrl Pts',(-1.52034376991476,-3.62912040068931,
53.971413657214));
#23560=CARTESIAN_POINT('Ctrl Pts',(-1.41248856738544,-3.67244508538788,
53.9772710582315));
#23561=CARTESIAN_POINT('Ctrl Pts',(-1.30290915295375,-3.71091858427929,
53.983128459249));
#23562=CARTESIAN_POINT('Ctrl Pts',(-1.19334556718039,-3.7493865257047,53.9889850141697));
#23563=CARTESIAN_POINT('Ctrl Pts',(-1.08205865387832,-3.7830045381676,53.9948415690904));
#23564=CARTESIAN_POINT('Ctrl Pts',(-0.969516139116825,-3.81163055082625,
54.0006981240111));
#23565=CARTESIAN_POINT('Ctrl Pts',(-0.856962767843835,-3.84025932491809,
54.0065552438894));
#23566=CARTESIAN_POINT('Ctrl Pts',(-0.743153954117419,-3.86389504022431,
54.0124123637677));
#23567=CARTESIAN_POINT('Ctrl Pts',(-0.628569778541057,-3.88244626923604,
54.0182694836461));
#23568=CARTESIAN_POINT('Ctrl Pts',(-0.508127703087051,-3.90194589484452,
54.024426037732));
#23569=CARTESIAN_POINT('Ctrl Pts',(-0.386829391856616,-3.91582732679284,
54.0305825918179));
#23570=CARTESIAN_POINT('Ctrl Pts',(-0.265239568459779,-3.92404599505705,
54.0367391459039));
#23571=CARTESIAN_POINT('Ctrl Pts',(-0.149391122737724,-3.93187658414514,
54.0426049922546));
#23572=CARTESIAN_POINT('Ctrl Pts',(-0.0332784881345224,-3.93456702174815,
54.0484708386054));
#23573=CARTESIAN_POINT('Ctrl Pts',(0.0826101593482019,-3.93213231740394,
54.0543366849561));
#23574=CARTESIAN_POINT('Ctrl Pts',(0.19857848883911,-3.92969593902059,54.0602065645097));
#23575=CARTESIAN_POINT('Ctrl Pts',(0.314322114061851,-3.92212742860087,
54.0660764440632));
#23576=CARTESIAN_POINT('Ctrl Pts',(0.429358388695931,-3.90949362118119,
54.0719463236167));
#23577=CARTESIAN_POINT('Ctrl Pts',(0.544557785348789,-3.89684189895874,
54.0778245266892));
#23578=CARTESIAN_POINT('Ctrl Pts',(0.659047424167076,-3.87911061047516,
54.0837027297616));
#23579=CARTESIAN_POINT('Ctrl Pts',(0.772355239372889,-3.85641755833224,
54.089580932834));
#23580=CARTESIAN_POINT('Ctrl Pts',(0.788850291906667,-3.85311396372521,
54.0904366661151));
#23581=CARTESIAN_POINT('Ctrl Pts',(0.805320326206703,-3.84970530131541,
54.0912923993963));
#23582=CARTESIAN_POINT('Ctrl Pts',(0.82176391592408,-3.84619202153053,54.0921481326774));
#23583=CARTESIAN_POINT('Ctrl Pts',(0.93470382495127,-3.822061676143,54.0980255864806));
#23584=CARTESIAN_POINT('Ctrl Pts',(1.0467651161977,-3.79291300036868,54.1039030402837));
#23585=CARTESIAN_POINT('Ctrl Pts',(1.15746816109081,-3.7588238128517,54.1097804940869));
#23586=CARTESIAN_POINT('Ctrl Pts',(1.26802972579053,-3.72477819184048,54.1156504364138));
#23587=CARTESIAN_POINT('Ctrl Pts',(1.37723610560554,-3.68580473651154,54.1215203787406));
#23588=CARTESIAN_POINT('Ctrl Pts',(1.48461775345995,-3.64203227966358,54.1273903210675));
#23589=CARTESIAN_POINT('Ctrl Pts',(1.59189073775631,-3.5983041178232,54.1332543233773));
#23590=CARTESIAN_POINT('Ctrl Pts',(1.69734228333967,-3.54978676925473,54.1391183256871));
#23591=CARTESIAN_POINT('Ctrl Pts',(1.80051854434761,-3.49665868672656,54.1449823279969));
#23592=CARTESIAN_POINT('Ctrl Pts',(1.90658356682353,-3.44204310740237,54.1510105124912));
#23593=CARTESIAN_POINT('Ctrl Pts',(2.01024358749085,-3.3825549190365,54.1570386969855));
#23594=CARTESIAN_POINT('Ctrl Pts',(2.11102782971279,-3.31844097464127,54.1630668814798));
#23595=CARTESIAN_POINT('Ctrl Pts',(2.20895677523108,-3.25614342862393,54.1689242827749));
#23596=CARTESIAN_POINT('Ctrl Pts',(2.30417032999127,-3.18947894643206,54.17478168407));
#23597=CARTESIAN_POINT('Ctrl Pts',(2.3962627612175,-3.11871989431597,54.1806390853651));
#23598=CARTESIAN_POINT('Ctrl Pts',(2.48834188980075,-3.04797106326143,54.1864956405655));
#23599=CARTESIAN_POINT('Ctrl Pts',(2.57730046434993,-2.97312908966979,54.1923521957659));
#23600=CARTESIAN_POINT('Ctrl Pts',(2.66276395042939,-2.89450810057489,54.1982087509663));
#23601=CARTESIAN_POINT('Ctrl Pts',(2.7482356808452,-2.8158795272132,54.2040658711262));
#23602=CARTESIAN_POINT('Ctrl Pts',(2.8302113489587,-2.73347149294836,54.2099229912862));
#23603=CARTESIAN_POINT('Ctrl Pts',(2.9083520871297,-2.6476361414077,54.2157801114461));
#23604=CARTESIAN_POINT('Ctrl Pts',(2.99048761408882,-2.55741262937631,54.2219366651473));
#23605=CARTESIAN_POINT('Ctrl Pts',(3.06838538698437,-2.4634024735282,54.2280932188485));
#23606=CARTESIAN_POINT('Ctrl Pts',(3.14169953943729,-2.36605431127425,54.2342497725496));
#23607=CARTESIAN_POINT('Ctrl Pts',(3.21155186190543,-2.27330284387086,54.2401156191841));
#23608=CARTESIAN_POINT('Ctrl Pts',(3.27724335250574,-2.17752178313405,54.2459814658186));
#23609=CARTESIAN_POINT('Ctrl Pts',(3.33851986779332,-2.0791282048852,54.2518473124531));
#23610=CARTESIAN_POINT('Ctrl Pts',(3.39983851521797,-1.98066697377286,54.2577171922911));
#23611=CARTESIAN_POINT('Ctrl Pts',(3.45673594091564,-1.87959000676744,54.2635870721291));
#23612=CARTESIAN_POINT('Ctrl Pts',(3.50900442940083,-1.77633806310771,54.269456951967));
#23613=CARTESIAN_POINT('Ctrl Pts',(3.56134703485703,-1.67293970768946,54.2753351553232));
#23614=CARTESIAN_POINT('Ctrl Pts',(3.60904743658074,-1.56736059581798,54.2812133586793));
#23615=CARTESIAN_POINT('Ctrl Pts',(3.65194638801383,-1.46006047103285,54.2870915620355));
#23616=CARTESIAN_POINT('Ctrl Pts',(3.65819148914052,-1.44444003958164,54.2879472933104));
#23617=CARTESIAN_POINT('Ctrl Pts',(3.66433492174529,-1.42878315875044,54.2888030245853));
#23618=CARTESIAN_POINT('Ctrl Pts',(3.67037628380472,-1.41309126926883,54.2896587558602));
#23619=CARTESIAN_POINT('Ctrl Pts',(3.71187041501763,-1.30531403050651,54.2955362095627));
#23620=CARTESIAN_POINT('Ctrl Pts',(3.74868137511156,-1.19553092150226,54.3014136632652));
#23621=CARTESIAN_POINT('Ctrl Pts',(3.78061229675617,-1.0841861747947,54.3072911169677));
#23622=CARTESIAN_POINT('Ctrl Pts',(3.81250241018582,-0.972983728406827,
54.3131610591929));
#23623=CARTESIAN_POINT('Ctrl Pts',(3.83952477586845,-0.860224006467499,
54.319031001418));
#23624=CARTESIAN_POINT('Ctrl Pts',(3.86153076176818,-0.746370669250853,
54.3249009436432));
#23625=CARTESIAN_POINT('Ctrl Pts',(3.88351447897329,-0.632632544559086,
54.3307649458505));
#23626=CARTESIAN_POINT('Ctrl Pts',(3.90049183611031,-0.51780340861447,54.3366289480577));
#23627=CARTESIAN_POINT('Ctrl Pts',(3.91236433905862,-0.402360880879767,
54.3424929502649));
#23628=CARTESIAN_POINT('Ctrl Pts',(3.92456925237632,-0.283686154049728,
54.3485211347974));
#23629=CARTESIAN_POINT('Ctrl Pts',(3.93137910493229,-0.164363605648615,
54.3545493193298));
#23630=CARTESIAN_POINT('Ctrl Pts',(3.93274344159755,-0.0449224061170324,
54.3605775038622));
#23631=CARTESIAN_POINT('Ctrl Pts',(3.93406912550207,0.0711349276675845,
54.3664349050533));
#23632=CARTESIAN_POINT('Ctrl Pts',(3.93025369795782,0.187303840308811,54.3722923062443));
#23633=CARTESIAN_POINT('Ctrl Pts',(3.92130360932623,0.303095700208723,54.3781497074353));
#23634=CARTESIAN_POINT('Ctrl Pts',(3.91235481352498,0.418870834103377,54.3840062625313));
#23635=CARTESIAN_POINT('Ctrl Pts',(3.89827286330148,0.53426861239305,54.3898628176272));
#23636=CARTESIAN_POINT('Ctrl Pts',(3.87911623126424,0.648803717885653,54.3957193727232));
#23637=CARTESIAN_POINT('Ctrl Pts',(3.85995775126064,0.763349872137798,54.4015764927784));
#23638=CARTESIAN_POINT('Ctrl Pts',(3.83572368434281,0.877032781296482,54.4074336128336));
#23639=CARTESIAN_POINT('Ctrl Pts',(3.8065238307318,0.989376230799395,54.4132907328889));
#23640=CARTESIAN_POINT('Ctrl Pts',(3.77583119179622,1.10746301912048,54.4194472867351));
#23641=CARTESIAN_POINT('Ctrl Pts',(3.7396517263843,1.22406927734305,54.4256038405813));
#23642=CARTESIAN_POINT('Ctrl Pts',(3.6981722300468,1.33866020965388,54.4317603944275));
#23643=CARTESIAN_POINT('Ctrl Pts',(3.65865136078463,1.44784025411824,54.4376262409575));
#23644=CARTESIAN_POINT('Ctrl Pts',(3.61431976499308,1.55519058108515,54.4434920874876));
#23645=CARTESIAN_POINT('Ctrl Pts',(3.56538791635528,1.66027046167415,54.4493579340177));
#23646=CARTESIAN_POINT('Ctrl Pts',(3.51642242345009,1.765422592458,54.4552278137514));
#23647=CARTESIAN_POINT('Ctrl Pts',(3.46285056939417,1.86830080349583,54.4610976934851));
#23648=CARTESIAN_POINT('Ctrl Pts',(3.40492802998567,1.96849031255372,54.4669675732188));
#23649=CARTESIAN_POINT('Ctrl Pts',(3.34692335612531,2.06882189083876,54.4728457764715));
#23650=CARTESIAN_POINT('Ctrl Pts',(3.28455590784092,2.16645681346466,54.4787239797241));
#23651=CARTESIAN_POINT('Ctrl Pts',(3.2181237423487,2.2610105216322,54.4846021829768));
#23652=CARTESIAN_POINT('Ctrl Pts',(3.208452737644,2.27477538011242,54.4854579149989));
#23653=CARTESIAN_POINT('Ctrl Pts',(3.19869565778891,2.28847499937988,54.4863136470211));
#23654=CARTESIAN_POINT('Ctrl Pts',(3.18885348983417,2.30210825557191,54.4871693790432));
#23655=CARTESIAN_POINT('Ctrl Pts',(3.12125418902311,2.39574601816625,54.4930468327347));
#23656=CARTESIAN_POINT('Ctrl Pts',(3.04941620835264,2.48655726347727,54.4989242864262));
#23657=CARTESIAN_POINT('Ctrl Pts',(2.97360405959491,2.57413439757147,54.5048017401177));
#23658=CARTESIAN_POINT('Ctrl Pts',(2.89788879994943,2.66159960671807,54.5106716823315));
#23659=CARTESIAN_POINT('Ctrl Pts',(2.81820974078964,2.74583861555468,54.5165416245452));
#23660=CARTESIAN_POINT('Ctrl Pts',(2.73487401906295,2.82647361563033,54.5224115667589));
#23661=CARTESIAN_POINT('Ctrl Pts',(2.65162262793072,2.90702701807475,54.5282755689543));
#23662=CARTESIAN_POINT('Ctrl Pts',(2.56472222951902,2.98398338113534,54.5341395711497));
#23663=CARTESIAN_POINT('Ctrl Pts',(2.47451904522582,3.0569992631361,54.5400035733451));
#23664=CARTESIAN_POINT('Ctrl Pts',(2.38179032129292,3.13205946880198,54.5460317578818));
#23665=CARTESIAN_POINT('Ctrl Pts',(2.28557142029616,3.2029549394754,54.5520599424185));
#23666=CARTESIAN_POINT('Ctrl Pts',(2.18627798661554,3.269354304024,54.5580881269552));
#23667=CARTESIAN_POINT('Ctrl Pts',(2.0897976164662,3.33387252070624,54.5639455281334));
#23668=CARTESIAN_POINT('Ctrl Pts',(1.990414948337,3.39414572349081,54.5698029293116));
#23669=CARTESIAN_POINT('Ctrl Pts',(1.88854276329811,3.44991235123362,54.5756603304899));
#23670=CARTESIAN_POINT('Ctrl Pts',(1.78668529358891,3.50567092354586,54.5815168855726));
#23671=CARTESIAN_POINT('Ctrl Pts',(1.68233938380184,3.55692401726563,54.5873734406554));
#23672=CARTESIAN_POINT('Ctrl Pts',(1.57594346133791,3.6034554536814,54.5932299957382));
#23673=CARTESIAN_POINT('Ctrl Pts',(1.46953727527553,3.64999137880283,54.59908711578));
#23674=CARTESIAN_POINT('Ctrl Pts',(1.36108106136615,3.6918045758734,54.6049442358217));
#23675=CARTESIAN_POINT('Ctrl Pts',(1.25103366585959,3.72872682921207,54.6108013558635));
#23676=CARTESIAN_POINT('Ctrl Pts',(1.13536031220635,3.76753666063479,54.616957909727));
#23677=CARTESIAN_POINT('Ctrl Pts',(1.01792926161511,3.80094207385933,54.6231144635905));
#23678=CARTESIAN_POINT('Ctrl Pts',(0.899290491862966,3.82880733535194,54.6292710174541));
#23679=CARTESIAN_POINT('Ctrl Pts',(0.786253746042588,3.85535682239686,54.63513686397));
#23680=CARTESIAN_POINT('Ctrl Pts',(0.672121154680575,3.87687738528061,54.6410027104859));
#23681=CARTESIAN_POINT('Ctrl Pts',(0.5573768456465,3.89330451569578,54.6468685570018));
#23682=CARTESIAN_POINT('Ctrl Pts',(0.44255364141266,3.90974294097818,54.6527384367211));
#23683=CARTESIAN_POINT('Ctrl Pts',(0.327118291381488,3.9210809200646,54.6586083164404));
#23684=CARTESIAN_POINT('Ctrl Pts',(0.211557887780263,3.92730597994579,54.6644781961596));
#23685=CARTESIAN_POINT('Ctrl Pts',(0.0958336189511281,3.9335398669929,54.6703563993976));
#23686=CARTESIAN_POINT('Ctrl Pts',(-0.0200156466463229,3.9346463640566,
54.6762346026355));
#23687=CARTESIAN_POINT('Ctrl Pts',(-0.135504975568601,3.9306650075523,54.6821128058735));
#23688=CARTESIAN_POINT('Ctrl Pts',(-0.152317583773183,3.93008541299016,
54.682968537991));
#23689=CARTESIAN_POINT('Ctrl Pts',(-0.169122577528871,3.92939808212121,
54.6838242701085));
#23690=CARTESIAN_POINT('Ctrl Pts',(-0.18591847626111,3.92860322763508,54.684680002226));
#23691=CARTESIAN_POINT('Ctrl Pts',(-0.30127831319858,3.92314390179777,54.6905574559491));
#23692=CARTESIAN_POINT('Ctrl Pts',(-0.416586581313027,3.91259017234618,
54.6964349096721));
#23693=CARTESIAN_POINT('Ctrl Pts',(-0.531357381452448,3.89694089423692,
54.7023123633952));
#23694=CARTESIAN_POINT('Ctrl Pts',(-0.645981502723869,3.88131161614852,
54.708182305641));
#23695=CARTESIAN_POINT('Ctrl Pts',(-0.760069116991416,3.86059979579573,
54.7140522478868));
#23696=CARTESIAN_POINT('Ctrl Pts',(-0.873135983901122,3.83485626244544,
54.7199221901326));
#23697=CARTESIAN_POINT('Ctrl Pts',(-0.986088434146258,3.80913877995604,
54.7257861923605));
#23698=CARTESIAN_POINT('Ctrl Pts',(-1.09802179182215,3.7783998039262,54.7316501945884));
#23699=CARTESIAN_POINT('Ctrl Pts',(-1.20845924694091,3.74274167536086,54.7375141968163));
#23700=CARTESIAN_POINT('Ctrl Pts',(-1.3219887668866,3.70608517857875,54.743542381341));
#23701=CARTESIAN_POINT('Ctrl Pts',(-1.43393693989953,3.66423005744842,54.7495705658657));
#23702=CARTESIAN_POINT('Ctrl Pts',(-1.54379913655438,3.61734339342756,54.7555987503903));
#23703=CARTESIAN_POINT('Ctrl Pts',(-1.65054884887056,3.57178506628599,54.761456151602));
#23704=CARTESIAN_POINT('Ctrl Pts',(-1.75532878853956,3.5214766367418,54.7673135528136));
#23705=CARTESIAN_POINT('Ctrl Pts',(-1.85769436035273,3.4666209287307,54.7731709540253));
#23706=CARTESIAN_POINT('Ctrl Pts',(-1.96004514557197,3.41177314456612,54.7790275091418));
#23707=CARTESIAN_POINT('Ctrl Pts',(-2.0599818929475,3.35237958288713,54.7848840642583));
#23708=CARTESIAN_POINT('Ctrl Pts',(-2.15708400579163,3.28868934257372,54.7907406193748));
#23709=CARTESIAN_POINT('Ctrl Pts',(-2.25419548570091,3.22499295830925,54.7965977394505));
#23710=CARTESIAN_POINT('Ctrl Pts',(-2.34847144255498,3.15699929770198,54.8024548595262));
#23711=CARTESIAN_POINT('Ctrl Pts',(-2.43952029561827,3.08500076616954,54.8083119796019));
#23712=CARTESIAN_POINT('Ctrl Pts',(-2.53522384217987,3.00932145135058,54.8144685334192));
#23713=CARTESIAN_POINT('Ctrl Pts',(-2.62736119639072,2.92921726301465,54.8206250872364));
#23714=CARTESIAN_POINT('Ctrl Pts',(-2.71551819351257,2.8450746810413,54.8267816410537));
#23715=CARTESIAN_POINT('Ctrl Pts',(-2.7995124917498,2.76490524066267,54.8326474876038));
#23716=CARTESIAN_POINT('Ctrl Pts',(-2.87989349302675,2.68107041608969,54.838513334154));
#23717=CARTESIAN_POINT('Ctrl Pts',(-2.95634266486319,2.59394044802684,54.8443791807041));
#23718=CARTESIAN_POINT('Ctrl Pts',(-3.03284440116098,2.50675057166507,54.8502490604578));
#23719=CARTESIAN_POINT('Ctrl Pts',(-3.10540866752619,2.41626136128656,54.8561189402114));
#23720=CARTESIAN_POINT('Ctrl Pts',(-3.17375889444228,2.32287396988054,54.861988819965));
#23721=CARTESIAN_POINT('Ctrl Pts',(-3.24220604231983,2.22935415468938,54.8678670232373));
#23722=CARTESIAN_POINT('Ctrl Pts',(-3.30642699960994,2.13292829994122,54.8737452265095));
#23723=CARTESIAN_POINT('Ctrl Pts',(-3.36618993711564,2.03402416584992,54.8796234297818));
#23724=CARTESIAN_POINT('Ctrl Pts',(-3.37489005316125,2.0196259873149,54.8804791616575));
#23725=CARTESIAN_POINT('Ctrl Pts',(-3.38349577378783,2.00517532465565,54.8813348935332));
#23726=CARTESIAN_POINT('Ctrl Pts',(-3.39200646822428,1.99067353413982,54.8821906254089));
#23727=CARTESIAN_POINT('Ctrl Pts',(-3.45257231638009,1.88747240890521,54.8882803901434));
#23728=CARTESIAN_POINT('Ctrl Pts',(-3.50850811753915,1.78136280708782,54.8943701548779));
#23729=CARTESIAN_POINT('Ctrl Pts',(-3.55953522084632,1.67278151937264,54.9004599196124));
#23730=CARTESIAN_POINT('Ctrl Pts',(-3.61048076066794,1.56437379174058,54.9065399502564));
#23731=CARTESIAN_POINT('Ctrl Pts',(-3.65653306873914,1.45350257799546,54.9126199809005));
#23732=CARTESIAN_POINT('Ctrl Pts',(-3.69745819945993,1.34063114362101,54.9187000115446));
#23733=CARTESIAN_POINT('Ctrl Pts',(-3.73830444202521,1.22797728263267,54.9247683221918));
#23734=CARTESIAN_POINT('Ctrl Pts',(-3.77404307991574,1.11333123252545,54.930836632839));
#23735=CARTESIAN_POINT('Ctrl Pts',(-3.80448766304021,0.997177327146436,
54.9369049434862));
#23736=CARTESIAN_POINT('Ctrl Pts',(-3.83489764772554,0.881155423700603,
54.9429663578631));
#23737=CARTESIAN_POINT('Ctrl Pts',(-3.86002546094088,0.763629433070065,
54.9490277722399));
#23738=CARTESIAN_POINT('Ctrl Pts',(-3.8797337597261,0.645100731391357,54.9550891866167));
#23739=CARTESIAN_POINT('Ctrl Pts',(-3.89941659063284,0.526725197401228,
54.9611427681833));
#23740=CARTESIAN_POINT('Ctrl Pts',(-3.91369380347358,0.407349899215915,
54.9671963497499));
#23741=CARTESIAN_POINT('Ctrl Pts',(-3.92247878698497,0.28748767913248,54.9732499313165));
#23742=CARTESIAN_POINT('Ctrl Pts',(-3.92950368752218,0.191640012126227,
54.9780906698727));
#23743=CARTESIAN_POINT('Ctrl Pts',(-3.93301760252523,0.0954813188314772,
54.9829314084289));
#23744=CARTESIAN_POINT('Ctrl Pts',(-3.9329999336673,-0.000722338618901584,
54.9877721469851));
#23745=CARTESIAN_POINT('',(-3.93299903070378,-0.00276124668366289,56.2377721469449));
#23746=CARTESIAN_POINT('Ctrl Pts',(-3.93299993366718,-0.000722339297067472,
54.9877721470192));
#23747=CARTESIAN_POINT('Ctrl Pts',(-3.93297720821431,-0.124458103037193,
54.9939982354881));
#23748=CARTESIAN_POINT('Ctrl Pts',(-3.927110968723,-0.248049901650573,55.0002243239571));
#23749=CARTESIAN_POINT('Ctrl Pts',(-3.91546729987528,-0.370951241549993,
55.006450412426));
#23750=CARTESIAN_POINT('Ctrl Pts',(-3.90378573984742,-0.494252530715322,
55.0126967620208));
#23751=CARTESIAN_POINT('Ctrl Pts',(-3.88628916959009,-0.616858538656386,
55.0189431116155));
#23752=CARTESIAN_POINT('Ctrl Pts',(-3.86309533707472,-0.738229921279,55.0251894612103));
#23753=CARTESIAN_POINT('Ctrl Pts',(-3.83986373499779,-0.859798948853376,
55.0314459825559));
#23754=CARTESIAN_POINT('Ctrl Pts',(-3.81091642630633,-0.980129019685123,
55.0377025039015));
#23755=CARTESIAN_POINT('Ctrl Pts',(-3.77642124542311,-1.09869539778642,
55.0439590252471));
#23756=CARTESIAN_POINT('Ctrl Pts',(-3.74182559238293,-1.21760711745272,
55.0502337696075));
#23757=CARTESIAN_POINT('Ctrl Pts',(-3.70164984674111,-1.33474455662902,
55.056508513968));
#23758=CARTESIAN_POINT('Ctrl Pts',(-3.65611105196853,-1.44960028134435,
55.0627832583285));
#23759=CARTESIAN_POINT('Ctrl Pts',(-3.61518375983273,-1.5528250992687,55.0684225884162));
#23760=CARTESIAN_POINT('Ctrl Pts',(-3.56992532214057,-1.65420707183091,
55.0740619185039));
#23761=CARTESIAN_POINT('Ctrl Pts',(-3.52052443902146,-1.7533957551713,55.0797012485916));
#23762=CARTESIAN_POINT('Ctrl Pts',(-3.46903757814324,-1.85677273180402,
55.0855787022998));
#23763=CARTESIAN_POINT('Ctrl Pts',(-3.41290911103248,-1.95804944682947,
55.0914561560079));
#23764=CARTESIAN_POINT('Ctrl Pts',(-3.35233380913251,-2.05678074479201,
55.097333609716));
#23765=CARTESIAN_POINT('Ctrl Pts',(-3.29183592341283,-2.15538586261638,
55.1032035519466));
#23766=CARTESIAN_POINT('Ctrl Pts',(-3.22690271905573,-2.25145168448782,
55.1090734941773));
#23767=CARTESIAN_POINT('Ctrl Pts',(-3.15777586579413,-2.34455551894345,
55.1149434364079));
#23768=CARTESIAN_POINT('Ctrl Pts',(-3.08871896462757,-2.43756513808378,
55.1208074386205));
#23769=CARTESIAN_POINT('Ctrl Pts',(-3.01547710049811,-2.52761840275179,
55.1266714408331));
#23770=CARTESIAN_POINT('Ctrl Pts',(-2.93833609211701,-2.61432018118719,
55.1325354430456));
#23771=CARTESIAN_POINT('Ctrl Pts',(-2.8590352636858,-2.70344946534716,55.138563627576));
#23772=CARTESIAN_POINT('Ctrl Pts',(-2.77561395333189,-2.78903643640921,
55.1445918121064));
#23773=CARTESIAN_POINT('Ctrl Pts',(-2.68842844146174,-2.87068659298427,
55.1506199966367));
#23774=CARTESIAN_POINT('Ctrl Pts',(-2.60371296552938,-2.95002353470586,
55.1564773978327));
#23775=CARTESIAN_POINT('Ctrl Pts',(-2.51544403133708,-3.0256434330798,55.1623347990287));
#23776=CARTESIAN_POINT('Ctrl Pts',(-2.42398643669716,-3.09722113429253,
55.1681922002246));
#23777=CARTESIAN_POINT('Ctrl Pts',(-2.3325420530075,-3.16878849618401,55.1740487553254));
#23778=CARTESIAN_POINT('Ctrl Pts',(-2.23791024954299,-3.23631456783101,
55.1799053104261));
#23779=CARTESIAN_POINT('Ctrl Pts',(-2.1404885033547,-3.29951480781741,55.1857618655268));
#23780=CARTESIAN_POINT('Ctrl Pts',(-2.04305735926919,-3.36272114448535,
55.1916189855866));
#23781=CARTESIAN_POINT('Ctrl Pts',(-1.94283608351721,-3.42160059543853,
55.1974761056465));
#23782=CARTESIAN_POINT('Ctrl Pts',(-1.84025009366266,-3.47591262732173,
55.2033332257063));
#23783=CARTESIAN_POINT('Ctrl Pts',(-1.7324195962137,-3.53300125534718,55.2094897795453));
#23784=CARTESIAN_POINT('Ctrl Pts',(-1.62197665314596,-3.58504286822423,
55.2156463333843));
#23785=CARTESIAN_POINT('Ctrl Pts',(-1.50944188025276,-3.63181417615757,
55.2218028872234));
#23786=CARTESIAN_POINT('Ctrl Pts',(-1.40222090488008,-3.67637698218755,
55.2276687337576));
#23787=CARTESIAN_POINT('Ctrl Pts',(-1.29310155049033,-3.71615574044766,
55.2335345802918));
#23788=CARTESIAN_POINT('Ctrl Pts',(-1.18255103060521,-3.751008139156,55.239400426826));
#23789=CARTESIAN_POINT('Ctrl Pts',(-1.07192449905926,-3.7858845014668,55.2452703065637));
#23790=CARTESIAN_POINT('Ctrl Pts',(-0.959865239997425,-3.8158276532582,
55.2511401863014));
#23791=CARTESIAN_POINT('Ctrl Pts',(-0.846851846557203,-3.84074614495448,
55.257010066039));
#23792=CARTESIAN_POINT('Ctrl Pts',(-0.733678199562052,-3.86569997119612,
55.2628882692954));
#23793=CARTESIAN_POINT('Ctrl Pts',(-0.619548123036424,-3.8856148496232,
55.2687664725518));
#23794=CARTESIAN_POINT('Ctrl Pts',(-0.504946530464559,-3.90045099973988,
55.2746446758081));
#23795=CARTESIAN_POINT('Ctrl Pts',(-0.488263158955069,-3.90261080396783,
55.275500407797));
#23796=CARTESIAN_POINT('Ctrl Pts',(-0.471569795818275,-3.90466306633423,
55.2763561397858));
#23797=CARTESIAN_POINT('Ctrl Pts',(-0.454867936511775,-3.90660775614004,
55.2772118717746));
#23798=CARTESIAN_POINT('Ctrl Pts',(-0.340153976662304,-3.91996453661635,
55.2830893254884));
#23799=CARTESIAN_POINT('Ctrl Pts',(-0.224663166259439,-3.92828622915271,
55.2889667792022));
#23800=CARTESIAN_POINT('Ctrl Pts',(-0.108874761772659,-3.93149275546184,
55.294844232916));
#23801=CARTESIAN_POINT('Ctrl Pts',(0.00676566332945326,-3.9346951837804,
55.3007141751524));
#23802=CARTESIAN_POINT('Ctrl Pts',(0.122702517450103,-3.93279543557375,
55.3065841173888));
#23803=CARTESIAN_POINT('Ctrl Pts',(0.238449736136254,-3.92576498574947,
55.3124540596252));
#23804=CARTESIAN_POINT('Ctrl Pts',(0.354079825805363,-3.91874165030502,
55.3183180618436));
#23805=CARTESIAN_POINT('Ctrl Pts',(0.469520252391502,-3.90659796577246,
55.3241820640619));
#23806=CARTESIAN_POINT('Ctrl Pts',(0.584283913491771,-3.88935744158784,
55.3300460662803));
#23807=CARTESIAN_POINT('Ctrl Pts',(0.702260766242369,-3.87163421139833,
55.3360742508085));
#23808=CARTESIAN_POINT('Ctrl Pts',(0.819521952844152,-3.84852450042129,
55.3421024353367));
#23809=CARTESIAN_POINT('Ctrl Pts',(0.935542402147672,-3.82011117819675,
55.348130619865));
#23810=CARTESIAN_POINT('Ctrl Pts',(1.04827589861093,-3.79250282829172,55.3539880210668));
#23811=CARTESIAN_POINT('Ctrl Pts',(1.15983758917749,-3.75988744853935,55.3598454222687));
#23812=CARTESIAN_POINT('Ctrl Pts',(1.26975583177661,-3.72239293031636,55.3657028234706));
#23813=CARTESIAN_POINT('Ctrl Pts',(1.37965819680554,-3.68490382813562,55.3715593785772));
#23814=CARTESIAN_POINT('Ctrl Pts',(1.48791719562057,-3.64253712211225,55.3774159336839));
#23815=CARTESIAN_POINT('Ctrl Pts',(1.59407734706772,-3.59547026292327,55.3832724887905));
#23816=CARTESIAN_POINT('Ctrl Pts',(1.70024773937251,-3.54839886337712,55.3891296088563));
#23817=CARTESIAN_POINT('Ctrl Pts',(1.8043185047075,-3.49662657653291,55.3949867289221));
#23818=CARTESIAN_POINT('Ctrl Pts',(1.90585575589902,-3.44037829863324,55.4008438489879));
#23819=CARTESIAN_POINT('Ctrl Pts',(2.01258389972579,-3.38125443794923,55.4070004028187));
#23820=CARTESIAN_POINT('Ctrl Pts',(2.11651218828637,-3.31718506977655,55.4131569566495));
#23821=CARTESIAN_POINT('Ctrl Pts',(2.2171691653615,-3.24848424533199,55.4193135104803));
#23822=CARTESIAN_POINT('Ctrl Pts',(2.31307320469071,-3.183027416,55.4251793570205));
#23823=CARTESIAN_POINT('Ctrl Pts',(2.40600750894773,-3.11336682291932,55.4310452035606));
#23824=CARTESIAN_POINT('Ctrl Pts',(2.49559762194041,-3.03981603215809,55.4369110501008));
#23825=CARTESIAN_POINT('Ctrl Pts',(2.58524933476359,-2.96621466978696,55.4427809298444));
#23826=CARTESIAN_POINT('Ctrl Pts',(2.67155197165439,-2.88871805843014,55.4486508095881));
#23827=CARTESIAN_POINT('Ctrl Pts',(2.7541674591796,-2.80767708378227,55.4545206893317));
#23828=CARTESIAN_POINT('Ctrl Pts',(2.83690009587701,-2.7265211926293,55.460398892594));
#23829=CARTESIAN_POINT('Ctrl Pts',(2.91593487038186,-2.64181120977399,55.4662770958563));
#23830=CARTESIAN_POINT('Ctrl Pts',(2.99097353195254,-2.55393154394539,55.4721552991186));
#23831=CARTESIAN_POINT('Ctrl Pts',(3.0018974447618,-2.54113827462096,55.4730110310649));
#23832=CARTESIAN_POINT('Ctrl Pts',(3.01273674403921,-2.52827788128809,55.4738667630112));
#23833=CARTESIAN_POINT('Ctrl Pts',(3.02349058702999,-2.51535159970549,55.4747224949575));
#23834=CARTESIAN_POINT('Ctrl Pts',(3.09735158361245,-2.42656956702987,55.4805999486653));
#23835=CARTESIAN_POINT('Ctrl Pts',(3.16741983797865,-2.33438595917166,55.4864774023732));
#23836=CARTESIAN_POINT('Ctrl Pts',(3.23336643838967,-2.23915843010164,55.4923548560811));
#23837=CARTESIAN_POINT('Ctrl Pts',(3.29922875801771,-2.14405260329771,55.4982247983115));
#23838=CARTESIAN_POINT('Ctrl Pts',(3.36097966677623,-2.04591092800972,55.5040947405419));
#23839=CARTESIAN_POINT('Ctrl Pts',(3.41832971213729,-1.94512492635288,55.5099646827724));
#23840=CARTESIAN_POINT('Ctrl Pts',(3.475621722804,-1.84444091388829,55.5158286849848));
#23841=CARTESIAN_POINT('Ctrl Pts',(3.52852152580334,-1.74111825431264,55.5216926871972));
#23842=CARTESIAN_POINT('Ctrl Pts',(3.57678268341861,-1.63557776812864,55.5275566894096));
#23843=CARTESIAN_POINT('Ctrl Pts',(3.62639507325392,-1.52708232370292,55.5335848739401));
#23844=CARTESIAN_POINT('Ctrl Pts',(3.67110497330673,-1.41624338886802,55.5396130584705));
#23845=CARTESIAN_POINT('Ctrl Pts',(3.71069491913246,-1.30354601649673,55.545641243001));
#23846=CARTESIAN_POINT('Ctrl Pts',(3.74916324983053,-1.19404145166942,55.5514986441969));
#23847=CARTESIAN_POINT('Ctrl Pts',(3.78279769085203,-1.08278275245442,55.5573560453928));
#23848=CARTESIAN_POINT('Ctrl Pts',(3.81144767707452,-0.970234819475773,
55.5632134465887));
#23849=CARTESIAN_POINT('Ctrl Pts',(3.8400935248378,-0.857703143923043,55.5690700016895));
#23850=CARTESIAN_POINT('Ctrl Pts',(3.86375624780682,-0.743883004576842,
55.5749265567902));
#23851=CARTESIAN_POINT('Ctrl Pts',(3.88233561911942,-0.629252843073858,
55.5807831118909));
#23852=CARTESIAN_POINT('Ctrl Pts',(3.9009167827119,-0.514611623643904,55.5866402319508));
#23853=CARTESIAN_POINT('Ctrl Pts',(3.91441355383479,-0.399160633925395,
55.5924973520106));
#23854=CARTESIAN_POINT('Ctrl Pts',(3.92277724186476,-0.283386151227936,
55.5983544720705));
#23855=CARTESIAN_POINT('Ctrl Pts',(3.93156850704697,-0.161692925096254,
55.6045110259097));
#23856=CARTESIAN_POINT('Ctrl Pts',(3.93468792686195,-0.0396427617862714,
55.6106675797488));
#23857=CARTESIAN_POINT('Ctrl Pts',(3.93214095724448,0.0821978853767393,
55.616824133588));
#23858=CARTESIAN_POINT('Ctrl Pts',(3.92971425339454,0.198285319447808,55.6226899801223));
#23859=CARTESIAN_POINT('Ctrl Pts',(3.92214414325636,0.314182155224603,55.6285558266567));
#23860=CARTESIAN_POINT('Ctrl Pts',(3.90948867235328,0.429403447519139,55.6344216731911));
#23861=CARTESIAN_POINT('Ctrl Pts',(3.89682449987763,0.544703962976815,55.6402915529289));
#23862=CARTESIAN_POINT('Ctrl Pts',(3.87906806714342,0.659327603541924,55.6461614326668));
#23863=CARTESIAN_POINT('Ctrl Pts',(3.85632855470308,0.77279950710489,55.6520313124047));
#23864=CARTESIAN_POINT('Ctrl Pts',(3.83355679752063,0.886432314393349,55.6579095156613));
#23865=CARTESIAN_POINT('Ctrl Pts',(3.80578795958185,0.998909727187948,55.6637877189179));
#23866=CARTESIAN_POINT('Ctrl Pts',(3.77318105601108,1.10977192186461,55.6696659221745));
#23867=CARTESIAN_POINT('Ctrl Pts',(3.76843423641047,1.12591092253712,55.6705216541631));
#23868=CARTESIAN_POINT('Ctrl Pts',(3.76358496803087,1.1420157277089,55.6713773861517));
#23869=CARTESIAN_POINT('Ctrl Pts',(3.75863382545225,1.15808495636809,55.6722331181403));
#23870=CARTESIAN_POINT('Ctrl Pts',(3.72462772109122,1.26845379711713,55.6781105718487));
#23871=CARTESIAN_POINT('Ctrl Pts',(3.6857004396103,1.37750444857909,55.6839880255571));
#23872=CARTESIAN_POINT('Ctrl Pts',(3.64197183586831,1.4847660242415,55.6898654792655));
#23873=CARTESIAN_POINT('Ctrl Pts',(3.59829911796362,1.59189051793806,55.6957354214964));
#23874=CARTESIAN_POINT('Ctrl Pts',(3.54983743547528,1.69723010447361,55.7016053637274));
#23875=CARTESIAN_POINT('Ctrl Pts',(3.49675656829594,1.80032844283455,55.7074753059583));
#23876=CARTESIAN_POINT('Ctrl Pts',(3.44372941566734,1.90332245206109,55.7133393081712));
#23877=CARTESIAN_POINT('Ctrl Pts',(3.38609256410601,2.00407935992187,55.7192033103841));
#23878=CARTESIAN_POINT('Ctrl Pts',(3.32406383370634,2.10216284560579,55.7250673125969));
#23879=CARTESIAN_POINT('Ctrl Pts',(3.26029840193243,2.20299250589752,55.7310954971272));
#23880=CARTESIAN_POINT('Ctrl Pts',(3.1918916894103,2.30099641560372,55.7371236816575));
#23881=CARTESIAN_POINT('Ctrl Pts',(3.11913114405559,2.3957274273553,55.7431518661877));
#23882=CARTESIAN_POINT('Ctrl Pts',(3.04843196368654,2.48777463307257,55.749009267384));
#23883=CARTESIAN_POINT('Ctrl Pts',(2.97362260159842,2.57673155027685,55.7548666685803));
#23884=CARTESIAN_POINT('Ctrl Pts',(2.89501017746513,2.66221807378232,55.7607240697766));
#23885=CARTESIAN_POINT('Ctrl Pts',(2.81640910881105,2.7476922488524,55.7665806248776));
#23886=CARTESIAN_POINT('Ctrl Pts',(2.7340063496535,2.82969672350588,55.7724371799787));
#23887=CARTESIAN_POINT('Ctrl Pts',(2.6481478633288,2.9078861556029,55.7782937350797));
#23888=CARTESIAN_POINT('Ctrl Pts',(2.56228109456958,2.9860831303306,55.7841508551399));
#23889=CARTESIAN_POINT('Ctrl Pts',(2.47295824094942,3.06046405315319,55.7900079752));
#23890=CARTESIAN_POINT('Ctrl Pts',(2.38055998543373,3.13072246546252,55.7958650952602));
#23891=CARTESIAN_POINT('Ctrl Pts',(2.28343805027946,3.20457270133834,55.8020216490988));
#23892=CARTESIAN_POINT('Ctrl Pts',(2.18291834923423,3.2738674546978,55.8081782029373));
#23893=CARTESIAN_POINT('Ctrl Pts',(2.07947830021533,3.33830181363722,55.8143347567759));
#23894=CARTESIAN_POINT('Ctrl Pts',(1.98092260347625,3.39969363623825,55.8202006033105));
#23895=CARTESIAN_POINT('Ctrl Pts',(1.87971644562286,3.45667342848559,55.8260664498451));
#23896=CARTESIAN_POINT('Ctrl Pts',(1.77629770914611,3.50902485720495,55.8319322963796));
#23897=CARTESIAN_POINT('Ctrl Pts',(1.67280786463709,3.56141228140453,55.8378021761177));
#23898=CARTESIAN_POINT('Ctrl Pts',(1.56710278710126,3.60916483593996,55.8436720558557));
#23899=CARTESIAN_POINT('Ctrl Pts',(1.45963985147843,3.6521145250356,55.8495419355937));
#23900=CARTESIAN_POINT('Ctrl Pts',(1.35202453287753,3.69512511700434,55.8554201388504));
#23901=CARTESIAN_POINT('Ctrl Pts',(1.24264677007972,3.73331911858355,55.8612983421072));
#23902=CARTESIAN_POINT('Ctrl Pts',(1.1319785695324,3.76657848957371,55.8671765453639));
#23903=CARTESIAN_POINT('Ctrl Pts',(1.11586781001058,3.77142029349949,55.8680322773503));
#23904=CARTESIAN_POINT('Ctrl Pts',(1.09972971832541,3.77615760801281,55.8688880093368));
#23905=CARTESIAN_POINT('Ctrl Pts',(1.08356576507486,3.78079015984195,55.8697437413232));
#23906=CARTESIAN_POINT('Ctrl Pts',(0.972546323557523,3.81260807646786,55.8756211950469));
#23907=CARTESIAN_POINT('Ctrl Pts',(0.859942257719565,3.83958403344108,55.8814986487706));
#23908=CARTESIAN_POINT('Ctrl Pts',(0.746213444616676,3.86156114739535,55.8873761024944));
#23909=CARTESIAN_POINT('Ctrl Pts',(0.632629978708228,3.8835101742557,55.8932460447407));
#23910=CARTESIAN_POINT('Ctrl Pts',(0.517925025673935,3.900472985893,55.899115986987));
#23911=CARTESIAN_POINT('Ctrl Pts',(0.402573556405177,3.91234246094118,55.9049859292333));
#23912=CARTESIAN_POINT('Ctrl Pts',(0.287338815679251,3.92419992481573,55.9108499314616));
#23913=CARTESIAN_POINT('Ctrl Pts',(0.17145926806963,3.93097426257382,55.9167139336899));
#23914=CARTESIAN_POINT('Ctrl Pts',(0.0554193631486505,3.93260952729714,
55.9225779359182));
#23915=CARTESIAN_POINT('Ctrl Pts',(-0.0638694658513173,3.93429057670925,
55.9286061204427));
#23916=CARTESIAN_POINT('Ctrl Pts',(-0.183327329042966,3.9305404401863,55.9346343049672));
#23917=CARTESIAN_POINT('Ctrl Pts',(-0.302422667863923,3.92135557300815,
55.9406624894917));
#23918=CARTESIAN_POINT('Ctrl Pts',(-0.41814394001257,3.91243092049954,55.9465198907035));
#23919=CARTESIAN_POINT('Ctrl Pts',(-0.533522514949512,3.89837537764589,
55.9523772919152));
#23920=CARTESIAN_POINT('Ctrl Pts',(-0.648072238113552,3.87923850442152,
55.9582346931269));
#23921=CARTESIAN_POINT('Ctrl Pts',(-0.762605414694159,3.86010439549776,
55.9640912482434));
#23922=CARTESIAN_POINT('Ctrl Pts',(-0.876309570824094,3.83589048372245,
55.9699478033599));
#23923=CARTESIAN_POINT('Ctrl Pts',(-0.988706445761817,3.8066978556367,55.9758043584763));
#23924=CARTESIAN_POINT('Ctrl Pts',(-1.10111416318871,3.77750241145172,55.9816614785519));
#23925=CARTESIAN_POINT('Ctrl Pts',(-1.21221394946203,3.74332739991008,55.9875185986274));
#23926=CARTESIAN_POINT('Ctrl Pts',(-1.32154114196649,3.70432423123165,55.993375718703));
#23927=CARTESIAN_POINT('Ctrl Pts',(-1.43645747211256,3.66332710228396,55.9995322725199));
#23928=CARTESIAN_POINT('Ctrl Pts',(-1.54941469313502,3.61699526388156,56.0056888263368));
#23929=CARTESIAN_POINT('Ctrl Pts',(-1.65989658677665,3.56556199233827,56.0118453801538));
#23930=CARTESIAN_POINT('Ctrl Pts',(-1.76516161878899,3.51655735640159,56.0177112267035));
#23931=CARTESIAN_POINT('Ctrl Pts',(-1.86817940136615,3.46292229648925,56.0235770732532));
#23932=CARTESIAN_POINT('Ctrl Pts',(-1.96852950616077,3.40490537069307,56.0294429198029));
#23933=CARTESIAN_POINT('Ctrl Pts',(-2.06894860907477,3.34684855396921,56.035312799556));
#23934=CARTESIAN_POINT('Ctrl Pts',(-2.16669603517733,3.2844040935218,56.0411826793091));
#23935=CARTESIAN_POINT('Ctrl Pts',(-2.26138119176589,3.21786328260346,56.0470525590622));
#23936=CARTESIAN_POINT('Ctrl Pts',(-2.35620061237455,3.15122811648631,56.0529307623338));
#23937=CARTESIAN_POINT('Ctrl Pts',(-2.44794877365813,3.08048526014792,56.0588089656054));
#23938=CARTESIAN_POINT('Ctrl Pts',(-2.53626892964854,3.00596555477595,56.064687168877));
#23939=CARTESIAN_POINT('Ctrl Pts',(-2.54912632319468,2.99511719102291,56.0655429007533));
#23940=CARTESIAN_POINT('Ctrl Pts',(-2.56191113381532,2.98418884728861,56.0663986326297));
#23941=CARTESIAN_POINT('Ctrl Pts',(-2.57462232916952,2.97318160598067,56.0672543645061));
#23942=CARTESIAN_POINT('Ctrl Pts',(-2.66068396062302,2.89865666018549,56.0730481297119));
#23943=CARTESIAN_POINT('Ctrl Pts',(-2.74366779970919,2.82025249851762,56.0788418949177));
#23944=CARTESIAN_POINT('Ctrl Pts',(-2.82319664746214,2.73825668806973,56.0846356601235));
#23945=CARTESIAN_POINT('Ctrl Pts',(-2.90262312396697,2.65636642439754,56.0904219674697));
#23946=CARTESIAN_POINT('Ctrl Pts',(-2.97860315528158,2.57089400348787,56.096208274816));
#23947=CARTESIAN_POINT('Ctrl Pts',(-3.05079247440205,2.48216725426227,56.1019945821623));
#23948=CARTESIAN_POINT('Ctrl Pts',(-3.12290181329056,2.39353880747351,56.1077744787235));
#23949=CARTESIAN_POINT('Ctrl Pts',(-3.19122852740523,2.301663532516,56.1135543752848));
#23950=CARTESIAN_POINT('Ctrl Pts',(-3.2554657983641,2.20690539799096,56.1193342718461));
#23951=CARTESIAN_POINT('Ctrl Pts',(-3.31966367911436,2.11220536902725,56.1251106241825));
#23952=CARTESIAN_POINT('Ctrl Pts',(-3.37977686097575,2.01462634359139,56.1308869765189));
#23953=CARTESIAN_POINT('Ctrl Pts',(-3.43553970410726,1.91456416489567,56.1366633288554));
#23954=CARTESIAN_POINT('Ctrl Pts',(-3.49128270802699,1.81453758615581,56.1424376260907));
#23955=CARTESIAN_POINT('Ctrl Pts',(-3.54267824260044,1.71202998119307,56.1482119233261));
#23956=CARTESIAN_POINT('Ctrl Pts',(-3.58950526741073,1.60746413186443,56.1539862205615));
#23957=CARTESIAN_POINT('Ctrl Pts',(-3.6363276851416,1.50290857025266,56.1597599496923));
#23958=CARTESIAN_POINT('Ctrl Pts',(-3.67858231408159,1.39629555558776,56.1655336788232));
#23959=CARTESIAN_POINT('Ctrl Pts',(-3.71609552636559,1.28806950081343,56.171307407954));
#23960=CARTESIAN_POINT('Ctrl Pts',(-3.75363352304202,1.17977194277798,56.1770849516973));
#23961=CARTESIAN_POINT('Ctrl Pts',(-3.78642370412774,1.06985961776369,56.1828624954407));
#23962=CARTESIAN_POINT('Ctrl Pts',(-3.81434184516174,0.958793663020485,
56.188640039184));
#23963=CARTESIAN_POINT('Ctrl Pts',(-3.84226902337821,0.847691755908585,
56.1944194531349));
#23964=CARTESIAN_POINT('Ctrl Pts',(-3.86532093285606,0.735435891859941,
56.2001988670857));
#23965=CARTESIAN_POINT('Ctrl Pts',(-3.88342453340857,0.622497303866083,
56.2059782810366));
#23966=CARTESIAN_POINT('Ctrl Pts',(-3.90155186064883,0.509410697879598,
56.2117652695221));
#23967=CARTESIAN_POINT('Ctrl Pts',(-3.91471787359035,0.395640003337236,
56.2175522580076));
#23968=CARTESIAN_POINT('Ctrl Pts',(-3.92290144284473,0.281661622744134,
56.2233392464932));
#23969=CARTESIAN_POINT('Ctrl Pts',(-3.92970478800912,0.186906603222668,
56.2281502133104));
#23970=CARTESIAN_POINT('Ctrl Pts',(-3.93306556565048,0.0920082219184449,
56.2329611801277));
#23971=CARTESIAN_POINT('Ctrl Pts',(-3.93299903070378,-0.00276124668366241,
56.2377721469449));
#23972=CARTESIAN_POINT('',(-3.93299858145448,0.00334040074976491,57.4877721470256));
#23973=CARTESIAN_POINT('Ctrl Pts',(-3.93299903070322,-0.00276124747559212,
56.2377721469851));
#23974=CARTESIAN_POINT('Ctrl Pts',(-3.93287459502664,-0.180001932956672,
56.246769760553));
#23975=CARTESIAN_POINT('Ctrl Pts',(-3.92076827578561,-0.356823248188878,
56.2557673741209));
#23976=CARTESIAN_POINT('Ctrl Pts',(-3.89685364668713,-0.53199685741675,
56.2647649876888));
#23977=CARTESIAN_POINT('Ctrl Pts',(-3.88123204610195,-0.646424396524865,
56.2706424413929));
#23978=CARTESIAN_POINT('Ctrl Pts',(-3.86054048287139,-0.760350850911274,
56.2765198950971));
#23979=CARTESIAN_POINT('Ctrl Pts',(-3.83482071000186,-0.873292117301467,
56.2823973488012));
#23980=CARTESIAN_POINT('Ctrl Pts',(-3.80913380740383,-0.98608904298896,
56.2882672910277));
#23981=CARTESIAN_POINT('Ctrl Pts',(-3.7784315659522,-1.09790288606155,56.2941372332542));
#23982=CARTESIAN_POINT('Ctrl Pts',(-3.74280736362221,-1.20825578368798,
56.3000071754807));
#23983=CARTESIAN_POINT('Ctrl Pts',(-3.70721921078017,-1.31849701101181,
56.305871177689));
#23984=CARTESIAN_POINT('Ctrl Pts',(-3.66671913054122,-1.42727984335804,
56.3117351798972));
#23985=CARTESIAN_POINT('Ctrl Pts',(-3.62145115558799,-1.53413836654014,
56.3175991821055));
#23986=CARTESIAN_POINT('Ctrl Pts',(-3.57491575251127,-1.64398875091456,
56.3236273666374));
#23987=CARTESIAN_POINT('Ctrl Pts',(-3.52334161667332,-1.7518050444529,56.3296555511693));
#23988=CARTESIAN_POINT('Ctrl Pts',(-3.46693972427375,-1.85709933720648,
56.3356837357013));
#23989=CARTESIAN_POINT('Ctrl Pts',(-3.41213574307814,-1.95941055753205,
56.3415411368925));
#23990=CARTESIAN_POINT('Ctrl Pts',(-3.35277408902343,-2.05934037178854,
56.3473985380838));
#23991=CARTESIAN_POINT('Ctrl Pts',(-3.28909604162208,-2.15646382510489,
56.3532559392751));
#23992=CARTESIAN_POINT('Ctrl Pts',(-3.225427192447,-2.25357324904165,56.359112494371));
#23993=CARTESIAN_POINT('Ctrl Pts',(-3.15744341588601,-2.3478767732614,56.3649690494669));
#23994=CARTESIAN_POINT('Ctrl Pts',(-3.08542996722739,-2.43897743272365,
56.3708256045628));
#23995=CARTESIAN_POINT('Ctrl Pts',(-3.01340957171283,-2.53008688031048,
56.3766827246177));
#23996=CARTESIAN_POINT('Ctrl Pts',(-2.93735898716203,-2.61799252532131,
56.3825398446726));
#23997=CARTESIAN_POINT('Ctrl Pts',(-2.85760404489878,-2.70233012834816,
56.3883969647275));
#23998=CARTESIAN_POINT('Ctrl Pts',(-2.77377178742812,-2.79097932613792,
56.3945535185728));
#23999=CARTESIAN_POINT('Ctrl Pts',(-2.68584674290883,-2.87568564067674,
56.4007100724182));
#24000=CARTESIAN_POINT('Ctrl Pts',(-2.59425044351078,-2.95607064129804,
56.4068666262636));
#24001=CARTESIAN_POINT('Ctrl Pts',(-2.50697924465678,-3.03265992951386,
56.4127324727926));
#24002=CARTESIAN_POINT('Ctrl Pts',(-2.4163759413284,-3.10532645905232,56.4185983193216));
#24003=CARTESIAN_POINT('Ctrl Pts',(-2.32283744780661,-3.17378562462359,
56.4244641658506));
#24004=CARTESIAN_POINT('Ctrl Pts',(-2.22923463965204,-3.24229186093471,
56.430334045583));
#24005=CARTESIAN_POINT('Ctrl Pts',(-2.13269296506131,-3.30658474488133,
56.4362039253154));
#24006=CARTESIAN_POINT('Ctrl Pts',(-2.0336364255655,-3.36642419914859,56.4420738050477));
#24007=CARTESIAN_POINT('Ctrl Pts',(-1.93443942340472,-3.42634850605919,
56.4479520082987));
#24008=CARTESIAN_POINT('Ctrl Pts',(-1.83272080115182,-3.4818065858652,56.4538302115497));
#24009=CARTESIAN_POINT('Ctrl Pts',(-1.728927114159,-3.53260527570317,56.4597084148006));
#24010=CARTESIAN_POINT('Ctrl Pts',(-1.71381712594818,-3.54000040373856,
56.4605641468244));
#24011=CARTESIAN_POINT('Ctrl Pts',(-1.69866319141438,-3.54729687171511,
56.4614198788481));
#24012=CARTESIAN_POINT('Ctrl Pts',(-1.68346671721348,-3.55449417105085,
56.4622756108719));
#24013=CARTESIAN_POINT('Ctrl Pts',(-1.57909224872148,-3.60392763060304,
56.4681530646793));
#24014=CARTESIAN_POINT('Ctrl Pts',(-1.4723674951303,-3.64884093872592,56.4740305184866));
#24015=CARTESIAN_POINT('Ctrl Pts',(-1.36372073238838,-3.68900457631244,
56.479907972294));
#24016=CARTESIAN_POINT('Ctrl Pts',(-1.25521282189451,-3.72911688414713,
56.4857779146242));
#24017=CARTESIAN_POINT('Ctrl Pts',(-1.14478817082094,-3.76449145173836,
56.4916478569545));
#24018=CARTESIAN_POINT('Ctrl Pts',(-1.0328980336689,-3.79494540830866,56.4975177992847));
#24019=CARTESIAN_POINT('Ctrl Pts',(-0.921121122401242,-3.82536854736229,
56.5033818015971));
#24020=CARTESIAN_POINT('Ctrl Pts',(-0.807882070680306,-3.85088087245687,
56.5092458039095));
#24021=CARTESIAN_POINT('Ctrl Pts',(-0.69364980051294,-3.87134846716856,
56.5151098062218));
#24022=CARTESIAN_POINT('Ctrl Pts',(-0.576219219325438,-3.89238912003296,
56.5211379907149));
#24023=CARTESIAN_POINT('Ctrl Pts',(-0.457739395909401,-3.90809822122731,
56.5271661752079));
#24024=CARTESIAN_POINT('Ctrl Pts',(-0.338734249508409,-3.91838590598348,
56.5331943597009));
#24025=CARTESIAN_POINT('Ctrl Pts',(-0.223100612295275,-3.92838213255716,
56.5390517609966));
#24026=CARTESIAN_POINT('Ctrl Pts',(-0.106971456081406,-3.93325996686306,
56.5449091622923));
#24027=CARTESIAN_POINT('Ctrl Pts',(0.00916547212947215,-3.93298932036697,
56.550766563588));
#24028=CARTESIAN_POINT('Ctrl Pts',(0.125285624483332,-3.93271871296548,
56.5566231187882));
#24029=CARTESIAN_POINT('Ctrl Pts',(0.241413134207897,-3.92730110457721,
56.5624796739884));
#24030=CARTESIAN_POINT('Ctrl Pts',(0.357059671235795,-3.91675853112966,
56.5683362291887));
#24031=CARTESIAN_POINT('Ctrl Pts',(0.472717364229187,-3.90621494068162,
56.5741933493477));
#24032=CARTESIAN_POINT('Ctrl Pts',(0.587893581478536,-3.89054543983216,
56.5800504695067));
#24033=CARTESIAN_POINT('Ctrl Pts',(0.702105233804478,-3.86982392889707,
56.5859075896657));
#24034=CARTESIAN_POINT('Ctrl Pts',(0.822155728162672,-3.84804307220736,
56.5920641433648));
#24035=CARTESIAN_POINT('Ctrl Pts',(0.941139924894108,-3.8206800797011,56.5982206970638));
#24036=CARTESIAN_POINT('Ctrl Pts',(1.05851056277257,-3.78788125322044,56.6043772507629));
#24037=CARTESIAN_POINT('Ctrl Pts',(1.1703390620456,-3.7566311585669,56.6102430973946));
#24038=CARTESIAN_POINT('Ctrl Pts',(1.28070252045885,-3.72044703788001,56.6161089440264));
#24039=CARTESIAN_POINT('Ctrl Pts',(1.38914571081522,-3.67950583558766,56.6219747906581));
#24040=CARTESIAN_POINT('Ctrl Pts',(1.49766346387512,-3.63853648319461,56.6278446704926));
#24041=CARTESIAN_POINT('Ctrl Pts',(1.6042579417669,-3.59280369837456,56.6337145503272));
#24042=CARTESIAN_POINT('Ctrl Pts',(1.70849641291049,-3.54253144051989,56.6395844301617));
#24043=CARTESIAN_POINT('Ctrl Pts',(1.81288269469777,-3.49218789636649,56.6454626335136));
#24044=CARTESIAN_POINT('Ctrl Pts',(1.91490594185586,-3.43729222945618,56.6513408368654));
#24045=CARTESIAN_POINT('Ctrl Pts',(2.0141603940696,-3.37811292099026,56.6572190402173));
#24046=CARTESIAN_POINT('Ctrl Pts',(2.0286095606375,-3.36949777409936,56.6580747714964));
#24047=CARTESIAN_POINT('Ctrl Pts',(2.04300010392026,-3.36079191692025,56.6589305027755));
#24048=CARTESIAN_POINT('Ctrl Pts',(2.05733082942857,-3.35199624974174,56.6597862340546));
#24049=CARTESIAN_POINT('Ctrl Pts',(2.15575912719411,-3.29158461548147,56.6656636875792));
#24050=CARTESIAN_POINT('Ctrl Pts',(2.25168561722266,-3.22673490030129,56.6715411411037));
#24051=CARTESIAN_POINT('Ctrl Pts',(2.34468407574939,-3.1576804120948,56.6774185946283));
#24052=CARTESIAN_POINT('Ctrl Pts',(2.43756368079638,-3.08871417660072,56.6832885366756));
#24053=CARTESIAN_POINT('Ctrl Pts',(2.52752236816214,-3.01555409892089,56.6891584787229));
#24054=CARTESIAN_POINT('Ctrl Pts',(2.61416043040077,-2.93847821910029,56.6950284207702));
#24055=CARTESIAN_POINT('Ctrl Pts',(2.70071082028906,-2.86148033529396,56.7008924228));
#24056=CARTESIAN_POINT('Ctrl Pts',(2.78394696276826,-2.78057480411996,56.7067564248297));
#24057=CARTESIAN_POINT('Ctrl Pts',(2.86350049982774,-2.69608120936411,56.7126204268594));
#24058=CARTESIAN_POINT('Ctrl Pts',(2.94528140721404,-2.60922193065852,56.7186486114585));
#24059=CARTESIAN_POINT('Ctrl Pts',(3.02317008802361,-2.51857096006013,56.7246767960576));
#24060=CARTESIAN_POINT('Ctrl Pts',(3.09680503223868,-2.42451801236888,56.7307049806566));
#24061=CARTESIAN_POINT('Ctrl Pts',(3.16835383601571,-2.33312966447581,56.736562381672));
#24062=CARTESIAN_POINT('Ctrl Pts',(3.23588642041773,-2.23852985960576,56.7424197826874));
#24063=CARTESIAN_POINT('Ctrl Pts',(3.29911110420297,-2.14111067488922,56.7482771837027));
#24064=CARTESIAN_POINT('Ctrl Pts',(3.36232665526344,-2.0437055622494,56.754133738624));
#24065=CARTESIAN_POINT('Ctrl Pts',(3.42123531860403,-1.94348222553152,56.7599902935453));
#24066=CARTESIAN_POINT('Ctrl Pts',(3.47558875164533,-1.84086170839539,56.7658468484666));
#24067=CARTESIAN_POINT('Ctrl Pts',(3.52994742796367,-1.738231291833,56.7717039683483));
#24068=CARTESIAN_POINT('Ctrl Pts',(3.57974980736229,-1.63320359969469,56.7775610882301));
#24069=CARTESIAN_POINT('Ctrl Pts',(3.62479385001183,-1.52622362218527,56.7834182081118));
#24070=CARTESIAN_POINT('Ctrl Pts',(3.67214068442458,-1.41377449500485,56.7895747622056));
#24071=CARTESIAN_POINT('Ctrl Pts',(3.71422958870528,-1.29916865495173,56.7957313162994));
#24072=CARTESIAN_POINT('Ctrl Pts',(3.75088410301986,-1.1829443967122,56.8018878703932));
#24073=CARTESIAN_POINT('Ctrl Pts',(3.78580781945848,-1.07220815824482,56.8077537167543));
#24074=CARTESIAN_POINT('Ctrl Pts',(3.81579858269825,-0.960003272196668,
56.8136195631155));
#24075=CARTESIAN_POINT('Ctrl Pts',(3.84075588063964,-0.846807690879045,
56.8194854094766));
#24076=CARTESIAN_POINT('Ctrl Pts',(3.8657303385776,-0.733534279189309,56.8253552890429));
#24077=CARTESIAN_POINT('Ctrl Pts',(3.88566436910299,-0.619269221088189,
56.8312251686093));
#24078=CARTESIAN_POINT('Ctrl Pts',(3.90050912831131,-0.504497314125691,
56.8370950481756));
#24079=CARTESIAN_POINT('Ctrl Pts',(3.91537493747158,-0.389562659954418,
56.8429732512641));
#24080=CARTESIAN_POINT('Ctrl Pts',(3.92513704076069,-0.27412013200252,56.8488514543526));
#24081=CARTESIAN_POINT('Ctrl Pts',(3.92979861957694,-0.158656262312916,
56.8547296574411));
#24082=CARTESIAN_POINT('Ctrl Pts',(3.93047723989724,-0.141847337414223,
56.8555853907066));
#24083=CARTESIAN_POINT('Ctrl Pts',(3.93104785585078,-0.125037953337633,
56.8564411239721));
#24084=CARTESIAN_POINT('Ctrl Pts',(3.931510568873,-0.108229602419195,56.8572968572375));
#24085=CARTESIAN_POINT('Ctrl Pts',(3.93468863204792,0.00721560555963267,
56.8631743109679));
#24086=CARTESIAN_POINT('Ctrl Pts',(3.93278268651428,0.122990150236636,56.8690517646983));
#24087=CARTESIAN_POINT('Ctrl Pts',(3.92575527379227,0.238609577117339,56.8749292184287));
#24088=CARTESIAN_POINT('Ctrl Pts',(3.91873684221516,0.354081240536956,56.8807991606801));
#24089=CARTESIAN_POINT('Ctrl Pts',(3.90660998529077,0.46939777233163,56.8866691029314));
#24090=CARTESIAN_POINT('Ctrl Pts',(3.88938919745631,0.584072487547633,56.8925390451827));
#24091=CARTESIAN_POINT('Ctrl Pts',(3.87218583599748,0.69863115902154,56.8984030474144));
#24092=CARTESIAN_POINT('Ctrl Pts',(3.84989885818527,0.812548900263899,56.904267049646));
#24093=CARTESIAN_POINT('Ctrl Pts',(3.82259468146891,0.925342585859694,56.9101310518776));
#24094=CARTESIAN_POINT('Ctrl Pts',(3.79452603330295,1.04129430669781,56.9161592364003));
#24095=CARTESIAN_POINT('Ctrl Pts',(3.7611551099159,1.1560576545347,56.9221874209229));
#24096=CARTESIAN_POINT('Ctrl Pts',(3.72261080887317,1.2691169235577,56.9282156054455));
#24097=CARTESIAN_POINT('Ctrl Pts',(3.68515849885229,1.37897313263744,56.9340730066565));
#24098=CARTESIAN_POINT('Ctrl Pts',(3.64282214965559,1.487220106419,56.9399304078675));
#24099=CARTESIAN_POINT('Ctrl Pts',(3.59577078837762,1.59339933395558,56.9457878090785));
#24100=CARTESIAN_POINT('Ctrl Pts',(3.5487262236299,1.69956322399052,56.9516443641927));
#24101=CARTESIAN_POINT('Ctrl Pts',(3.49696816822327,1.80365958468784,56.9575009193069));
#24102=CARTESIAN_POINT('Ctrl Pts',(3.44071358844026,1.90525037785653,56.9633574744211));
#24103=CARTESIAN_POINT('Ctrl Pts',(3.38445358201128,2.00685097106765,56.9692145944929));
#24104=CARTESIAN_POINT('Ctrl Pts',(3.3236963887626,2.10594515538632,56.9750717145647));
#24105=CARTESIAN_POINT('Ctrl Pts',(3.25870432906919,2.20212059063659,56.9809288346365));
#24106=CARTESIAN_POINT('Ctrl Pts',(3.19038967815428,2.30321280585034,56.9870853884518));
#24107=CARTESIAN_POINT('Ctrl Pts',(3.11739598910982,2.4010795233256,56.9932419422672));
#24108=CARTESIAN_POINT('Ctrl Pts',(3.04007770569127,2.49527885082185,56.9993984960825));
#24109=CARTESIAN_POINT('Ctrl Pts',(2.96641032633423,2.58503016560828,57.0052643426248));
#24110=CARTESIAN_POINT('Ctrl Pts',(2.88881775321142,2.67145224474171,57.0111301891671));
#24111=CARTESIAN_POINT('Ctrl Pts',(2.80764538398454,2.75419977448809,57.0169960357093));
#24112=CARTESIAN_POINT('Ctrl Pts',(2.72641720276739,2.83700419926377,57.0228659154537));
#24113=CARTESIAN_POINT('Ctrl Pts',(2.64160462506545,2.9161287631432,57.0287357951981));
#24114=CARTESIAN_POINT('Ctrl Pts',(2.55358701072106,2.99126768756603,57.0346056749425));
#24115=CARTESIAN_POINT('Ctrl Pts',(2.46544458699009,3.06651315933323,57.0404838782037));
#24116=CARTESIAN_POINT('Ctrl Pts',(2.37408838188039,3.13776146185018,57.0463620814648));
#24117=CARTESIAN_POINT('Ctrl Pts',(2.27992763197877,3.20474944308282,57.052240284726));
#24118=CARTESIAN_POINT('Ctrl Pts',(2.26621998124525,3.21450136042672,57.0530960166241));
#24119=CARTESIAN_POINT('Ctrl Pts',(2.25245293796707,3.22416306909368,57.0539517485223));
#24120=CARTESIAN_POINT('Ctrl Pts',(2.23862780747392,3.23373383870789,57.0548074804205));
#24121=CARTESIAN_POINT('Ctrl Pts',(2.14367216270103,3.29946910248276,57.0606849348273));
#24122=CARTESIAN_POINT('Ctrl Pts',(2.04566303290193,3.36112614987088,57.0665623892341));
#24123=CARTESIAN_POINT('Ctrl Pts',(1.94498571113632,3.41840892572488,57.0724398436409));
#24124=CARTESIAN_POINT('Ctrl Pts',(1.84443705649401,3.4756184933344,57.078309786573));
#24125=CARTESIAN_POINT('Ctrl Pts',(1.74122734686845,3.52846470513796,57.0841797295052));
#24126=CARTESIAN_POINT('Ctrl Pts',(1.63577212790531,3.57669380092399,57.0900496724373));
#24127=CARTESIAN_POINT('Ctrl Pts',(1.53042362304631,3.62487409187323,57.0959136753534));
#24128=CARTESIAN_POINT('Ctrl Pts',(1.42283450183459,3.6684463900876,57.1017776782694));
#24129=CARTESIAN_POINT('Ctrl Pts',(1.31344569670922,3.70720236860574,57.1076416811854));
#24130=CARTESIAN_POINT('Ctrl Pts',(1.20099420520583,3.74704344360462,57.1136698654528));
#24131=CARTESIAN_POINT('Ctrl Pts',(1.08664114851458,3.78179429297267,57.1196980497202));
#24132=CARTESIAN_POINT('Ctrl Pts',(0.970888882770561,3.81128112021568,57.1257262339876));
#24133=CARTESIAN_POINT('Ctrl Pts',(0.858415953743547,3.83993256653009,57.1315836358874));
#24134=CARTESIAN_POINT('Ctrl Pts',(0.744622458318199,3.86361414435249,57.1374410377871));
#24135=CARTESIAN_POINT('Ctrl Pts',(0.629984773635399,3.88221691627188,57.1432984396869));
#24136=CARTESIAN_POINT('Ctrl Pts',(0.515363648261151,3.9008170010379,57.1491549954903));
#24137=CARTESIAN_POINT('Ctrl Pts',(0.399898983185378,3.91433967268589,57.1550115512937));
#24138=CARTESIAN_POINT('Ctrl Pts',(0.284076199998829,3.92272733090056,57.1608681070971));
#24139=CARTESIAN_POINT('Ctrl Pts',(0.168242243876824,3.93111579823724,57.1667252278578));
#24140=CARTESIAN_POINT('Ctrl Pts',(0.0520505124086948,3.93436823762812,
57.1725823486184));
#24141=CARTESIAN_POINT('Ctrl Pts',(-0.0640103171830569,3.9324790755062,
57.1784394693791));
#24142=CARTESIAN_POINT('Ctrl Pts',(-0.186004494975884,3.93049333423077,
57.1845960222311));
#24143=CARTESIAN_POINT('Ctrl Pts',(-0.307853524419974,3.9228263832232,57.1907525750831));
#24144=CARTESIAN_POINT('Ctrl Pts',(-0.428993645620601,3.90953366170662,
57.1969091279351));
#24145=CARTESIAN_POINT('Ctrl Pts',(-0.544413664051061,3.89686860782332,
57.202774975159));
#24146=CARTESIAN_POINT('Ctrl Pts',(-0.65918978509334,3.87909705182298,57.2086408223829));
#24147=CARTESIAN_POINT('Ctrl Pts',(-0.772844080756706,3.85631962197629,
57.2145066696068));
#24148=CARTESIAN_POINT('Ctrl Pts',(-0.886576522071217,3.83352653097859,
57.2203765500302));
#24149=CARTESIAN_POINT('Ctrl Pts',(-0.999185202731103,3.80572081111499,
57.2262464304536));
#24150=CARTESIAN_POINT('Ctrl Pts',(-1.11020675248651,3.77305313595414,57.232116310877));
#24151=CARTESIAN_POINT('Ctrl Pts',(-1.22138573115095,3.74033913792649,57.2379945148095));
#24152=CARTESIAN_POINT('Ctrl Pts',(-1.33097269973614,3.70274956109741,57.2438727187419));
#24153=CARTESIAN_POINT('Ctrl Pts',(-1.43852366699403,3.66048339150693,57.2497509226744));
#24154=CARTESIAN_POINT('Ctrl Pts',(-1.45418053515729,3.65433044038137,57.2506066496507));
#24155=CARTESIAN_POINT('Ctrl Pts',(-1.4697942979821,3.6480784602632,57.2514623766269));
#24156=CARTESIAN_POINT('Ctrl Pts',(-1.48536363059346,3.64172814538788,57.2523181036032));
#24157=CARTESIAN_POINT('Ctrl Pts',(-1.59229961531961,3.59811181375283,57.2581955557168));
#24158=CARTESIAN_POINT('Ctrl Pts',(-1.69748813306968,3.54970988500913,57.2640730078305));
#24159=CARTESIAN_POINT('Ctrl Pts',(-1.8004707162327,3.49668331422629,57.2699504599441));
#24160=CARTESIAN_POINT('Ctrl Pts',(-1.90332168602245,3.44372451224123,57.2758204005808));
#24161=CARTESIAN_POINT('Ctrl Pts',(-2.00397196448123,3.38615300965328,57.2816903412176));
#24162=CARTESIAN_POINT('Ctrl Pts',(-2.10198197991541,3.32417820763432,57.2875602818543));
#24163=CARTESIAN_POINT('Ctrl Pts',(-2.19989281529583,3.26226612026926,57.2934242824753));
#24164=CARTESIAN_POINT('Ctrl Pts',(-2.29516835563841,3.19595981612733,57.2992882830963));
#24165=CARTESIAN_POINT('Ctrl Pts',(-2.38739321211389,3.12551478172038,57.3051522837174));
#24166=CARTESIAN_POINT('Ctrl Pts',(-2.48220024644996,3.05309737657536,57.3111804688452));
#24167=CARTESIAN_POINT('Ctrl Pts',(-2.57378284453499,2.97630625682685,57.3172086539731));
#24168=CARTESIAN_POINT('Ctrl Pts',(-2.66172097930895,2.89546722107274,57.323236839101));
#24169=CARTESIAN_POINT('Ctrl Pts',(-2.7471677242768,2.81691844937905,57.3290942387213));
#24170=CARTESIAN_POINT('Ctrl Pts',(-2.82917341376195,2.73454834430281,57.3349516383417));
#24171=CARTESIAN_POINT('Ctrl Pts',(-2.90738653816944,2.64869638080154,57.340809037962));
#24172=CARTESIAN_POINT('Ctrl Pts',(-2.98558836488799,2.5628568184003,57.3466655914958));
#24173=CARTESIAN_POINT('Ctrl Pts',(-3.05999843816813,2.47353670255036,57.3525221450295));
#24174=CARTESIAN_POINT('Ctrl Pts',(-3.130303304737,2.38111113145789,57.3583786985632));
#24175=CARTESIAN_POINT('Ctrl Pts',(-3.20061495346844,2.28867664426503,57.3642358170664));
#24176=CARTESIAN_POINT('Ctrl Pts',(-3.26682035849011,2.1931364346237,57.3700929355695));
#24177=CARTESIAN_POINT('Ctrl Pts',(-3.32864786319633,2.09489675230991,57.3759500540726));
#24178=CARTESIAN_POINT('Ctrl Pts',(-3.39363621856898,1.99163469416537,57.3821066101321));
#24179=CARTESIAN_POINT('Ctrl Pts',(-3.45378692888341,1.88539027559086,57.3882631661915));
#24180=CARTESIAN_POINT('Ctrl Pts',(-3.50883841719906,1.77666596803903,57.394419722251));
#24181=CARTESIAN_POINT('Ctrl Pts',(-3.56129038796504,1.67307559517643,57.4002855672686));
#24182=CARTESIAN_POINT('Ctrl Pts',(-3.60911358120336,1.56723458939839,57.4061514122863));
#24183=CARTESIAN_POINT('Ctrl Pts',(-3.65213116331708,1.45959822071976,57.4120172573039));
#24184=CARTESIAN_POINT('Ctrl Pts',(-3.69517832331094,1.3518878437995,57.417887135539));
#24185=CARTESIAN_POINT('Ctrl Pts',(-3.73341315710086,1.24238003427091,57.423757013774));
#24186=CARTESIAN_POINT('Ctrl Pts',(-3.76670870051357,1.13154521141467,57.4296268920091));
#24187=CARTESIAN_POINT('Ctrl Pts',(-3.80005145734785,1.02055322364445,57.4355050937916));
#24188=CARTESIAN_POINT('Ctrl Pts',(-3.82844084754621,0.908230865923159,
57.441383295574));
#24189=CARTESIAN_POINT('Ctrl Pts',(-3.85180095910932,0.795058721985113,
57.4472614973565));
#24190=CARTESIAN_POINT('Ctrl Pts',(-3.85520170240365,0.778583226627879,
57.4481172404998));
#24191=CARTESIAN_POINT('Ctrl Pts',(-3.85849594864675,0.762089729330191,
57.448972983643));
#24192=CARTESIAN_POINT('Ctrl Pts',(-3.8616835554484,0.745579719131035,57.4498287267862));
#24193=CARTESIAN_POINT('Ctrl Pts',(-3.89349633805213,0.580807399979073,
57.4583691686516));
#24194=CARTESIAN_POINT('Ctrl Pts',(-3.91477062463092,0.4139403465271,57.466909610517));
#24195=CARTESIAN_POINT('Ctrl Pts',(-3.92529386198954,0.246083516366632,
57.4754500523825));
#24196=CARTESIAN_POINT('Ctrl Pts',(-3.93035481505268,0.165355931326066,
57.47955741725));
#24197=CARTESIAN_POINT('Ctrl Pts',(-3.93292973557021,0.0843997468008381,
57.4836647821176));
#24198=CARTESIAN_POINT('Ctrl Pts',(-3.9329985814538,0.0033404015496607,
57.4877721469851));
#24199=CARTESIAN_POINT('',(-3.93299997598709,-0.000434609756366564,58.7377721470271));
#24200=CARTESIAN_POINT('Ctrl Pts',(-3.93299858145448,0.00334040074973609,
57.4877721470256));
#24201=CARTESIAN_POINT('Ctrl Pts',(-3.93309550525033,-0.110777988079204,
57.4935546494572));
#24202=CARTESIAN_POINT('Ctrl Pts',(-3.92822141577198,-0.225058967539185,
57.4993371518887));
#24203=CARTESIAN_POINT('Ctrl Pts',(-3.91836055661331,-0.339027356384526,
57.5051196543202));
#24204=CARTESIAN_POINT('Ctrl Pts',(-3.90825529794007,-0.455820430022834,
57.5110454749722));
#24205=CARTESIAN_POINT('Ctrl Pts',(-3.89291276328519,-0.572284765183148,
57.5169712956243));
#24206=CARTESIAN_POINT('Ctrl Pts',(-3.87237285095124,-0.687908063054844,
57.5228971162763));
#24207=CARTESIAN_POINT('Ctrl Pts',(-3.85235870955178,-0.800571690584067,
57.5286712505817));
#24208=CARTESIAN_POINT('Ctrl Pts',(-3.82741013327092,-0.912436371183917,
57.5344453848871));
#24209=CARTESIAN_POINT('Ctrl Pts',(-3.79761646195819,-1.02303382537638,
57.5402195191925));
#24210=CARTESIAN_POINT('Ctrl Pts',(-3.76783009514474,-1.1336041644471,57.5459922378563));
#24211=CARTESIAN_POINT('Ctrl Pts',(-3.73320110443993,-1.24290748371754,
57.5517649565202));
#24212=CARTESIAN_POINT('Ctrl Pts',(-3.69386947882092,-1.35048779092421,
57.557537675184));
#24213=CARTESIAN_POINT('Ctrl Pts',(-3.65453736283475,-1.45806943938867,
57.5633104658192));
#24214=CARTESIAN_POINT('Ctrl Pts',(-3.61050264242728,-1.56392763358175,
57.5690832564544));
#24215=CARTESIAN_POINT('Ctrl Pts',(-3.56195420950007,-1.66762442097279,
57.5748560470896));
#24216=CARTESIAN_POINT('Ctrl Pts',(-3.51115626516457,-1.77612604123223,
57.5808963223296));
#24217=CARTESIAN_POINT('Ctrl Pts',(-3.45541646261234,-1.88226066750435,
57.5869365975695));
#24218=CARTESIAN_POINT('Ctrl Pts',(-3.39500539199336,-1.98555468026849,
57.5929768728094));
#24219=CARTESIAN_POINT('Ctrl Pts',(-3.33719109215317,-2.084408598341,57.5987575067274));
#24220=CARTESIAN_POINT('Ctrl Pts',(-3.27509907872395,-2.18066071817606,
57.6045381406453));
#24221=CARTESIAN_POINT('Ctrl Pts',(-3.20901054362121,-2.27392619293767,
57.6103187745633));
#24222=CARTESIAN_POINT('Ctrl Pts',(-3.14287855809915,-2.36725298580807,
57.6161032090037));
#24223=CARTESIAN_POINT('Ctrl Pts',(-3.07274508360941,-2.45758889200227,
57.6218876434442));
#24224=CARTESIAN_POINT('Ctrl Pts',(-2.99893087505149,-2.54458299268524,
57.6276720778847));
#24225=CARTESIAN_POINT('Ctrl Pts',(-2.92501327916339,-2.63169894101769,
57.6334646142509));
#24226=CARTESIAN_POINT('Ctrl Pts',(-2.84740495560434,-2.71546343896211,
57.6392571506171));
#24227=CARTESIAN_POINT('Ctrl Pts',(-2.7664625042894,-2.79556330859469,57.6450496869833));
#24228=CARTESIAN_POINT('Ctrl Pts',(-2.75579757715864,-2.80611721768611,
57.6458129079785));
#24229=CARTESIAN_POINT('Ctrl Pts',(-2.74507481257095,-2.81660756592347,
57.6465761289737));
#24230=CARTESIAN_POINT('Ctrl Pts',(-2.73429506597381,-2.82703369137888,
57.6473393499689));
#24231=CARTESIAN_POINT('Ctrl Pts',(-2.65128173977405,-2.90732383044949,
57.653216808485));
#24232=CARTESIAN_POINT('Ctrl Pts',(-2.56459287448662,-2.98408606550775,
57.659094267001));
#24233=CARTESIAN_POINT('Ctrl Pts',(-2.47456054136355,-3.05696567320056,
57.6649717255171));
#24234=CARTESIAN_POINT('Ctrl Pts',(-2.38464327049678,-3.12975213999823,
57.6708416725801));
#24235=CARTESIAN_POINT('Ctrl Pts',(-2.29139134749635,-3.1986655904819,57.6767116196432));
#24236=CARTESIAN_POINT('Ctrl Pts',(-2.19517356620747,-3.26338811884581,
57.6825815667062));
#24237=CARTESIAN_POINT('Ctrl Pts',(-2.09905315097321,-3.32804515227577,
57.6884455737697));
#24238=CARTESIAN_POINT('Ctrl Pts',(-1.99997318774395,-3.38851947061545,
57.6943095808331));
#24239=CARTESIAN_POINT('Ctrl Pts',(-1.89833490173518,-3.44453387279819,
57.7001735878965));
#24240=CARTESIAN_POINT('Ctrl Pts',(-1.79385103043734,-3.50211652022676,
57.7062017706155));
#24241=CARTESIAN_POINT('Ctrl Pts',(-1.68666381001068,-3.55498554751881,
57.7122299533345));
#24242=CARTESIAN_POINT('Ctrl Pts',(-1.57724068230134,-3.60288784589441,
57.7182581360534));
#24243=CARTESIAN_POINT('Ctrl Pts',(-1.4709174798734,-3.64943308613357,57.7241155421148));
#24244=CARTESIAN_POINT('Ctrl Pts',(-1.36248375739337,-3.69128905536023,
57.7299729481762));
#24245=CARTESIAN_POINT('Ctrl Pts',(-1.25239186243257,-3.72827086233185,
57.7358303542376));
#24246=CARTESIAN_POINT('Ctrl Pts',(-1.14231587017115,-3.7652473273066,57.7416869142007));
#24247=CARTESIAN_POINT('Ctrl Pts',(-1.03058257265253,-3.79735089876927,
57.7475434741638));
#24248=CARTESIAN_POINT('Ctrl Pts',(-0.917661582905724,-3.8244458708758,
57.7534000341269));
#24249=CARTESIAN_POINT('Ctrl Pts',(-0.804729700281146,-3.8515434566879,
57.7592571590406));
#24250=CARTESIAN_POINT('Ctrl Pts',(-0.690610298803393,-3.87363138643092,
57.7651142839544));
#24251=CARTESIAN_POINT('Ctrl Pts',(-0.57578465712533,-3.89062476070606,
57.7709714088682));
#24252=CARTESIAN_POINT('Ctrl Pts',(-0.455089013286741,-3.90848685334629,
57.7771279558918));
#24253=CARTESIAN_POINT('Ctrl Pts',(-0.333613513951472,-3.92071965581202,
57.7832845029155));
#24254=CARTESIAN_POINT('Ctrl Pts',(-0.211923433336705,-3.92728627151151,
57.7894410499391));
#24255=CARTESIAN_POINT('Ctrl Pts',(-0.0959792332007362,-3.93354282916215,
57.7953069012612));
#24256=CARTESIAN_POINT('Ctrl Pts',(0.0201593256405265,-3.93465611332302,
57.8011727525832));
#24257=CARTESIAN_POINT('Ctrl Pts',(0.136004315335366,-3.93064776165585,
57.8070386039053));
#24258=CARTESIAN_POINT('Ctrl Pts',(0.251928956505384,-3.92663665396856,
57.8129084884075));
#24259=CARTESIAN_POINT('Ctrl Pts',(0.367559216520916,-3.91749693078149,
57.8187783729097));
#24260=CARTESIAN_POINT('Ctrl Pts',(0.482413400481056,-3.90330197538396,
57.8246482574119));
#24261=CARTESIAN_POINT('Ctrl Pts',(0.597430446905614,-3.88908689163464,
57.830526465371));
#24262=CARTESIAN_POINT('Ctrl Pts',(0.711668816482015,-3.86980234051534,
57.8364046733302));
#24263=CARTESIAN_POINT('Ctrl Pts',(0.82465808600255,-3.84557252450017,57.8422828812893));
#24264=CARTESIAN_POINT('Ctrl Pts',(0.841106059963436,-3.84204536316365,
57.8431385785768));
#24265=CARTESIAN_POINT('Ctrl Pts',(0.857527593346193,-3.83841349227568,
57.8439942758644));
#24266=CARTESIAN_POINT('Ctrl Pts',(0.873921266230486,-3.8346773815316,57.8448499731519));
#24267=CARTESIAN_POINT('Ctrl Pts',(0.986522809923481,-3.80901553990768,
57.8507274135638));
#24268=CARTESIAN_POINT('Ctrl Pts',(1.09817767466564,-3.77834778367696,57.8566048539757));
#24269=CARTESIAN_POINT('Ctrl Pts',(1.20840733454266,-3.7427584364775,57.8624822943876));
#24270=CARTESIAN_POINT('Ctrl Pts',(1.31849611878142,-3.7072145731524,57.8683522233169));
#24271=CARTESIAN_POINT('Ctrl Pts',(1.42716293148851,-3.66676175352668,57.8742221522463));
#24272=CARTESIAN_POINT('Ctrl Pts',(1.53394001998351,-3.62153517380309,57.8800920811756));
#24273=CARTESIAN_POINT('Ctrl Pts',(1.64060905662699,-3.57635436059875,57.8859560700976));
#24274=CARTESIAN_POINT('Ctrl Pts',(1.74539179526742,-3.52640955642787,57.8918200590196));
#24275=CARTESIAN_POINT('Ctrl Pts',(1.84783685675272,-3.47188535968949,57.8976840479416));
#24276=CARTESIAN_POINT('Ctrl Pts',(1.95315053552432,-3.41583440264642,57.903712237458));
#24277=CARTESIAN_POINT('Ctrl Pts',(2.05599326083579,-3.3549439344886,57.9097404269743));
#24278=CARTESIAN_POINT('Ctrl Pts',(2.15589764895159,-3.28946717984006,57.9157686164907));
#24279=CARTESIAN_POINT('Ctrl Pts',(2.25297136636655,-3.22584563029778,57.9216260045061));
#24280=CARTESIAN_POINT('Ctrl Pts',(2.3472706518138,-3.15789443962736,57.9274833925216));
#24281=CARTESIAN_POINT('Ctrl Pts',(2.43839351015087,-3.08589145785364,57.933340780537));
#24282=CARTESIAN_POINT('Ctrl Pts',(2.52950320684809,-3.01389887607539,57.9391973225206));
#24283=CARTESIAN_POINT('Ctrl Pts',(2.61743706519509,-2.93785592262794,57.9450538645043));
#24284=CARTESIAN_POINT('Ctrl Pts',(2.70182485264192,-2.85808178078347,57.9509104064879));
#24285=CARTESIAN_POINT('Ctrl Pts',(2.78622078178691,-2.77829994236343,57.9567675135083));
#24286=CARTESIAN_POINT('Ctrl Pts',(2.86706966014709,-2.69478648331711,57.9626246205287));
#24287=CARTESIAN_POINT('Ctrl Pts',(2.94403743498049,-2.60789811561599,57.968481727549));
#24288=CARTESIAN_POINT('Ctrl Pts',(3.02494046039717,-2.51656727182126,57.9746382999478));
#24289=CARTESIAN_POINT('Ctrl Pts',(3.10155467196922,-2.42150765840215,57.9807948723466));
#24290=CARTESIAN_POINT('Ctrl Pts',(3.17354032432473,-2.32317257427958,57.9869514447454));
#24291=CARTESIAN_POINT('Ctrl Pts',(3.24212651904858,-2.22948127598435,57.9928172785548));
#24292=CARTESIAN_POINT('Ctrl Pts',(3.30651113921793,-2.13281718287333,57.9986831123642));
#24293=CARTESIAN_POINT('Ctrl Pts',(3.36644573060327,-2.03360078257827,58.0045489461735));
#24294=CARTESIAN_POINT('Ctrl Pts',(3.42642153266298,-1.93431616166687,58.0104188132959));
#24295=CARTESIAN_POINT('Ctrl Pts',(3.48194101623978,-1.83247610023236,58.0162886804183));
#24296=CARTESIAN_POINT('Ctrl Pts',(3.53280247247931,-1.72852413649448,58.0221585475406));
#24297=CARTESIAN_POINT('Ctrl Pts',(3.58373605267083,-1.62442476395245,58.0280367384124));
#24298=CARTESIAN_POINT('Ctrl Pts',(3.62999826139828,-1.51820788985982,58.0339149292841));
#24299=CARTESIAN_POINT('Ctrl Pts',(3.67143611213218,-1.41033537661496,58.0397931201558));
#24300=CARTESIAN_POINT('Ctrl Pts',(3.6774691868759,-1.3946298580209,58.0406489455488));
#24301=CARTESIAN_POINT('Ctrl Pts',(3.68340008502672,-1.37888926644417,58.0415047709417));
#24302=CARTESIAN_POINT('Ctrl Pts',(3.68922842404239,-1.36311504842313,58.0423605963347));
#24303=CARTESIAN_POINT('Ctrl Pts',(3.72925510536922,-1.25478408205178,58.0482380599109));
#24304=CARTESIAN_POINT('Ctrl Pts',(3.76457179281869,-1.14451102670765,58.0541155234872));
#24305=CARTESIAN_POINT('Ctrl Pts',(3.79498766993197,-1.03274274873477,58.0599929870635));
#24306=CARTESIAN_POINT('Ctrl Pts',(3.82536467469992,-0.921117313760708,
58.0658629390762));
#24307=CARTESIAN_POINT('Ctrl Pts',(3.85085321809989,-0.808000851035608,
58.0717328910889));
#24308=CARTESIAN_POINT('Ctrl Pts',(3.87131097836753,-0.69385899775889,58.0776028431016));
#24309=CARTESIAN_POINT('Ctrl Pts',(3.89174803634702,-0.579832650652215,
58.0834668549999));
#24310=CARTESIAN_POINT('Ctrl Pts',(3.90716436552608,-0.464783380736541,
58.0893308668981));
#24311=CARTESIAN_POINT('Ctrl Pts',(3.91746796700674,-0.349190102202228,
58.0951948787963));
#24312=CARTESIAN_POINT('Ctrl Pts',(3.92806002826915,-0.230360672506577,
58.1012230596597));
#24313=CARTESIAN_POINT('Ctrl Pts',(3.93324873810663,-0.110956751342765,
58.1072512405231));
#24314=CARTESIAN_POINT('Ctrl Pts',(3.93299083247968,0.00849185673065156,
58.1132794213865));
#24315=CARTESIAN_POINT('Ctrl Pts',(3.93274023297324,0.124556645937995,58.1191368319708));
#24316=CARTESIAN_POINT('Ctrl Pts',(3.92734746710776,0.240663184613262,58.1249942425552));
#24317=CARTESIAN_POINT('Ctrl Pts',(3.91682562021546,0.356322972629773,58.1308516531395));
#24318=CARTESIAN_POINT('Ctrl Pts',(3.90630529341633,0.471966051255202,58.1367082175026));
#24319=CARTESIAN_POINT('Ctrl Pts',(3.89065739645109,0.587162096868206,58.1425647818658));
#24320=CARTESIAN_POINT('Ctrl Pts',(3.86994698709251,0.701426629871944,58.1484213462289));
#24321=CARTESIAN_POINT('Ctrl Pts',(3.84923458036361,0.81570218286964,58.1542784754156));
#24322=CARTESIAN_POINT('Ctrl Pts',(3.82345876422852,0.929045638766885,58.1601356046023));
#24323=CARTESIAN_POINT('Ctrl Pts',(3.79273579573425,1.04098231673549,58.1659927337891));
#24324=CARTESIAN_POINT('Ctrl Pts',(3.76044229612203,1.15864109919484,58.1721492742664));
#24325=CARTESIAN_POINT('Ctrl Pts',(3.72268260755957,1.27474498151757,58.1783058147438));
#24326=CARTESIAN_POINT('Ctrl Pts',(3.67965076860994,1.3887617582106,58.1844623552212));
#24327=CARTESIAN_POINT('Ctrl Pts',(3.63865070715375,1.49739515537782,58.1903282104598));
#24328=CARTESIAN_POINT('Ctrl Pts',(3.59286519680946,1.60413366828352,58.1961940656984));
#24329=CARTESIAN_POINT('Ctrl Pts',(3.54251067677579,1.7085394654293,58.202059920937));
#24330=CARTESIAN_POINT('Ctrl Pts',(3.49212153558816,1.81301704658127,58.2079298092332));
#24331=CARTESIAN_POINT('Ctrl Pts',(3.43715732435433,1.91515835608604,58.2137996975294));
#24332=CARTESIAN_POINT('Ctrl Pts',(3.3778793279353,2.01455212042461,58.2196695858256));
#24333=CARTESIAN_POINT('Ctrl Pts',(3.31851727774101,2.11408682105717,58.2255477973833));
#24334=CARTESIAN_POINT('Ctrl Pts',(3.25482946277169,2.21086585963588,58.2314260089411));
#24335=CARTESIAN_POINT('Ctrl Pts',(3.18711913504503,2.30450875872272,58.2373042204989));
#24336=CARTESIAN_POINT('Ctrl Pts',(3.1772628296522,2.31813995860402,58.2381598868385));
#24337=CARTESIAN_POINT('Ctrl Pts',(3.16732135603069,2.3317047665503,58.239015553178));
#24338=CARTESIAN_POINT('Ctrl Pts',(3.15729571616681,2.34520207246084,58.2398712195176));
#24339=CARTESIAN_POINT('Ctrl Pts',(3.08843061494,2.43791369490481,58.2457487046349));
#24340=CARTESIAN_POINT('Ctrl Pts',(3.01536557255422,2.52774145148418,58.2516261897521));
#24341=CARTESIAN_POINT('Ctrl Pts',(2.93837061745917,2.61428137629684,58.2575036748694));
#24342=CARTESIAN_POINT('Ctrl Pts',(2.86147405986521,2.70071070539146,58.2633736487173));
#24343=CARTESIAN_POINT('Ctrl Pts',(2.78065784949517,2.78386025355741,58.2692436225652));
#24344=CARTESIAN_POINT('Ctrl Pts',(2.69623423127772,2.8633564168797,58.2751135964131));
#24345=CARTESIAN_POINT('Ctrl Pts',(2.61189604166093,2.94277213771287,58.2809776304107));
#24346=CARTESIAN_POINT('Ctrl Pts',(2.52395800393851,3.01854154625617,58.2868416644083));
#24347=CARTESIAN_POINT('Ctrl Pts',(2.4327709769061,3.0903259332833,58.2927056984059));
#24348=CARTESIAN_POINT('Ctrl Pts',(2.33903155703685,3.16411961879518,58.2987338710849));
#24349=CARTESIAN_POINT('Ctrl Pts',(2.24185886899489,3.23370156412764,58.3047620437638));
#24350=CARTESIAN_POINT('Ctrl Pts',(2.14167301494458,3.29874607950629,58.3107902164427));
#24351=CARTESIAN_POINT('Ctrl Pts',(2.04432478387846,3.36194830074489,58.3166476496344));
#24352=CARTESIAN_POINT('Ctrl Pts',(1.94413215200164,3.42086643555492,58.3225050828262));
#24353=CARTESIAN_POINT('Ctrl Pts',(1.84151141899156,3.4752445516429,58.3283625160179));
#24354=CARTESIAN_POINT('Ctrl Pts',(1.73890550896687,3.52961481311908,58.3342191031365));
#24355=CARTESIAN_POINT('Ctrl Pts',(1.63387255962941,3.57944616682173,58.340075690255));
#24356=CARTESIAN_POINT('Ctrl Pts',(1.52685389817576,3.62452840706559,58.3459322773736));
#24357=CARTESIAN_POINT('Ctrl Pts',(1.41982491334592,3.66961499609237,58.3517894294381));
#24358=CARTESIAN_POINT('Ctrl Pts',(1.31081021577677,3.70995140082501,58.3576465815025));
#24359=CARTESIAN_POINT('Ctrl Pts',(1.20027089819499,3.74537565151296,58.363503733567));
#24360=CARTESIAN_POINT('Ctrl Pts',(1.08408195406364,3.78261042348478,58.3696602426614));
#24361=CARTESIAN_POINT('Ctrl Pts',(0.966208905409569,3.8144174858749,58.3758167517559));
#24362=CARTESIAN_POINT('Ctrl Pts',(0.847203506495735,3.840668590048,58.3819732608503));
#24363=CARTESIAN_POINT('Ctrl Pts',(0.733816006300927,3.86568045595248,58.3878391390585));
#24364=CARTESIAN_POINT('Ctrl Pts',(0.619401048536494,3.88564892764175,58.3937050172667));
#24365=CARTESIAN_POINT('Ctrl Pts',(0.504443596768991,3.9005160758134,58.3995708954749));
#24366=CARTESIAN_POINT('Ctrl Pts',(0.389407105984118,3.91539344589554,58.4054408067688));
#24367=CARTESIAN_POINT('Ctrl Pts',(0.273827788375325,3.92516247373269,58.4113107180626));
#24368=CARTESIAN_POINT('Ctrl Pts',(0.158192865142057,3.92981730076834,58.4171806293565));
#24369=CARTESIAN_POINT('Ctrl Pts',(0.0423939789340578,3.93447872805299,
58.4230588638116));
#24370=CARTESIAN_POINT('Ctrl Pts',(-0.0734602595775473,3.93401148640706,
58.4289370982668));
#24371=CARTESIAN_POINT('Ctrl Pts',(-0.188885493857291,3.92846169259804,
58.4348153327219));
#24372=CARTESIAN_POINT('Ctrl Pts',(-0.205684189554592,3.92765398969008,
58.4356708360481));
#24373=CARTESIAN_POINT('Ctrl Pts',(-0.222473813232077,3.92673872131916,
58.4365263393742));
#24374=CARTESIAN_POINT('Ctrl Pts',(-0.239252888532522,3.92571612006381,
58.4373818427004));
#24375=CARTESIAN_POINT('Ctrl Pts',(-0.3545258843286,3.91869080382328,58.4432591887134));
#24376=CARTESIAN_POINT('Ctrl Pts',(-0.469678179270346,3.90657243372861,
58.4491365347265));
#24377=CARTESIAN_POINT('Ctrl Pts',(-0.58422391822207,3.88936645398415,58.4550138807396));
#24378=CARTESIAN_POINT('Ctrl Pts',(-0.69862326109188,3.87218246447734,58.4608837151644));
#24379=CARTESIAN_POINT('Ctrl Pts',(-0.81241718536282,3.84992385745057,58.4667535495892));
#24380=CARTESIAN_POINT('Ctrl Pts',(-0.925122199257555,3.82264802413731,
58.472623384014));
#24381=CARTESIAN_POINT('Ctrl Pts',(-1.03771316091207,3.79539979270071,58.478487278439));
#24382=CARTESIAN_POINT('Ctrl Pts',(-1.14921700547454,3.76314453084539,58.484351172864));
#24383=CARTESIAN_POINT('Ctrl Pts',(-1.25915836950832,3.72599103601944,58.4902150672889));
#24384=CARTESIAN_POINT('Ctrl Pts',(-1.37218074418515,3.68779634697153,58.4962432922304));
#24385=CARTESIAN_POINT('Ctrl Pts',(-1.48355132852975,3.64442488787103,58.5022715171718));
#24386=CARTESIAN_POINT('Ctrl Pts',(-1.59276778428541,3.59605058158844,58.5082997421132));
#24387=CARTESIAN_POINT('Ctrl Pts',(-1.69888739854487,3.54904793269951,58.5141570362456));
#24388=CARTESIAN_POINT('Ctrl Pts',(-1.8029730017585,3.49732251472514,58.5200143303779));
#24389=CARTESIAN_POINT('Ctrl Pts',(-1.90458280629988,3.44108316289318,58.5258716245103));
#24390=CARTESIAN_POINT('Ctrl Pts',(-2.00617794100624,3.38485193057307,58.5317280730005));
#24391=CARTESIAN_POINT('Ctrl Pts',(-2.10529762699227,3.32410826002245,58.5375845214906));
#24392=CARTESIAN_POINT('Ctrl Pts',(-2.20152470130567,3.25910693128363,58.5434409699808));
#24393=CARTESIAN_POINT('Ctrl Pts',(-2.29776106777071,3.19409932570217,58.5492979839979));
#24394=CARTESIAN_POINT('Ctrl Pts',(-2.39110392544248,3.12483347554203,58.555154998015));
#24395=CARTESIAN_POINT('Ctrl Pts',(-2.48116571288909,3.05160706926427,58.5610120120322));
#24396=CARTESIAN_POINT('Ctrl Pts',(-2.57583576307342,2.97463382951768,58.5671687165198));
#24397=CARTESIAN_POINT('Ctrl Pts',(-2.66687968578266,2.89328431438268,58.5733254210074));
#24398=CARTESIAN_POINT('Ctrl Pts',(-2.75388856641615,2.80795063413915,58.579482125495));
#24399=CARTESIAN_POINT('Ctrl Pts',(-2.83678546754567,2.72664976458811,58.5853478683878));
#24400=CARTESIAN_POINT('Ctrl Pts',(-2.91601974679324,2.64173304362052,58.5912136112807));
#24401=CARTESIAN_POINT('Ctrl Pts',(-2.9912779436942,2.5535749966603,58.5970793541736));
#24402=CARTESIAN_POINT('Ctrl Pts',(-3.06658789782654,2.46535632086997,58.6029491311069));
#24403=CARTESIAN_POINT('Ctrl Pts',(-3.13791607168383,2.37389220472495,58.6088189080402));
#24404=CARTESIAN_POINT('Ctrl Pts',(-3.20499138435813,2.27958751229038,58.6146886849736));
#24405=CARTESIAN_POINT('Ctrl Pts',(-3.27216183241156,2.18514906404743,58.6205667872271));
#24406=CARTESIAN_POINT('Ctrl Pts',(-3.33506716014055,2.08786234517067,58.6264448894806));
#24407=CARTESIAN_POINT('Ctrl Pts',(-3.39348138473765,1.9881582158971,58.6323229917341));
#24408=CARTESIAN_POINT('Ctrl Pts',(-3.40199285287121,1.97363044419508,58.6331794831172));
#24409=CARTESIAN_POINT('Ctrl Pts',(-3.41040905280243,1.95905138454428,58.6340359745003));
#24410=CARTESIAN_POINT('Ctrl Pts',(-3.41872937063379,1.94442240533429,58.6348924658833));
#24411=CARTESIAN_POINT('Ctrl Pts',(-3.47820543226259,1.83985018986187,58.6410149164095));
#24412=CARTESIAN_POINT('Ctrl Pts',(-3.53295935359999,1.73240702198956,58.6471373669357));
#24413=CARTESIAN_POINT('Ctrl Pts',(-3.58271656562753,1.62253844650233,58.6532598174618));
#24414=CARTESIAN_POINT('Ctrl Pts',(-3.63239088497217,1.51285290580777,58.6593720683339));
#24415=CARTESIAN_POINT('Ctrl Pts',(-3.67708492333178,1.40075033324975,58.665484319206));
#24416=CARTESIAN_POINT('Ctrl Pts',(-3.71656924016522,1.28670201797378,58.6715965700781));
#24417=CARTESIAN_POINT('Ctrl Pts',(-3.75597208802662,1.17288902142062,58.6776962093911));
#24418=CARTESIAN_POINT('Ctrl Pts',(-3.79018652288456,1.0571386266198,58.6837958487041));
#24419=CARTESIAN_POINT('Ctrl Pts',(-3.81903093378893,0.939942406088445,
58.6898954880171));
#24420=CARTESIAN_POINT('Ctrl Pts',(-3.84783991649881,0.822890132005107,
58.6959876354382));
#24421=CARTESIAN_POINT('Ctrl Pts',(-3.87129192094621,0.704395919129239,
58.7020797828594));
#24422=CARTESIAN_POINT('Ctrl Pts',(-3.88925465038843,0.584967746488714,
58.7081719302805));
#24423=CARTESIAN_POINT('Ctrl Pts',(-3.90719108832866,0.465714377240255,
58.7142551608103));
#24424=CARTESIAN_POINT('Ctrl Pts',(-3.91965421122248,0.34553013120326,58.7203383913401));
#24425=CARTESIAN_POINT('Ctrl Pts',(-3.9265625930753,0.224933773946519,58.7264216218699));
#24426=CARTESIAN_POINT('Ctrl Pts',(-3.93085931016457,0.149928014252427,
58.7302051302416));
#24427=CARTESIAN_POINT('Ctrl Pts',(-3.93300828556888,0.0747630755042776,
58.7339886386134));
#24428=CARTESIAN_POINT('Ctrl Pts',(-3.93299997598718,-0.000434608922615996,
58.7377721469851));
#24429=CARTESIAN_POINT('Ctrl Pts',(-3.93299997598709,-0.000434609756364034,
58.737772147027));
#24430=CARTESIAN_POINT('Ctrl Pts',(-3.93298638829109,-0.123396433039988,
58.7439588679526));
#24431=CARTESIAN_POINT('Ctrl Pts',(-3.92720208159448,-0.24622899957672,
58.7501455888783));
#24432=CARTESIAN_POINT('Ctrl Pts',(-3.91570891145027,-0.368392074818398,
58.7563323098039));
#24433=CARTESIAN_POINT('Ctrl Pts',(-3.90393241978397,-0.493566628006301,
58.762671541409));
#24434=CARTESIAN_POINT('Ctrl Pts',(-3.8861620251258,-0.618037871898027,
58.7690107730142));
#24435=CARTESIAN_POINT('Ctrl Pts',(-3.8625194007969,-0.741237396835596,
58.7753500046194));
#24436=CARTESIAN_POINT('Ctrl Pts',(-3.83934346399611,-0.862005056301857,
58.7815641045858));
#24437=CARTESIAN_POINT('Ctrl Pts',(-3.81052514587804,-0.981550438922573,
58.7877782045522));
#24438=CARTESIAN_POINT('Ctrl Pts',(-3.77622924634803,-1.09935511961599,
58.7939923045186));
#24439=CARTESIAN_POINT('Ctrl Pts',(-3.74089743603393,-1.22071810147133,
58.8003941019432));
#24440=CARTESIAN_POINT('Ctrl Pts',(-3.69975207331446,-1.34023319123688,
58.8067958993678));
#24441=CARTESIAN_POINT('Ctrl Pts',(-3.65302592841248,-1.45735739142676,
58.8131976967924));
#24442=CARTESIAN_POINT('Ctrl Pts',(-3.6062997835105,-1.57448159161665,58.819599494217));
#24443=CARTESIAN_POINT('Ctrl Pts',(-3.55399308169572,-1.68921458270921,
58.8260012916416));
#24444=CARTESIAN_POINT('Ctrl Pts',(-3.49638884021169,-1.80104249756723,
58.8324030890661));
#24445=CARTESIAN_POINT('Ctrl Pts',(-3.44350101193356,-1.90371437389691,
58.838280731999));
#24446=CARTESIAN_POINT('Ctrl Pts',(-3.38600025284171,-2.00422289819233,
58.8441583749319));
#24447=CARTESIAN_POINT('Ctrl Pts',(-3.32408739703009,-2.10212558542675,
58.8500360178648));
#24448=CARTESIAN_POINT('Ctrl Pts',(-3.26225364615663,-2.19990318416516,
58.8559061510395));
#24449=CARTESIAN_POINT('Ctrl Pts',(-3.19601922821315,-2.29508122176198,
58.8617762842141));
#24450=CARTESIAN_POINT('Ctrl Pts',(-3.12563156484665,-2.38724031484774,
58.8676464173887));
#24451=CARTESIAN_POINT('Ctrl Pts',(-3.05531510950412,-2.47930617473615,
58.8735106120144));
#24452=CARTESIAN_POINT('Ctrl Pts',(-2.98085401545927,-2.56835883939158,
58.8793748066401));
#24453=CARTESIAN_POINT('Ctrl Pts',(-2.90253947355337,-2.65400708447897,
58.8852390012658));
#24454=CARTESIAN_POINT('Ctrl Pts',(-2.82203585200479,-2.74204940383647,
58.8912671142234));
#24455=CARTESIAN_POINT('Ctrl Pts',(-2.73746041099675,-2.82649379389863,
58.8972952271811));
#24456=CARTESIAN_POINT('Ctrl Pts',(-2.64917473959605,-2.90695067021893,
58.9033233401387));
#24457=CARTESIAN_POINT('Ctrl Pts',(-2.5633864010418,-2.98513166646979,58.9091809361341));
#24458=CARTESIAN_POINT('Ctrl Pts',(-2.47409524585201,-3.05954741859253,
58.9150385321296));
#24459=CARTESIAN_POINT('Ctrl Pts',(-2.38167048197705,-3.12987774765713,
58.9208961281251));
#24460=CARTESIAN_POINT('Ctrl Pts',(-2.28925905977581,-3.20019792441769,
58.9267528785664));
#24461=CARTESIAN_POINT('Ctrl Pts',(-2.19371525654455,-3.26643360112181,
58.9326096290078));
#24462=CARTESIAN_POINT('Ctrl Pts',(-2.09544040396874,-3.32830565204209,
58.9384663794492));
#24463=CARTESIAN_POINT('Ctrl Pts',(-1.99715606608524,-3.39018367473873,
58.9443236951734));
#24464=CARTESIAN_POINT('Ctrl Pts',(-1.89614050391788,-3.44769701463841,
58.9501810108975));
#24465=CARTESIAN_POINT('Ctrl Pts',(-1.79282238876367,-3.50061092987321,
58.9560383266217));
#24466=CARTESIAN_POINT('Ctrl Pts',(-1.68423075796155,-3.55622565279857,
58.9621946087573));
#24467=CARTESIAN_POINT('Ctrl Pts',(-1.57309576447285,-3.60675879098142,
58.9683508908929));
#24468=CARTESIAN_POINT('Ctrl Pts',(-1.45994091604914,-3.65199418422944,
58.9745071730285));
#24469=CARTESIAN_POINT('Ctrl Pts',(-1.35212080864639,-3.69509693259904,
58.9803732142129));
#24470=CARTESIAN_POINT('Ctrl Pts',(-1.24246737256233,-3.73338998665922,
58.9862392553973));
#24471=CARTESIAN_POINT('Ctrl Pts',(-1.13144973577546,-3.76673738073331,
58.9921052965816));
#24472=CARTESIAN_POINT('Ctrl Pts',(-1.0203557757963,-3.80010770071039,58.9979753705936));
#24473=CARTESIAN_POINT('Ctrl Pts',(-0.907896146386374,-3.82852548957049,
59.0038454446055));
#24474=CARTESIAN_POINT('Ctrl Pts',(-0.794550664326466,-3.85190579347657,
59.0097155186175));
#24475=CARTESIAN_POINT('Ctrl Pts',(-0.681044496122018,-3.87531924286693,
59.0155939144394));
#24476=CARTESIAN_POINT('Ctrl Pts',(-0.566650374805284,-3.89368089219465,
59.0214723102613));
#24477=CARTESIAN_POINT('Ctrl Pts',(-0.451853736377204,-3.90695753763999,
59.0273507060832));
#24478=CARTESIAN_POINT('Ctrl Pts',(-0.435169791696756,-3.90888709604157,
59.0282050414718));
#24479=CARTESIAN_POINT('Ctrl Pts',(-0.418477344820747,-3.91070933780461,
59.0290593768604));
#24480=CARTESIAN_POINT('Ctrl Pts',(-0.40177788411543,-3.91242425253649,
59.0299137122491));
#24481=CARTESIAN_POINT('Ctrl Pts',(-0.286909493420838,-3.92422041164043,
59.0357903170649));
#24482=CARTESIAN_POINT('Ctrl Pts',(-0.171332551631751,-3.93097286977808,
59.0416669218808));
#24483=CARTESIAN_POINT('Ctrl Pts',(-0.0555272300337676,-3.93260800572912,
59.0475435266966));
#24484=CARTESIAN_POINT('Ctrl Pts',(0.0601300414201887,-3.93424105125711,
59.0534126186264));
#24485=CARTESIAN_POINT('Ctrl Pts',(0.176014703109235,-3.93076977955394,
59.0592817105561));
#24486=CARTESIAN_POINT('Ctrl Pts',(0.291640467311843,-3.92217220909869,
59.0651508024859));
#24487=CARTESIAN_POINT('Ctrl Pts',(0.407149200849934,-3.9135833406779,59.0710139540119));
#24488=CARTESIAN_POINT('Ctrl Pts',(0.522399149025639,-3.89987852482489,
59.0768771055379));
#24489=CARTESIAN_POINT('Ctrl Pts',(0.636903685379811,-3.88108782373571,
59.0827402570638));
#24490=CARTESIAN_POINT('Ctrl Pts',(0.754637461873528,-3.8617671900505,59.0887687603292));
#24491=CARTESIAN_POINT('Ctrl Pts',(0.871582712350225,-3.83706952811667,
59.0947972635945));
#24492=CARTESIAN_POINT('Ctrl Pts',(0.987215344586107,-3.80708482482512,
59.1008257668599));
#24493=CARTESIAN_POINT('Ctrl Pts',(1.09954983810318,-3.77795536203952,59.1066823217776));
#24494=CARTESIAN_POINT('Ctrl Pts',(1.21064515363453,-3.74383649058138,59.1125388766954));
#24495=CARTESIAN_POINT('Ctrl Pts',(1.32003153369388,-3.70486244684654,59.1183954316132));
#24496=CARTESIAN_POINT('Ctrl Pts',(1.4294021684974,-3.66589401309979,59.1242511435289));
#24497=CARTESIAN_POINT('Ctrl Pts',(1.53706396837671,-3.62207193522498,59.1301068554445));
#24498=CARTESIAN_POINT('Ctrl Pts',(1.64256400733718,-3.57357978528539,59.1359625673601));
#24499=CARTESIAN_POINT('Ctrl Pts',(1.74807429704893,-3.5250829236796,59.1418188482371));
#24500=CARTESIAN_POINT('Ctrl Pts',(1.85142203335346,-3.471915260312,59.1476751291141));
#24501=CARTESIAN_POINT('Ctrl Pts',(1.95217652726788,-3.41430751491196,59.1535314099911));
#24502=CARTESIAN_POINT('Ctrl Pts',(2.0581175454533,-3.35373430407106,59.1596891537778));
#24503=CARTESIAN_POINT('Ctrl Pts',(2.1611907829416,-3.28825196343846,59.1658468975645));
#24504=CARTESIAN_POINT('Ctrl Pts',(2.26092875103528,-3.21818119172026,59.1720046413513));
#24505=CARTESIAN_POINT('Ctrl Pts',(2.35592550779208,-3.15144135147784,59.1778696664752));
#24506=CARTESIAN_POINT('Ctrl Pts',(2.44789649712951,-3.08053958472428,59.1837346915992));
#24507=CARTESIAN_POINT('Ctrl Pts',(2.53647167680405,-3.00579447613618,59.1895997167231));
#24508=CARTESIAN_POINT('Ctrl Pts',(2.62510786062882,-2.93099788854629,59.1954687812504));
#24509=CARTESIAN_POINT('Ctrl Pts',(2.71034327535287,-2.85235296739318,59.2013378457776));
#24510=CARTESIAN_POINT('Ctrl Pts',(2.79184477099934,-2.77021511342415,59.2072069103048));
#24511=CARTESIAN_POINT('Ctrl Pts',(2.8734620420719,-2.68796058006211,59.213084312022));
#24512=CARTESIAN_POINT('Ctrl Pts',(2.95133453412424,-2.60220351727131,59.2189617137391));
#24513=CARTESIAN_POINT('Ctrl Pts',(3.02516937696303,-2.51333229810247,59.2248391154563));
#24514=CARTESIAN_POINT('Ctrl Pts',(3.03599498323125,-2.50030207022755,59.2257008554482));
#24515=CARTESIAN_POINT('Ctrl Pts',(3.04673386801589,-2.48720494651646,59.2265625954401));
#24516=CARTESIAN_POINT('Ctrl Pts',(3.05738518806404,-2.47404220089443,59.227424335432));
#24517=CARTESIAN_POINT('Ctrl Pts',(3.13004555183358,-2.3842495854459,59.2333028876681));
#24518=CARTESIAN_POINT('Ctrl Pts',(3.19886580446545,-2.2911063406,59.2391814399041));
#24519=CARTESIAN_POINT('Ctrl Pts',(3.26352187689826,-2.19497470577826,59.2450599921402));
#24520=CARTESIAN_POINT('Ctrl Pts',(3.32809529196935,-2.09896596718288,59.2509310291407));
#24521=CARTESIAN_POINT('Ctrl Pts',(3.38851488609573,-1.99997677564306,59.2568020661411));
#24522=CARTESIAN_POINT('Ctrl Pts',(3.44449651071182,-1.89840269376494,59.2626731031416));
#24523=CARTESIAN_POINT('Ctrl Pts',(3.50042144825045,-1.79693146595523,59.2685381951212));
#24524=CARTESIAN_POINT('Ctrl Pts',(3.5519171575756,-1.69288091346448,59.2744032871007));
#24525=CARTESIAN_POINT('Ctrl Pts',(3.59874290193592,-1.58667530571499,59.2802683790802));
#24526=CARTESIAN_POINT('Ctrl Pts',(3.64686746882529,-1.47752383478829,59.2862961532275));
#24527=CARTESIAN_POINT('Ctrl Pts',(3.69005895967147,-1.36609637212501,59.2923239273748));
#24528=CARTESIAN_POINT('Ctrl Pts',(3.72810663232228,-1.25288065594236,59.2983517015221));
#24529=CARTESIAN_POINT('Ctrl Pts',(3.76508565851155,-1.14284483398345,59.3042101733424));
#24530=CARTESIAN_POINT('Ctrl Pts',(3.79720583164214,-1.03112029185799,59.3100686451628));
#24531=CARTESIAN_POINT('Ctrl Pts',(3.82432286679152,-0.918174063310112,
59.3159271169831));
#24532=CARTESIAN_POINT('Ctrl Pts',(3.85143594431274,-0.805244318834775,
59.3217847337818));
#24533=CARTESIAN_POINT('Ctrl Pts',(3.87354723963922,-0.691093643335088,
59.3276423505805));
#24534=CARTESIAN_POINT('Ctrl Pts',(3.89056298456905,-0.576201929102187,
59.3334999673792));
#24535=CARTESIAN_POINT('Ctrl Pts',(3.90758034144363,-0.46129933088524,59.3393581390848));
#24536=CARTESIAN_POINT('Ctrl Pts',(3.91950112792571,-0.345655962286249,
59.3452163107904));
#24537=CARTESIAN_POINT('Ctrl Pts',(3.92628321296247,-0.229758855344093,
59.351074482496));
#24538=CARTESIAN_POINT('Ctrl Pts',(3.93340898608571,-0.107988561218616,
59.3572295221725));
#24539=CARTESIAN_POINT('Ctrl Pts',(3.93486154728916,0.0140613566219913,
59.3633845618491));
#24540=CARTESIAN_POINT('Ctrl Pts',(3.9306539578738,0.135825120839118,59.3695396015257));
#24541=CARTESIAN_POINT('Ctrl Pts',(3.9266433659979,0.251887957617895,59.3754064648733));
#24542=CARTESIAN_POINT('Ctrl Pts',(3.91749072180953,0.367690413961021,59.3812733282208));
#24543=CARTESIAN_POINT('Ctrl Pts',(3.90326057992152,0.482748221364511,59.3871401915684));
#24544=CARTESIAN_POINT('Ctrl Pts',(3.88902068475051,0.597884888934454,59.3930110760409));
#24545=CARTESIAN_POINT('Ctrl Pts',(3.86969643059257,0.712275485802583,59.3988819605135));
#24546=CARTESIAN_POINT('Ctrl Pts',(3.84540336846444,0.825446505718101,59.404752844986));
#24547=CARTESIAN_POINT('Ctrl Pts',(3.82107596005679,0.938777530307518,59.4106320298958));
#24548=CARTESIAN_POINT('Ctrl Pts',(3.79176582972588,1.05088514016715,59.4165112148057));
#24549=CARTESIAN_POINT('Ctrl Pts',(3.75763815878209,1.16131152911896,59.4223903997155));
#24550=CARTESIAN_POINT('Ctrl Pts',(3.75271458121455,1.17724267462267,59.4232385860153));
#24551=CARTESIAN_POINT('Ctrl Pts',(3.74769081402651,1.19313886356976,59.424086772315));
#24552=CARTESIAN_POINT('Ctrl Pts',(3.74256743438735,1.20899875891715,59.4249349586148));
#24553=CARTESIAN_POINT('Ctrl Pts',(3.70705934153858,1.31891734317774,59.4308133982399));
#24554=CARTESIAN_POINT('Ctrl Pts',(3.66664671419419,1.42744985201521,59.436691837865));
#24555=CARTESIAN_POINT('Ctrl Pts',(3.62145598834394,1.53412695839938,59.44257027749));
#24556=CARTESIAN_POINT('Ctrl Pts',(3.5763229008701,1.6406680037866,59.4484412194769));
#24557=CARTESIAN_POINT('Ctrl Pts',(3.52642399432385,1.74535797677613,59.4543121614637));
#24558=CARTESIAN_POINT('Ctrl Pts',(3.47193542213628,1.84774279176386,59.4601831034505));
#24559=CARTESIAN_POINT('Ctrl Pts',(3.41750186398949,1.95002423457351,59.466048117878));
#24560=CARTESIAN_POINT('Ctrl Pts',(3.35848805055208,2.05000478708441,59.4719131323055));
#24561=CARTESIAN_POINT('Ctrl Pts',(3.29511789235706,2.14725105087139,59.477778146733));
#24562=CARTESIAN_POINT('Ctrl Pts',(3.22998876693747,2.24719658187791,59.4838059565274));
#24563=CARTESIAN_POINT('Ctrl Pts',(3.16025808282592,2.34425339745184,59.4898337663218));
#24564=CARTESIAN_POINT('Ctrl Pts',(3.08621931271244,2.43797853842906,59.4958615761161));
#24565=CARTESIAN_POINT('Ctrl Pts',(3.01426091902777,2.5290701460051,59.501720013656));
#24566=CARTESIAN_POINT('Ctrl Pts',(2.93823359066717,2.61701447246204,59.5075784511959));
#24567=CARTESIAN_POINT('Ctrl Pts',(2.85844974123687,2.70143555851751,59.5134368887357));
#24568=CARTESIAN_POINT('Ctrl Pts',(2.77867731787939,2.78584455438827,59.519294487272));
#24569=CARTESIAN_POINT('Ctrl Pts',(2.69514972639875,2.86673101362479,59.5251520858084));
#24570=CARTESIAN_POINT('Ctrl Pts',(2.60821774187903,2.9437542714954,59.5310096843447));
#24571=CARTESIAN_POINT('Ctrl Pts',(2.52127728521412,3.02078503583474,59.536867853746));
#24572=CARTESIAN_POINT('Ctrl Pts',(2.43093208457753,3.09395157690207,59.5427260231472));
#24573=CARTESIAN_POINT('Ctrl Pts',(2.33756709784436,3.16295258628318,59.5485841925485));
#24574=CARTESIAN_POINT('Ctrl Pts',(2.23946950746874,3.23545120691831,59.5547393083193));
#24575=CARTESIAN_POINT('Ctrl Pts',(2.13803836325414,3.30335061655387,59.5608944240901));
#24576=CARTESIAN_POINT('Ctrl Pts',(2.03375474315252,3.36635272137437,59.5670495398608));
#24577=CARTESIAN_POINT('Ctrl Pts',(1.93435423171398,3.42640473562894,59.572916440674));
#24578=CARTESIAN_POINT('Ctrl Pts',(1.83236272648546,3.48200754090552,59.5787833414872));
#24579=CARTESIAN_POINT('Ctrl Pts',(1.72822113911942,3.53295070646347,59.5846502423004));
#24580=CARTESIAN_POINT('Ctrl Pts',(1.62400793238906,3.58392890622078,59.5905211778486));
#24581=CARTESIAN_POINT('Ctrl Pts',(1.51764207618984,3.63024092116307,59.5963921133968));
#24582=CARTESIAN_POINT('Ctrl Pts',(1.40958331825366,3.67172491737888,59.602263048945));
#24583=CARTESIAN_POINT('Ctrl Pts',(1.30137143848424,3.71326769740521,59.6081423037486));
#24584=CARTESIAN_POINT('Ctrl Pts',(1.19146225961509,3.74996867734835,59.6140215585523));
#24585=CARTESIAN_POINT('Ctrl Pts',(1.08032948423019,3.78171617199161,59.6199008133559));
#24586=CARTESIAN_POINT('Ctrl Pts',(1.06429529911185,3.78629668574546,59.6207490695032));
#24587=CARTESIAN_POINT('Ctrl Pts',(1.04823565714201,3.79077417225764,59.6215973256504));
#24588=CARTESIAN_POINT('Ctrl Pts',(1.03215199383441,3.79514838466477,59.6224455817977));
#24589=CARTESIAN_POINT('Ctrl Pts',(0.920833718315192,3.82542319038558,59.6283165335643));
#24590=CARTESIAN_POINT('Ctrl Pts',(0.807997354646353,3.85084640293736,59.6341874853308));
#24591=CARTESIAN_POINT('Ctrl Pts',(0.69410380974655,3.871267092477,59.6400584370974));
#24592=CARTESIAN_POINT('Ctrl Pts',(0.580356270243658,3.89166160379131,59.6459218626197));
#24593=CARTESIAN_POINT('Ctrl Pts',(0.465554647974981,3.90706627292493,59.6517852881421));
#24594=CARTESIAN_POINT('Ctrl Pts',(0.350174337588973,3.91738011090245,59.6576487136643));
#24595=CARTESIAN_POINT('Ctrl Pts',(0.234911052071881,3.92768348803503,59.6635061921875));
#24596=CARTESIAN_POINT('Ctrl Pts',(0.119070655354441,3.93290626773586,59.6693636707107));
#24597=CARTESIAN_POINT('Ctrl Pts',(0.00313738484995835,3.93299874864159,
59.6752211492339));
#24598=CARTESIAN_POINT('Ctrl Pts',(-0.116222907459339,3.93309396331027,
59.6812517765567));
#24599=CARTESIAN_POINT('Ctrl Pts',(-0.235681210891267,3.92775076617025,
59.6872824038795));
#24600=CARTESIAN_POINT('Ctrl Pts',(-0.35470450151807,3.91697251925551,59.6933130312022));
#24601=CARTESIAN_POINT('Ctrl Pts',(-0.470180628499413,3.90651548851128,
59.6991639321716));
#24602=CARTESIAN_POINT('Ctrl Pts',(-0.585246863951679,3.89094281569465,
59.7050148331409));
#24603=CARTESIAN_POINT('Ctrl Pts',(-0.69941862137128,3.87031039996524,59.7108657341102));
#24604=CARTESIAN_POINT('Ctrl Pts',(-0.813574253703784,3.8496808982621,59.7167158087256));
#24605=CARTESIAN_POINT('Ctrl Pts',(-0.926835252369466,3.82399314808559,
59.7225658833409));
#24606=CARTESIAN_POINT('Ctrl Pts',(-1.03872561286469,3.79335446553297,59.7284159579562));
#24607=CARTESIAN_POINT('Ctrl Pts',(-1.15062728847733,3.76271268458751,59.7342666241711));
#24608=CARTESIAN_POINT('Ctrl Pts',(-1.26115765152597,3.7271190851998,59.7401172903859));
#24609=CARTESIAN_POINT('Ctrl Pts',(-1.36985498049327,3.68673111745592,59.7459679566008));
#24610=CARTESIAN_POINT('Ctrl Pts',(-1.47858964580015,3.64632927688837,59.7518206324552));
#24611=CARTESIAN_POINT('Ctrl Pts',(-1.58548963766565,3.60112993735095,59.7576733083097));
#24612=CARTESIAN_POINT('Ctrl Pts',(-1.69011303260906,3.55133875278113,59.7635259841642));
#24613=CARTESIAN_POINT('Ctrl Pts',(-1.79485550045048,3.50149090038243,59.7693853210057));
#24614=CARTESIAN_POINT('Ctrl Pts',(-1.89731582659599,3.44704095049977,59.7752446578472));
#24615=CARTESIAN_POINT('Ctrl Pts',(-1.9970764577922,3.38824063810884,59.7811039946887));
#24616=CARTESIAN_POINT('Ctrl Pts',(-2.09690534358347,3.32940009550421,59.7869673403927));
#24617=CARTESIAN_POINT('Ctrl Pts',(-2.1940305109698,3.26620348883162,59.7928306860968));
#24618=CARTESIAN_POINT('Ctrl Pts',(-2.28806461775223,3.19894503000448,59.7986940318009));
#24619=CARTESIAN_POINT('Ctrl Pts',(-2.38223514931497,3.13158899253506,59.8045658840531));
#24620=CARTESIAN_POINT('Ctrl Pts',(-2.4733053472488,3.0601595974302,59.8104377363053));
#24621=CARTESIAN_POINT('Ctrl Pts',(-2.56092203913391,2.98499033658038,59.8163095885574));
#24622=CARTESIAN_POINT('Ctrl Pts',(-2.57905967009159,2.969429462467,59.8175251273651));
#24623=CARTESIAN_POINT('Ctrl Pts',(-2.59704943683639,2.95370844251526,59.8187406661728));
#24624=CARTESIAN_POINT('Ctrl Pts',(-2.61488841530372,2.9378304198014,59.8199562049805));
#24625=CARTESIAN_POINT('Ctrl Pts',(-2.70005904694706,2.86202219870492,59.8257596879673));
#24626=CARTESIAN_POINT('Ctrl Pts',(-2.78208717217367,2.78236726364629,59.8315631709542));
#24627=CARTESIAN_POINT('Ctrl Pts',(-2.86059898584348,2.69915958071977,59.837366653941));
#24628=CARTESIAN_POINT('Ctrl Pts',(-2.93900947422837,2.61605928344372,59.8431626471051));
#24629=CARTESIAN_POINT('Ctrl Pts',(-3.01391238330406,2.52941565788114,59.8489586402692));
#24630=CARTESIAN_POINT('Ctrl Pts',(-3.08496744691924,2.43956243032406,59.8547546334334));
#24631=CARTESIAN_POINT('Ctrl Pts',(-3.1559427125746,2.34981011189123,59.8605441174424));
#24632=CARTESIAN_POINT('Ctrl Pts',(-3.22307846824127,2.25685569311537,59.8663336014514));
#24633=CARTESIAN_POINT('Ctrl Pts',(-3.2860724371803,2.16106847129007,59.8721230854604));
#24634=CARTESIAN_POINT('Ctrl Pts',(-3.3490272798566,2.06534074398576,59.8779089735558));
#24635=CARTESIAN_POINT('Ctrl Pts',(-3.40784521526477,1.96678406291508,59.8836948616511));
#24636=CARTESIAN_POINT('Ctrl Pts',(-3.46226560101986,1.86579899989111,59.8894807497465));
#24637=CARTESIAN_POINT('Ctrl Pts',(-3.51666611407386,1.76485081359897,59.8952645250082));
#24638=CARTESIAN_POINT('Ctrl Pts',(-3.56667206870605,1.66147638095618,59.9010483002699));
#24639=CARTESIAN_POINT('Ctrl Pts',(-3.61206779602966,1.55610257916551,59.9068320755315));
#24640=CARTESIAN_POINT('Ctrl Pts',(-3.65745856371834,1.45074028981484,59.9126152188964));
#24641=CARTESIAN_POINT('Ctrl Pts',(-3.6982399392204,1.3433794556174,59.9183983622613));
#24642=CARTESIAN_POINT('Ctrl Pts',(-3.73424395708088,1.23446792951662,59.9241815056262));
#24643=CARTESIAN_POINT('Ctrl Pts',(-3.77026966288204,1.12549079777353,59.9299681326154));
#24644=CARTESIAN_POINT('Ctrl Pts',(-3.80151212814882,1.01496151105195,59.9357547596045));
#24645=CARTESIAN_POINT('Ctrl Pts',(-3.8278530225736,0.903343919874489,59.9415413865937));
#24646=CARTESIAN_POINT('Ctrl Pts',(-3.8542021824487,0.791691304462895,59.9473298293556));
#24647=CARTESIAN_POINT('Ctrl Pts',(-3.87564662640377,0.678950120736433,
59.9531182721175));
#24648=CARTESIAN_POINT('Ctrl Pts',(-3.89211932283257,0.565593649923186,
59.9589067148794));
#24649=CARTESIAN_POINT('Ctrl Pts',(-3.90861163564203,0.452102189450431,
59.9647020507627));
#24650=CARTESIAN_POINT('Ctrl Pts',(-3.92012033260397,0.337994400458905,
59.9704973866461));
#24651=CARTESIAN_POINT('Ctrl Pts',(-3.92663034482843,0.22374792752712,59.9762927225294));
#24652=CARTESIAN_POINT('Ctrl Pts',(-3.93092869755112,0.148314637841466,
59.9801191973368));
#24653=CARTESIAN_POINT('Ctrl Pts',(-3.93304893094804,0.0728209313073551,
59.9839456721443));
#24654=CARTESIAN_POINT('Ctrl Pts',(-3.9329991429617,-0.00259643266824124,
59.9877721469517));
#24655=CARTESIAN_POINT('Origin',(-9.35406549764863E-15,0.,41.4527091182931));
#24656=CARTESIAN_POINT('',(3.08633327008855,-0.927720059309073,50.1419356690201));
#24657=CARTESIAN_POINT('Ctrl Pts',(3.08633327008855,-0.927720059309073,
50.1419356690201));
#24658=CARTESIAN_POINT('Ctrl Pts',(3.13685348859573,-0.759649713490565,
50.1534735349637));
#24659=CARTESIAN_POINT('Ctrl Pts',(3.17356710806874,-0.587711993181435,
50.16542241742));
#24660=CARTESIAN_POINT('Ctrl Pts',(3.2122200237151,-0.289034929219761,50.1857202293767));
#24661=CARTESIAN_POINT('Ctrl Pts',(3.22104582932805,-0.163606356509486,
50.1941131152217));
#24662=CARTESIAN_POINT('Ctrl Pts',(3.2232399976714,0.0225944212214418,50.2062819931546));
#24663=CARTESIAN_POINT('Ctrl Pts',(3.22224602972785,0.0831735796066807,
50.2101967129909));
#24664=CARTESIAN_POINT('Ctrl Pts',(3.21722795830564,0.195607969746975,50.2173784201255));
#24665=CARTESIAN_POINT('Ctrl Pts',(3.21365538769434,0.247462636076168,50.2206573898647));
#24666=CARTESIAN_POINT('Ctrl Pts',(3.20549926368679,0.334931489911482,50.2261354927619));
#24667=CARTESIAN_POINT('Ctrl Pts',(3.20157210717137,0.370595247070645,50.2283541934687));
#24668=CARTESIAN_POINT('Ctrl Pts',(3.19294606514685,0.438489784230139,50.232552046447));
#24669=CARTESIAN_POINT('Ctrl Pts',(3.18835255187181,0.470729208883945,50.2345341454286));
#24670=CARTESIAN_POINT('Ctrl Pts',(3.17489470238123,0.555916046152079,50.2397452301427));
#24671=CARTESIAN_POINT('Ctrl Pts',(3.16519459434201,0.608722172473708,50.2429483781026));
#24672=CARTESIAN_POINT('Ctrl Pts',(3.10582757262411,0.89189854007648,50.2600222140235));
#24673=CARTESIAN_POINT('Ctrl Pts',(3.03232745225429,1.11653350180377,50.273130271094));
#24674=CARTESIAN_POINT('Ctrl Pts',(2.89343794092022,1.42276206254468,50.2920934009401));
#24675=CARTESIAN_POINT('Ctrl Pts',(2.84762737509321,1.51236608636721,50.2977988153934));
#24676=CARTESIAN_POINT('Ctrl Pts',(2.77623870771935,1.63721913016987,50.3061675042645));
#24677=CARTESIAN_POINT('Ctrl Pts',(2.75401971170232,1.67432462506036,50.308710414296));
#24678=CARTESIAN_POINT('Ctrl Pts',(2.71275607925004,1.74018990650942,50.3133460520374));
#24679=CARTESIAN_POINT('Ctrl Pts',(2.69398338432274,1.76911270729488,50.3154252790585));
#24680=CARTESIAN_POINT('Ctrl Pts',(2.66297650078571,1.81524633915605,50.3188222229089));
#24681=CARTESIAN_POINT('Ctrl Pts',(2.6510304220032,1.83264856437271,50.3201225024542));
#24682=CARTESIAN_POINT('Ctrl Pts',(2.626605590923,1.86749041659045,50.3227669347323));
#24683=CARTESIAN_POINT('Ctrl Pts',(2.61412204161715,1.88492526914433,50.3241114260391));
#24684=CARTESIAN_POINT('Ctrl Pts',(2.5796599132161,1.93205515471179,50.3278011760857));
#24685=CARTESIAN_POINT('Ctrl Pts',(2.55734377894605,1.96149813185895,50.33016697198));
#24686=CARTESIAN_POINT('Ctrl Pts',(2.42039429742089,2.13587321435007,50.3445162771805));
#24687=CARTESIAN_POINT('Ctrl Pts',(2.29398182210057,2.27110132943294,50.3570511377045));
#24688=CARTESIAN_POINT('Ctrl Pts',(2.02288472296532,2.51524962568076,50.3816548591468));
#24689=CARTESIAN_POINT('Ctrl Pts',(1.87919905759162,2.62434162094821,50.3936820365134));
#24690=CARTESIAN_POINT('Ctrl Pts',(1.67376853888951,2.75474356212943,50.4093571201811));
#24691=CARTESIAN_POINT('Ctrl Pts',(1.6194135196018,2.78704394382615,50.4133765314517));
#24692=CARTESIAN_POINT('Ctrl Pts',(1.53111321739769,2.83606008353103,50.419707988439));
#24693=CARTESIAN_POINT('Ctrl Pts',(1.4977651725816,2.85381221542383,50.4220557201799));
#24694=CARTESIAN_POINT('Ctrl Pts',(1.43293144078974,2.88687548898488,50.4265395535711));
#24695=CARTESIAN_POINT('Ctrl Pts',(1.40149344491668,2.90226788485684,50.428678228009));
#24696=CARTESIAN_POINT('Ctrl Pts',(1.32654251036697,2.9374627470053,50.433697102474));
#24697=CARTESIAN_POINT('Ctrl Pts',(1.28282684860697,2.95681552568822,50.4365618254308));
#24698=CARTESIAN_POINT('Ctrl Pts',(1.12596652202807,3.02212300216649,50.4466392108348));
#24699=CARTESIAN_POINT('Ctrl Pts',(1.01065553947981,3.0626145086386,50.4536758175758));
#24700=CARTESIAN_POINT('Ctrl Pts',(0.697565891709428,3.1529393280572,50.4721644283239));
#24701=CARTESIAN_POINT('Ctrl Pts',(0.496912601079402,3.19072037772553,50.4833634460264));
#24702=CARTESIAN_POINT('Ctrl Pts',(0.204902367362186,3.21747502615022,50.5001312974058));
#24703=CARTESIAN_POINT('Ctrl Pts',(0.1154662521291,3.22192417344698,50.50533442865));
#24704=CARTESIAN_POINT('Ctrl Pts',(-0.00312374491549286,3.22287980685227,
50.5124542150706));
#24705=CARTESIAN_POINT('Ctrl Pts',(-0.0322172045423297,3.22272026765864,
50.514218522677));
#24706=CARTESIAN_POINT('Ctrl Pts',(-0.0811194089388643,3.2217898787515,
50.5172195995788));
#24707=CARTESIAN_POINT('Ctrl Pts',(-0.10093111086254,3.22123008758901,50.5184452959748));
#24708=CARTESIAN_POINT('Ctrl Pts',(-0.143319967612828,3.21964092412135,
50.5210908262252));
#24709=CARTESIAN_POINT('Ctrl Pts',(-0.165893164453825,3.21855676997438,
50.522513313459));
#24710=CARTESIAN_POINT('Ctrl Pts',(-0.232057580356062,3.2146811328333,50.5267192284953));
#24711=CARTESIAN_POINT('Ctrl Pts',(-0.27560408052192,3.21124080028935,50.5295338102967));
#24712=CARTESIAN_POINT('Ctrl Pts',(-0.520130950457913,3.18691216874051,
50.5455514951931));
#24713=CARTESIAN_POINT('Ctrl Pts',(-0.718860105977541,3.14804369002197,
50.5593488360495));
#24714=CARTESIAN_POINT('Ctrl Pts',(-1.08341101543709,3.04040230833409,50.5849400854615));
#24715=CARTESIAN_POINT('Ctrl Pts',(-1.24973669728024,2.97590325680127,50.5967368707795));
#24716=CARTESIAN_POINT('Ctrl Pts',(-1.45511732340627,2.87598323464553,50.611296362327));
#24717=CARTESIAN_POINT('Ctrl Pts',(-1.49981439933665,2.85292888320626,50.6144664192762));
#24718=CARTESIAN_POINT('Ctrl Pts',(-1.57475538528106,2.81202671375218,50.619786862669));
#24719=CARTESIAN_POINT('Ctrl Pts',(-1.60527934530082,2.79471414286986,50.621955523527));
#24720=CARTESIAN_POINT('Ctrl Pts',(-1.66684612988226,2.75845312799999,50.6263353849259));
#24721=CARTESIAN_POINT('Ctrl Pts',(-1.69786318909509,2.73947083167311,50.6285449572063));
#24722=CARTESIAN_POINT('Ctrl Pts',(-1.77686688864992,2.68926356531442,50.6341855497439));
#24723=CARTESIAN_POINT('Ctrl Pts',(-1.82435576520394,2.65727700792887,50.6375881702418));
#24724=CARTESIAN_POINT('Ctrl Pts',(-2.04138047685718,2.50253603299261,50.6532414743377));
#24725=CARTESIAN_POINT('Ctrl Pts',(-2.19955331342346,2.36471892350634,50.6649119598523));
#24726=CARTESIAN_POINT('Ctrl Pts',(-2.46501678096647,2.08357034282935,50.6865539904165));
#24727=CARTESIAN_POINT('Ctrl Pts',(-2.57591155249613,1.94479767804143,50.6964910790293));
#24728=CARTESIAN_POINT('Ctrl Pts',(-2.6930441691688,1.77050796956148,50.7090249300383));
#24729=CARTESIAN_POINT('Ctrl Pts',(-2.71085700133695,1.74311201550285,50.7109968903079));
#24730=CARTESIAN_POINT('Ctrl Pts',(-2.73908901553656,1.6982118883219,50.71423982233));
#24731=CARTESIAN_POINT('Ctrl Pts',(-2.74976478067043,1.68087057179405,50.7154949397547));
#24732=CARTESIAN_POINT('Ctrl Pts',(-2.77127601933335,1.64517507374303,50.718086196289));
#24733=CARTESIAN_POINT('Ctrl Pts',(-2.78209496726725,1.62681262971739,50.7194230991081));
#24734=CARTESIAN_POINT('Ctrl Pts',(-2.8111454408908,1.57636937556066,50.7231034608115));
#24735=CARTESIAN_POINT('Ctrl Pts',(-2.82900885013162,1.54408152604282,50.7254676619173));
#24736=CARTESIAN_POINT('Ctrl Pts',(-2.93264936737491,1.34891500678954,50.7397771430256));
#24737=CARTESIAN_POINT('Ctrl Pts',(-3.00489103698888,1.17924753251186,50.7522739254275));
#24738=CARTESIAN_POINT('Ctrl Pts',(-3.1051649512933,0.873515310599367,50.7739931373521));
#24739=CARTESIAN_POINT('Ctrl Pts',(-3.13965133148799,0.740049616714836,
50.7832303132723));
#24740=CARTESIAN_POINT('Ctrl Pts',(-3.17739305073633,0.542503971100684,
50.7964072906922));
#24741=CARTESIAN_POINT('Ctrl Pts',(-3.18745101811869,0.479889564815537,
50.8005145078508));
#24742=CARTESIAN_POINT('Ctrl Pts',(-3.20258902322406,0.363884727118246,
50.8079933740099));
#24743=CARTESIAN_POINT('Ctrl Pts',(-3.20819653648734,0.31058666027832,50.8113792965692));
#24744=CARTESIAN_POINT('Ctrl Pts',(-3.21533538737369,0.221411086604464,
50.8169639182265));
#24745=CARTESIAN_POINT('Ctrl Pts',(-3.21760089447557,0.185604877272735,
50.819184766121));
#24746=CARTESIAN_POINT('Ctrl Pts',(-3.22094185891495,0.113790316646707,
50.8235983556407));
#24747=CARTESIAN_POINT('Ctrl Pts',(-3.22201242244565,0.0777869219772379,
50.8257906351577));
#24748=CARTESIAN_POINT('Ctrl Pts',(-3.22318388300327,-0.0125848122350477,
50.8312466371793));
#24749=CARTESIAN_POINT('Ctrl Pts',(-3.22251307841298,-0.0669528803071431,
50.8344863849312));
#24750=CARTESIAN_POINT('Ctrl Pts',(-3.21152665457355,-0.358685216055101,
50.851686127683));
#24751=CARTESIAN_POINT('Ctrl Pts',(-3.17636421075039,-0.594372392630117,
50.8648583487903));
#24752=CARTESIAN_POINT('Ctrl Pts',(-3.08898906648665,-0.924718045923707,
50.8840560188992));
#24753=CARTESIAN_POINT('Ctrl Pts',(-3.05750694141818,-1.02401455906482,
50.889938640144));
#24754=CARTESIAN_POINT('Ctrl Pts',(-3.00595299420508,-1.16288558383963,
50.8985371769));
#24755=CARTESIAN_POINT('Ctrl Pts',(-2.98978532652108,-1.20384369531999,
50.9011209426701));
#24756=CARTESIAN_POINT('Ctrl Pts',(-2.95932421911207,-1.27660988032735,
50.9058188869767));
#24757=CARTESIAN_POINT('Ctrl Pts',(-2.94534384396209,-1.30854195213678,
50.9079184760733));
#24758=CARTESIAN_POINT('Ctrl Pts',(-2.92214512621198,-1.35927313639041,
50.9113250061042));
#24759=CARTESIAN_POINT('Ctrl Pts',(-2.91325636743957,-1.37822091096904,
50.9126134084705));
#24760=CARTESIAN_POINT('Ctrl Pts',(-2.89510964291145,-1.41594346140055,
50.915213388997));
#24761=CARTESIAN_POINT('Ctrl Pts',(-2.8858520432938,-1.43471727358412,50.9165249220915));
#24762=CARTESIAN_POINT('Ctrl Pts',(-2.86062661436476,-1.48464075896815,
50.9200570934682));
#24763=CARTESIAN_POINT('Ctrl Pts',(-2.84433346285337,-1.51562189639145,
50.9222958825958));
#24764=CARTESIAN_POINT('Ctrl Pts',(-2.72864510662595,-1.72716368864217,
50.9378768465314));
#24765=CARTESIAN_POINT('Ctrl Pts',(-2.61263775555365,-1.89808128277749,
50.9519269314204));
#24766=CARTESIAN_POINT('Ctrl Pts',(-2.36102051270327,-2.20161557159665,
50.9784949113271));
#24767=CARTESIAN_POINT('Ctrl Pts',(-2.22845255021441,-2.33571126030287,
50.9909899126789));
#24768=CARTESIAN_POINT('Ctrl Pts',(-2.04619088503711,-2.49034133099285,
51.0062308344743));
#24769=CARTESIAN_POINT('Ctrl Pts',(-2.00668919870367,-2.52227992252108,
51.0094335987568));
#24770=CARTESIAN_POINT('Ctrl Pts',(-1.93844643854729,-2.57483826159254,
51.0148026120983));
#24771=CARTESIAN_POINT('Ctrl Pts',(-1.91009196339019,-2.59594212507118,
51.0169874751686));
#24772=CARTESIAN_POINT('Ctrl Pts',(-1.85170995302399,-2.63792050912542,
51.0213962416543));
#24773=CARTESIAN_POINT('Ctrl Pts',(-1.82166279008571,-2.65875896046727,
51.0236185659754));
#24774=CARTESIAN_POINT('Ctrl Pts',(-1.74348776548612,-2.71102771996091,
51.0292865800497));
#24775=CARTESIAN_POINT('Ctrl Pts',(-1.69486101335956,-2.74169065105194,
51.0327038878865));
#24776=CARTESIAN_POINT('Ctrl Pts',(-1.49421570631325,-2.8608335058814,51.0464129326366));
#24777=CARTESIAN_POINT('Ctrl Pts',(-1.33589178380515,-2.93810311525452,
51.056322416913));
#24778=CARTESIAN_POINT('Ctrl Pts',(-1.03787918618702,-3.05445038454346,
51.0742508374183));
#24779=CARTESIAN_POINT('Ctrl Pts',(-0.900364279575766,-3.09777344529481,
51.0822731865236));
#24780=CARTESIAN_POINT('Ctrl Pts',(-0.709491233437202,-3.14411936337167,
51.0935803218847));
#24781=CARTESIAN_POINT('Ctrl Pts',(-0.658269286571034,-3.15524094146588,
51.0966318516028));
#24782=CARTESIAN_POINT('Ctrl Pts',(-0.568185561978951,-3.17251142354894,
51.1020634826264));
#24783=CARTESIAN_POINT('Ctrl Pts',(-0.529439230667669,-3.17920703288653,
51.1044205117754));
#24784=CARTESIAN_POINT('Ctrl Pts',(-0.49058209429631,-3.18519179505032,
51.1068136617517));
#24785=CARTESIAN_POINT('',(1.91684063918175,2.59072181572651,50.1419356690201));
#24786=CARTESIAN_POINT('Origin',(-1.041818884589E-14,0.,50.1419356690201));
#24787=CARTESIAN_POINT('',(-3.22274873162613,0.00285924854630651,50.5811622197476));
#24788=CARTESIAN_POINT('Ctrl Pts',(-3.22274873162613,0.00285924854630654,
50.5811622197476));
#24789=CARTESIAN_POINT('Ctrl Pts',(-3.22262606019522,0.141126066550874,
50.5726197745096));
#24790=CARTESIAN_POINT('Ctrl Pts',(-3.21360167581526,0.279007275896255,
50.5640773292716));
#24791=CARTESIAN_POINT('Ctrl Pts',(-3.19584473577038,0.415564660851703,
50.5555348840336));
#24792=CARTESIAN_POINT('Ctrl Pts',(-3.1829722359087,0.514558908425243,50.5493422278177));
#24793=CARTESIAN_POINT('Ctrl Pts',(-3.16551157989265,0.612858278864528,
50.5431495716017));
#24794=CARTESIAN_POINT('Ctrl Pts',(-3.14354197865906,0.710113646473836,
50.5369569153858));
#24795=CARTESIAN_POINT('Ctrl Pts',(-3.1218293532884,0.80623142939279,50.5308366939473));
#24796=CARTESIAN_POINT('Ctrl Pts',(-3.09566276943955,0.90153560505576,50.5247164725087));
#24797=CARTESIAN_POINT('Ctrl Pts',(-3.06511720146087,0.995577271641297,
50.5185962510702));
#24798=CARTESIAN_POINT('Ctrl Pts',(-3.03461292647625,1.08949180809844,50.5124843032466));
#24799=CARTESIAN_POINT('Ctrl Pts',(-2.99974156371624,1.18214680967076,50.506372355423));
#24800=CARTESIAN_POINT('Ctrl Pts',(-2.96062902974355,1.27310380988347,50.5002604075994));
#24801=CARTESIAN_POINT('Ctrl Pts',(-2.92155733029939,1.36396584856231,50.4941548408124));
#24802=CARTESIAN_POINT('Ctrl Pts',(-2.87825343276076,1.45313300486155,50.4880492740253));
#24803=CARTESIAN_POINT('Ctrl Pts',(-2.83089263567421,1.54018325136511,50.4819437072382));
#24804=CARTESIAN_POINT('Ctrl Pts',(-2.78356365430523,1.62717501983984,50.4758422420077));
#24805=CARTESIAN_POINT('Ctrl Pts',(-2.73218339858752,1.71205231641932,50.4697407767772));
#24806=CARTESIAN_POINT('Ctrl Pts',(-2.67697431528342,1.79441524676228,50.4636393115467));
#24807=CARTESIAN_POINT('Ctrl Pts',(-2.62178396127082,1.87675023606295,50.4575399161952));
#24808=CARTESIAN_POINT('Ctrl Pts',(-2.56276760522076,1.9565721859484,50.4514405208437));
#24809=CARTESIAN_POINT('Ctrl Pts',(-2.50019191985115,2.03350877215002,50.4453411254922));
#24810=CARTESIAN_POINT('Ctrl Pts',(-2.43762003683202,2.11044068337501,50.4392421007645));
#24811=CARTESIAN_POINT('Ctrl Pts',(-2.3714895334439,2.18448723608768,50.4331430760367));
#24812=CARTESIAN_POINT('Ctrl Pts',(-2.30210770264219,2.25530877884505,50.427044051309));
#24813=CARTESIAN_POINT('Ctrl Pts',(-2.23271076539457,2.32614574151556,50.4209436986459));
#24814=CARTESIAN_POINT('Ctrl Pts',(-2.16006140450322,2.39375598379192,50.4148433459829));
#24815=CARTESIAN_POINT('Ctrl Pts',(-2.08450332668258,2.45783714748339,50.4087429933198));
#24816=CARTESIAN_POINT('Ctrl Pts',(-2.00885443188885,2.52199533347991,50.4026353083426));
#24817=CARTESIAN_POINT('Ctrl Pts',(-1.93029017833084,2.58261568575184,50.3965276233653));
#24818=CARTESIAN_POINT('Ctrl Pts',(-1.84918674915733,2.63943666892028,50.3904199383881));
#24819=CARTESIAN_POINT('Ctrl Pts',(-1.768032317762,2.69629338419545,50.3843084125683));
#24820=CARTESIAN_POINT('Ctrl Pts',(-1.68433590672813,2.74934573955533,50.3781968867485));
#24821=CARTESIAN_POINT('Ctrl Pts',(-1.59850005921721,2.79837723032164,50.3720853609287));
#24822=CARTESIAN_POINT('Ctrl Pts',(-1.51250737215979,2.8474983115912,50.3659626681085));
#24823=CARTESIAN_POINT('Ctrl Pts',(-1.4243678359665,2.89258365598401,50.3598399752884));
#24824=CARTESIAN_POINT('Ctrl Pts',(-1.33450590411258,2.93346408779598,50.3537172824682));
#24825=CARTESIAN_POINT('Ctrl Pts',(-1.26468810812105,2.96522594278185,50.3489602857131));
#24826=CARTESIAN_POINT('Ctrl Pts',(-1.19383105609949,2.99445049063284,50.344203288958));
#24827=CARTESIAN_POINT('Ctrl Pts',(-1.12213954345542,3.02107934478949,50.3394462922029));
#24828=CARTESIAN_POINT('Ctrl Pts',(-1.0265657642302,3.05657894766191,50.3331046188182));
#24829=CARTESIAN_POINT('Ctrl Pts',(-0.929169554246279,3.08758984486248,
50.3267629454334));
#24830=CARTESIAN_POINT('Ctrl Pts',(-0.830398224371547,3.11392940694882,
50.3204212720487));
#24831=CARTESIAN_POINT('Ctrl Pts',(-0.731773318293886,3.14022992188757,
50.314088999893));
#24832=CARTESIAN_POINT('Ctrl Pts',(-0.631777738060152,3.16187277887449,
50.3077567277373));
#24833=CARTESIAN_POINT('Ctrl Pts',(-0.530876565142943,3.1787242150086,50.3014244555816));
#24834=CARTESIAN_POINT('Ctrl Pts',(-0.424986417318397,3.19640885644247,
50.2947790894749));
#24835=CARTESIAN_POINT('Ctrl Pts',(-0.31809923935474,3.20881592952247,50.2881337233682));
#24836=CARTESIAN_POINT('Ctrl Pts',(-0.210769145412158,3.21585042093724,
50.2814883572615));
#24837=CARTESIAN_POINT('Ctrl Pts',(-0.108748201975073,3.22253694681617,
50.2751717083629));
#24838=CARTESIAN_POINT('Ctrl Pts',(-0.00632757651942337,3.22436963666028,
50.2688550594643));
#24839=CARTESIAN_POINT('Ctrl Pts',(0.0960087647114913,3.22131958669092,
50.2625384105657));
#24840=CARTESIAN_POINT('Ctrl Pts',(0.198275729533058,3.21827160442804,50.2562260438841));
#24841=CARTESIAN_POINT('Ctrl Pts',(0.300458119624661,3.21034748182014,50.2499136772025));
#24842=CARTESIAN_POINT('Ctrl Pts',(0.402071203165288,3.19757037609576,50.2436013105208));
#24843=CARTESIAN_POINT('Ctrl Pts',(0.503636990654584,3.18479921750562,50.2372918819453));
#24844=CARTESIAN_POINT('Ctrl Pts',(0.604633597356732,3.16717962291273,50.2309824533698));
#24845=CARTESIAN_POINT('Ctrl Pts',(0.704581288421044,3.14478660174374,50.2246730247942));
#24846=CARTESIAN_POINT('Ctrl Pts',(0.804503681232043,3.12239924858284,50.2183651932293));
#24847=CARTESIAN_POINT('Ctrl Pts',(0.903377291858967,3.09524096409745,50.2120573616644));
#24848=CARTESIAN_POINT('Ctrl Pts',(1.00073308481727,3.06343775119588,50.2057495300994));
#24849=CARTESIAN_POINT('Ctrl Pts',(1.09811106106199,3.03162729168104,50.1994402612452));
#24850=CARTESIAN_POINT('Ctrl Pts',(1.19397014176976,2.99516991119222,50.1931309923911));
#24851=CARTESIAN_POINT('Ctrl Pts',(1.28785719676933,2.95424125677464,50.1868217235369));
#24852=CARTESIAN_POINT('Ctrl Pts',(1.38175496784341,2.913307930845,50.1805117345558));
#24853=CARTESIAN_POINT('Ctrl Pts',(1.47367989593232,2.86790248302421,50.1742017455747));
#24854=CARTESIAN_POINT('Ctrl Pts',(1.56320057919852,2.81824795071218,50.1678917565936));
#24855=CARTESIAN_POINT('Ctrl Pts',(1.65278085478603,2.76856036426409,50.1615775671654));
#24856=CARTESIAN_POINT('Ctrl Pts',(1.73995333823911,2.71461824789198,50.1552633777373));
#24857=CARTESIAN_POINT('Ctrl Pts',(1.82431303210882,2.65668957979247,50.1489491883091));
#24858=CARTESIAN_POINT('Ctrl Pts',(1.85554735742454,2.63524138834548,50.1466113485463));
#24859=CARTESIAN_POINT('Ctrl Pts',(1.88639638224608,2.61324711681045,50.1442735087836));
#24860=CARTESIAN_POINT('Ctrl Pts',(1.91684063918178,2.59072181572649,50.1419356690208));
#24861=CARTESIAN_POINT('Ctrl Pts',(-3.22274870145484,0.00289305568448681,
50.5817658723809));
#24862=CARTESIAN_POINT('Ctrl Pts',(-3.22294593790816,-0.216820490517224,
50.5940710088782));
#24863=CARTESIAN_POINT('Ctrl Pts',(-3.20067541107489,-0.435964380627837,
50.6063421177884));
#24864=CARTESIAN_POINT('Ctrl Pts',(-3.14577957458053,-0.702062716046087,
50.622387585657));
#24865=CARTESIAN_POINT('Ctrl Pts',(-3.13404357799902,-0.752722786275725,
50.6254923413925));
#24866=CARTESIAN_POINT('Ctrl Pts',(-3.1121464086732,-0.837824431242347,
50.6308043780983));
#24867=CARTESIAN_POINT('Ctrl Pts',(-3.1026256862327,-0.872421193767486,
50.6329912168688));
#24868=CARTESIAN_POINT('Ctrl Pts',(-3.08336780646881,-0.938094142503432,
50.6371977604574));
#24869=CARTESIAN_POINT('Ctrl Pts',(-3.07373335171097,-0.969195961374662,
50.6392139493982));
#24870=CARTESIAN_POINT('Ctrl Pts',(-3.04697821554796,-1.05115185498848,
50.6445928861539));
#24871=CARTESIAN_POINT('Ctrl Pts',(-3.02905646767004,-1.10173174930548,
50.6479808315215));
#24872=CARTESIAN_POINT('Ctrl Pts',(-2.92568908737845,-1.37184214798474,
50.6664531184552));
#24873=CARTESIAN_POINT('Ctrl Pts',(-2.81764048990057,-1.58192199893996,
50.682265881946));
#24874=CARTESIAN_POINT('Ctrl Pts',(-2.63213206238254,-1.86229357301267,
50.7048793763472));
#24875=CARTESIAN_POINT('Ctrl Pts',(-2.57266218212015,-1.94362229042128,
50.7116337837267));
#24876=CARTESIAN_POINT('Ctrl Pts',(-2.48233007528408,-2.05573037319448,
50.7211120505662));
#24877=CARTESIAN_POINT('Ctrl Pts',(-2.45450345960228,-2.08887602857737,
50.7239365132111));
#24878=CARTESIAN_POINT('Ctrl Pts',(-2.40331016691311,-2.14741883010464,
50.7289513877557));
#24879=CARTESIAN_POINT('Ctrl Pts',(-2.38018727660624,-2.17302004890099,
50.7311538498141));
#24880=CARTESIAN_POINT('Ctrl Pts',(-2.34225760734563,-2.21368301599351,
50.7346605935914));
#24881=CARTESIAN_POINT('Ctrl Pts',(-2.32770663230663,-2.22897848471628,
50.7359816691638));
#24882=CARTESIAN_POINT('Ctrl Pts',(-2.29807837871757,-2.25951607225457,
50.7386212568842));
#24883=CARTESIAN_POINT('Ctrl Pts',(-2.28299724290356,-2.2747528999986,50.7399392973703));
#24884=CARTESIAN_POINT('Ctrl Pts',(-2.24153356794207,-2.31581687015043,
50.7434980565896));
#24885=CARTESIAN_POINT('Ctrl Pts',(-2.2148566712145,-2.34134377961174,50.7457175606291));
#24886=CARTESIAN_POINT('Ctrl Pts',(-2.05150091703217,-2.49236629606847,
50.7589359388627));
#24887=CARTESIAN_POINT('Ctrl Pts',(-1.90461716824201,-2.60633731052415,
50.7692977867751));
#24888=CARTESIAN_POINT('Ctrl Pts',(-1.57824147938978,-2.81717334016311,
50.7910864900979));
#24889=CARTESIAN_POINT('Ctrl Pts',(-1.39775205847823,-2.91094318019762,
50.8024888642781));
#24890=CARTESIAN_POINT('Ctrl Pts',(-1.16193759080524,-3.00643787871655,
50.8175239224694));
#24891=CARTESIAN_POINT('Ctrl Pts',(-1.11376821521377,-3.02461363007976,
50.8205995517256));
#24892=CARTESIAN_POINT('Ctrl Pts',(-1.03159753188286,-3.05339002568585,
50.8258651688267));
#24893=CARTESIAN_POINT('Ctrl Pts',(-0.997817527671875,-3.06459526573084,
50.8280351190038));
#24894=CARTESIAN_POINT('Ctrl Pts',(-0.92889730297866,-3.08619666055815,
50.8324763958555));
#24895=CARTESIAN_POINT('Ctrl Pts',(-0.893751576129889,-3.09655743895753,
50.8347484926124));
#24896=CARTESIAN_POINT('Ctrl Pts',(-0.803271344232077,-3.12156186672095,
50.8406195768897));
#24897=CARTESIAN_POINT('Ctrl Pts',(-0.74771139666121,-3.13533416857717,
50.8442455191745));
#24898=CARTESIAN_POINT('Ctrl Pts',(-0.625114591955927,-3.16227978483002,
50.8522958948133));
#24899=CARTESIAN_POINT('Ctrl Pts',(-0.558001847543211,-3.17480783705022,
50.8567349905582));
#24900=CARTESIAN_POINT('Ctrl Pts',(-0.490581718709063,-3.18519185289811,
50.8612231915357));
#24901=CARTESIAN_POINT('Ctrl Pts',(0.500000469481149,-0.249903141644244,
19.1419331299125));
#24902=CARTESIAN_POINT('Ctrl Pts',(0.499985698745681,-0.249901829979438,
19.1419329611828));
#24903=CARTESIAN_POINT('Ctrl Pts',(0.499943925319444,-0.225581315070387,
19.1419270874343));
#24904=CARTESIAN_POINT('Ctrl Pts',(0.499905220847302,-0.0968326406578691,
19.1419269431202));
#24905=CARTESIAN_POINT('Ctrl Pts',(0.499905354496604,0.0576085255888102,
19.1419269231968));
#24906=CARTESIAN_POINT('Ctrl Pts',(0.499924487070724,0.161824164743378,
19.1419270312494));
#24907=CARTESIAN_POINT('Ctrl Pts',(0.499957970023252,0.233166151920814,
19.1419290385144));
#24908=CARTESIAN_POINT('Ctrl Pts',(0.499985738380631,0.249901825150789,
19.1419329686928));
#24909=CARTESIAN_POINT('Ctrl Pts',(0.500000469481149,0.249903141644244,
19.1419331299125));
#24910=CARTESIAN_POINT('Ctrl Pts',(0.50000579870514,-1.07273214192946,19.141904307727));
#24911=CARTESIAN_POINT('Ctrl Pts',(0.617766930419002,-1.05838545165019,
19.1642183664756));
#24912=CARTESIAN_POINT('Ctrl Pts',(0.961751310472008,-0.926346421353011,
19.2125872476967));
#24913=CARTESIAN_POINT('Ctrl Pts',(1.28046455179809,-0.399644119496195,
19.2137755873294));
#24914=CARTESIAN_POINT('Ctrl Pts',(1.27936400811516,0.237312123921118,19.2139396493409));
#24915=CARTESIAN_POINT('Ctrl Pts',(1.12181620701011,0.66571216146587,19.2130498921711));
#24916=CARTESIAN_POINT('Ctrl Pts',(0.846099822863789,0.968022143869402,
19.1965205779324));
#24917=CARTESIAN_POINT('Ctrl Pts',(0.617440555450805,1.05842521350129,19.1641565230633));
#24918=CARTESIAN_POINT('Ctrl Pts',(0.500005798705135,1.07273214192946,19.141904307727));
#24919=CARTESIAN_POINT('Ctrl Pts',(0.374651423361831,-2.49809918431546,
19.8198617495831));
#24920=CARTESIAN_POINT('Ctrl Pts',(0.709304215540434,-2.46080219696565,
19.8562164416348));
#24921=CARTESIAN_POINT('Ctrl Pts',(1.68368133342979,-2.14239899065394,19.9350988623808));
#24922=CARTESIAN_POINT('Ctrl Pts',(2.57589462505932,-0.923785761636194,
19.9392568404695));
#24923=CARTESIAN_POINT('Ctrl Pts',(2.57299273739104,0.549303191743538,19.9396328253395));
#24924=CARTESIAN_POINT('Ctrl Pts',(2.13168844086288,1.54026272327316,19.9369090432763));
#24925=CARTESIAN_POINT('Ctrl Pts',(1.35624450163379,2.24246685246118,19.9089996947345));
#24926=CARTESIAN_POINT('Ctrl Pts',(0.708376725350636,2.46090556556345,19.8561156846084));
#24927=CARTESIAN_POINT('Ctrl Pts',(0.374651423361818,2.49809918431547,19.8198617495831));
#24928=CARTESIAN_POINT('Ctrl Pts',(0.11219973762821,-3.,21.2392862649499));
#24929=CARTESIAN_POINT('Ctrl Pts',(0.545410746577862,-2.98330036684517,
21.254809362827));
#24930=CARTESIAN_POINT('Ctrl Pts',(1.84334280227898,-2.65791740981921,21.2909019746354));
#24931=CARTESIAN_POINT('Ctrl Pts',(3.03119172810009,-1.14304804845867,21.2989264987267));
#24932=CARTESIAN_POINT('Ctrl Pts',(3.02359011539719,0.679678385818526,21.298996417349));
#24933=CARTESIAN_POINT('Ctrl Pts',(2.443255756993,1.90810517204302,21.2948760084178));
#24934=CARTESIAN_POINT('Ctrl Pts',(1.40427963606369,2.75990594888198,21.2788873186408));
#24935=CARTESIAN_POINT('Ctrl Pts',(0.54421010229727,2.98334664987728,21.2547663405623));
#24936=CARTESIAN_POINT('Ctrl Pts',(0.112199737628194,3.,21.2392862649499));
#24937=CARTESIAN_POINT('Ctrl Pts',(1.76595225516049E-15,-3.,21.846099125618));
#24938=CARTESIAN_POINT('Ctrl Pts',(0.443076107560806,-3.,21.8529261923905));
#24939=CARTESIAN_POINT('Ctrl Pts',(1.79348225283645,-2.70799686462405,21.8711225067259));
#24940=CARTESIAN_POINT('Ctrl Pts',(3.03256681393803,-1.16243291399857,21.8807881756829));
#24941=CARTESIAN_POINT('Ctrl Pts',(3.02252392263477,0.691564152912778,21.8807213059649));
#24942=CARTESIAN_POINT('Ctrl Pts',(2.42127463370821,1.94262419136537,21.876015661462));
#24943=CARTESIAN_POINT('Ctrl Pts',(1.33503220965341,2.79906458058143,21.8649899286495));
#24944=CARTESIAN_POINT('Ctrl Pts',(0.441848122160112,3.,21.8529072711754));
#24945=CARTESIAN_POINT('Ctrl Pts',(-1.48930058907191E-14,3.,21.846099125618));
#24946=CARTESIAN_POINT('',(0.500000234886957,0.250003172331033,19.141934398682));
#24947=CARTESIAN_POINT('',(0.499951141785782,2.95746651812731,21.8534599521462));
#24948=CARTESIAN_POINT('Ctrl Pts',(0.500000469773915,0.250006344662067,
19.1419331283439));
#24949=CARTESIAN_POINT('Ctrl Pts',(0.500000469773915,0.267897236481739,
19.141933220399));
#24950=CARTESIAN_POINT('Ctrl Pts',(0.5,0.285781329534287,19.142122715469));
#24951=CARTESIAN_POINT('Ctrl Pts',(0.5,0.647586433160097,19.1497655967622));
#24952=CARTESIAN_POINT('Ctrl Pts',(0.500000000105589,0.988807525496054,
19.2265788097412));
#24953=CARTESIAN_POINT('Ctrl Pts',(0.500000000105589,1.62419548103609,19.4977571124707));
#24954=CARTESIAN_POINT('Ctrl Pts',(0.500000000129562,1.9184510407218,19.6932861554111));
#24955=CARTESIAN_POINT('Ctrl Pts',(0.500000000129562,2.44456182345909,20.2134324331408));
#24956=CARTESIAN_POINT('Ctrl Pts',(0.499999999835962,2.62278482582048,20.5122279848983));
#24957=CARTESIAN_POINT('Ctrl Pts',(0.499999999835962,2.81085326210919,20.9561451281499));
#24958=CARTESIAN_POINT('Ctrl Pts',(0.499999999999019,2.86545844391283,21.1318314683005));
#24959=CARTESIAN_POINT('Ctrl Pts',(0.499999999999019,2.93869926777347,21.4893795880377));
#24960=CARTESIAN_POINT('Ctrl Pts',(0.499999999999999,2.95754601494669,21.6714083748326));
#24961=CARTESIAN_POINT('Ctrl Pts',(0.499999999999999,2.95745819674082,21.8534588950701));
#24962=CARTESIAN_POINT('',(0.500115911061517,-2.95873774531605,21.8534555877921));
#24963=CARTESIAN_POINT('Ctrl Pts',(0.499951141785782,2.95746651812731,21.8534599521462));
#24964=CARTESIAN_POINT('Ctrl Pts',(0.773041654135478,2.91095214720846,21.8573003801108));
#24965=CARTESIAN_POINT('Ctrl Pts',(1.47173378593617,2.69128316033362,21.8663774964905));
#24966=CARTESIAN_POINT('Ctrl Pts',(2.42127463370821,1.94262419136537,21.876015661462));
#24967=CARTESIAN_POINT('Ctrl Pts',(3.02252392263477,0.691564152912778,21.8807213059649));
#24968=CARTESIAN_POINT('Ctrl Pts',(3.03256681393803,-1.16243291399857,21.8807881756829));
#24969=CARTESIAN_POINT('Ctrl Pts',(1.91000174505638,-2.56265704491053,21.8720314348768));
#24970=CARTESIAN_POINT('Ctrl Pts',(0.775090389504859,-2.91314338265178,
21.8573170895367));
#24971=CARTESIAN_POINT('Ctrl Pts',(0.500115911061517,-2.95873774531605,
21.8534555877921));
#24972=CARTESIAN_POINT('',(0.500000234886961,-0.250003167770416,19.141934398682));
#24973=CARTESIAN_POINT('Ctrl Pts',(0.500000000000001,-2.95875696259953,
21.8534539603318));
#24974=CARTESIAN_POINT('Ctrl Pts',(0.500000000000001,-2.95871463188845,
21.67146735895));
#24975=CARTESIAN_POINT('Ctrl Pts',(0.499999999998967,-2.93976167349618,
21.4895125652458));
#24976=CARTESIAN_POINT('Ctrl Pts',(0.499999999998967,-2.86636194368596,
21.132115489418));
#24977=CARTESIAN_POINT('Ctrl Pts',(0.499999999825066,-2.81170123842746,
20.9565020048332));
#24978=CARTESIAN_POINT('Ctrl Pts',(0.499999999825066,-2.6234386591811,20.5124823848305));
#24979=CARTESIAN_POINT('Ctrl Pts',(0.50000000005703,-2.44498892439426,20.2134765044685));
#24980=CARTESIAN_POINT('Ctrl Pts',(0.500000000057029,-1.91831791688,19.6930503466231));
#24981=CARTESIAN_POINT('Ctrl Pts',(0.500000000109665,-1.62378550938661,
19.4974427643328));
#24982=CARTESIAN_POINT('Ctrl Pts',(0.500000000109665,-0.988277937574047,
19.2264560225243));
#24983=CARTESIAN_POINT('Ctrl Pts',(0.5,-0.647284047492248,19.1497487087651));
#24984=CARTESIAN_POINT('Ctrl Pts',(0.5,-0.285729480193629,19.1421221661827));
#24985=CARTESIAN_POINT('Ctrl Pts',(0.500000469773922,-0.267871311676459,
19.1419332201691));
#24986=CARTESIAN_POINT('Ctrl Pts',(0.500000469773922,-0.250006335540832,
19.1419331283438));
#24987=CARTESIAN_POINT('',(0.5,1.66533453693774E-16,19.1419356690201));
#24988=CARTESIAN_POINT('Origin',(0.5,2.22044604925031E-16,0.));
#24989=CARTESIAN_POINT('',(0.500000000000001,-2.95803989154981,24.3207730140306));
#24990=CARTESIAN_POINT('',(0.500000000000001,-2.95803989154981,39.1419356690201));
#24991=CARTESIAN_POINT('',(0.499999999999999,2.95803989154981,24.3207730140306));
#24992=CARTESIAN_POINT('Origin',(0.5,2.22044604925031E-16,0.));
#24993=CARTESIAN_POINT('',(0.499999999999999,2.95803989154981,39.1419356690201));
#24994=CARTESIAN_POINT('Origin',(-9.07107736682793E-15,0.,39.1419356690201));
#24995=CARTESIAN_POINT('',(-0.499940024180695,-2.95805002868819,21.8534578776881));
#24996=CARTESIAN_POINT('',(-2.99999997692161,-0.000372116104727271,21.880545165042));
#24997=CARTESIAN_POINT('Ctrl Pts',(-0.499940024180695,-2.95805002868819,
21.8534578776881));
#24998=CARTESIAN_POINT('Ctrl Pts',(-0.59094175739541,-2.94266982610114,
21.8547370166103));
#24999=CARTESIAN_POINT('Ctrl Pts',(-0.68138174282413,-2.92306085113225,
21.8559764996555));
#25000=CARTESIAN_POINT('Ctrl Pts',(-0.770826195716954,-2.89928042382874,
21.8571725494205));
#25001=CARTESIAN_POINT('Ctrl Pts',(-0.860457040630935,-2.87545044083154,
21.8583710916166));
#25002=CARTESIAN_POINT('Ctrl Pts',(-0.949087732495046,-2.84743164098335,
21.8595260193239));
#25003=CARTESIAN_POINT('Ctrl Pts',(-1.03628975548556,-2.81533364677718,
21.860633531475));
#25004=CARTESIAN_POINT('Ctrl Pts',(-1.12349177847607,-2.78323565257101,
21.8617410436262));
#25005=CARTESIAN_POINT('Ctrl Pts',(-1.20926467836655,-2.74705858859954,
21.8628011402213));
#25006=CARTESIAN_POINT('Ctrl Pts',(-1.29319483960894,-2.70696270879538,
21.8638100201928));
#25007=CARTESIAN_POINT('Ctrl Pts',(-1.38514368549922,-2.66303607004747,
21.8649152885213));
#25008=CARTESIAN_POINT('Ctrl Pts',(-1.47489907524035,-2.61439837108066,
21.8659590862581));
#25009=CARTESIAN_POINT('Ctrl Pts',(-1.56199166539876,-2.56128523152437,
21.8669430860832));
#25010=CARTESIAN_POINT('Ctrl Pts',(-1.64895250576959,-2.50825243915768,
21.8679255973573));
#25011=CARTESIAN_POINT('Ctrl Pts',(-1.73325829906695,-2.45075788734509,
21.8688484915021));
#25012=CARTESIAN_POINT('Ctrl Pts',(-1.81446583003367,-2.38908219859432,
21.8697134336183));
#25013=CARTESIAN_POINT('Ctrl Pts',(-1.89558530704206,-2.32747338527323,
21.8705774378709));
#25014=CARTESIAN_POINT('Ctrl Pts',(-1.97361295219982,-2.26169267203088,
21.8713836157024));
#25015=CARTESIAN_POINT('Ctrl Pts',(-2.04813532502368,-2.19206334087092,
21.8721336268026));
#25016=CARTESIAN_POINT('Ctrl Pts',(-2.12254248874703,-2.1225416543324,21.8728824784107));
#25017=CARTESIAN_POINT('Ctrl Pts',(-2.1934549447046,-2.0491834436902,21.8735753368172));
#25018=CARTESIAN_POINT('Ctrl Pts',(-2.2604935455019,-1.97235111751034,21.8742138540263));
#25019=CARTESIAN_POINT('Ctrl Pts',(-2.28764065829647,-1.94123806025276,
21.8744724199643));
#25020=CARTESIAN_POINT('Ctrl Pts',(-2.31415291921105,-1.90955575635341,
21.8747220748988));
#25021=CARTESIAN_POINT('Ctrl Pts',(-2.34000681387336,-1.87733004850673,
21.8749629285299));
#25022=CARTESIAN_POINT('Ctrl Pts',(-2.39854704458456,-1.80436230431125,
21.8755082864853));
#25023=CARTESIAN_POINT('Ctrl Pts',(-2.45373755903258,-1.72857059033661,
21.8760085208243));
#25024=CARTESIAN_POINT('Ctrl Pts',(-2.50529548516313,-1.65030134582181,
21.8764659088202));
#25025=CARTESIAN_POINT('Ctrl Pts',(-2.55682438665815,-1.57207616313154,
21.8769230393287));
#25026=CARTESIAN_POINT('Ctrl Pts',(-2.60472450989376,-1.49137659468018,
21.8773373717214));
#25027=CARTESIAN_POINT('Ctrl Pts',(-2.64875480042251,-1.40858013873501,
21.8777111794279));
#25028=CARTESIAN_POINT('Ctrl Pts',(-2.6927693533044,-1.32581327653925,21.8780848535252));
#25029=CARTESIAN_POINT('Ctrl Pts',(-2.73291661193963,-1.24095141659554,
21.8784180319004));
#25030=CARTESIAN_POINT('Ctrl Pts',(-2.76900090393528,-1.15439767584903,
21.8787129855462));
#25031=CARTESIAN_POINT('Ctrl Pts',(-2.80509635843587,-1.06781716011249,
21.8790080304346));
#25032=CARTESIAN_POINT('Ctrl Pts',(-2.83712615654066,-0.979544134173076,
21.8792648269406));
#25033=CARTESIAN_POINT('Ctrl Pts',(-2.86494263903965,-0.890002064611414,
21.8794856481653));
#25034=CARTESIAN_POINT('Ctrl Pts',(-2.88763543272642,-0.816953298976749,
21.8796657949719));
#25035=CARTESIAN_POINT('Ctrl Pts',(-2.90752498795916,-0.743060415173017,
21.8798219989361));
#25036=CARTESIAN_POINT('Ctrl Pts',(-2.92455591077185,-0.668560187843599,
21.8799554942307));
#25037=CARTESIAN_POINT('Ctrl Pts',(-2.94760321776225,-0.567741833547698,
21.8801361483897));
#25038=CARTESIAN_POINT('Ctrl Pts',(-2.96542055692276,-0.465785336223467,
21.8802752157295));
#25039=CARTESIAN_POINT('Ctrl Pts',(-2.9779300558943,-0.363225249950262,
21.8803728029858));
#25040=CARTESIAN_POINT('Ctrl Pts',(-2.99045336542708,-0.260551936731979,
21.880470497979));
#25041=CARTESIAN_POINT('Ctrl Pts',(-2.99765709289031,-0.157274008900583,
21.8805266212497));
#25042=CARTESIAN_POINT('Ctrl Pts',(-2.99951519597997,-0.0539313367649988,
21.8805412798873));
#25043=CARTESIAN_POINT('Ctrl Pts',(-2.99983617653992,-0.0360792655033546,
21.8805438121137));
#25044=CARTESIAN_POINT('Ctrl Pts',(-2.99999776244028,-0.0182252642061044,
21.8805451069813));
#25045=CARTESIAN_POINT('Ctrl Pts',(-2.99999997692161,-0.000372116104727271,
21.880545165042));
#25046=CARTESIAN_POINT('',(-0.499999999999999,-2.95803989154981,24.3207730140306));
#25047=CARTESIAN_POINT('',(-0.499999999999999,-2.95803989154981,39.1419356690201));
#25048=CARTESIAN_POINT('Ctrl Pts',(-0.499999999999998,-2.95803989154981,
24.3207730140306));
#25049=CARTESIAN_POINT('Ctrl Pts',(-0.331796881873697,-2.98647140773842,
24.3173150006272));
#25050=CARTESIAN_POINT('Ctrl Pts',(-0.163503365753256,-3.,24.3156328315757));
#25051=CARTESIAN_POINT('Ctrl Pts',(0.163503365753248,-3.,24.3156328315757));
#25052=CARTESIAN_POINT('Ctrl Pts',(0.331796881873693,-2.98647140773842,
24.3173150006272));
#25053=CARTESIAN_POINT('Ctrl Pts',(0.5,-2.95803989154981,24.3207730140306));
#25054=CARTESIAN_POINT('',(-0.500000000000001,2.95803989154981,24.3207730140306));
#25055=CARTESIAN_POINT('Ctrl Pts',(0.499999999999998,2.95803989154981,24.3207730140306));
#25056=CARTESIAN_POINT('Ctrl Pts',(0.331796881873692,2.98647140773842,24.3173150006272));
#25057=CARTESIAN_POINT('Ctrl Pts',(0.163503365753246,3.,24.3156328315757));
#25058=CARTESIAN_POINT('Ctrl Pts',(-7.97972798949331E-15,3.,24.3156328315757));
#25059=CARTESIAN_POINT('Ctrl Pts',(-0.163503365753258,3.,24.3156328315757));
#25060=CARTESIAN_POINT('Ctrl Pts',(-0.331796881873699,2.98647140773842,
24.3173150006272));
#25061=CARTESIAN_POINT('Ctrl Pts',(-0.500000000000002,2.95803989154981,
24.3207730140306));
#25062=CARTESIAN_POINT('',(-0.500010187139659,2.95803816959088,21.8534623270851));
#25063=CARTESIAN_POINT('',(-0.500000000000001,2.95803989154981,39.1419356690201));
#25064=CARTESIAN_POINT('Ctrl Pts',(-2.9999999769217,-0.000372115392980615,
21.880545165042));
#25065=CARTESIAN_POINT('Ctrl Pts',(-3.00001277286105,0.102788942964087,
21.8805455005347));
#25066=CARTESIAN_POINT('Ctrl Pts',(-2.99470013233285,0.205905330647462,
21.8805045404221));
#25067=CARTESIAN_POINT('Ctrl Pts',(-2.98410189910898,0.308441008515781,
21.8804223912109));
#25068=CARTESIAN_POINT('Ctrl Pts',(-2.97349464501599,0.411063961395882,
21.8803401720769));
#25069=CARTESIAN_POINT('Ctrl Pts',(-2.95759284574052,0.513104906228459,
21.8802166936969));
#25070=CARTESIAN_POINT('Ctrl Pts',(-2.93648808754871,0.61403396623034,21.8800520628496));
#25071=CARTESIAN_POINT('Ctrl Pts',(-2.93249958683041,0.633108130674964,
21.8800209499486));
#25072=CARTESIAN_POINT('Ctrl Pts',(-2.92832540577109,0.65214261275552,21.8799883672603));
#25073=CARTESIAN_POINT('Ctrl Pts',(-2.92396636693129,0.671133880127263,
21.8799543155056));
#25074=CARTESIAN_POINT('Ctrl Pts',(-2.90131348256699,0.769826963514177,
21.8797773566643));
#25075=CARTESIAN_POINT('Ctrl Pts',(-2.87365814172373,0.867378355378354,
21.8795607237316));
#25076=CARTESIAN_POINT('Ctrl Pts',(-2.84113958094458,0.963289095541988,
21.879301307984));
#25077=CARTESIAN_POINT('Ctrl Pts',(-2.80862422134745,1.05919039409045,21.8790419177738));
#25078=CARTESIAN_POINT('Ctrl Pts',(-2.77124670666013,1.15345103353225,21.8787397531715));
#25079=CARTESIAN_POINT('Ctrl Pts',(-2.72919572627057,1.24558849051623,21.878391706372));
#25080=CARTESIAN_POINT('Ctrl Pts',(-2.68715425179392,1.33770511919527,21.8780437382508));
#25081=CARTESIAN_POINT('Ctrl Pts',(-2.6404415648864,1.42769920755386,21.8776499086739));
#25082=CARTESIAN_POINT('Ctrl Pts',(-2.58929383883054,1.51510970434297,21.8772071119431));
#25083=CARTESIAN_POINT('Ctrl Pts',(-2.5381556180301,1.60250395683029,21.8767643975013));
#25084=CARTESIAN_POINT('Ctrl Pts',(-2.48258417734381,1.68731527556145,21.8762727341039));
#25085=CARTESIAN_POINT('Ctrl Pts',(-2.42286082065673,1.76910865797627,21.875729017784));
#25086=CARTESIAN_POINT('Ctrl Pts',(-2.39643455500711,1.80530042233742,21.8754884353267));
#25087=CARTESIAN_POINT('Ctrl Pts',(-2.36919597786386,1.84090168069933,21.8752376615998));
#25088=CARTESIAN_POINT('Ctrl Pts',(-2.34117214558247,1.8758765910232,21.8749764277025));
#25089=CARTESIAN_POINT('Ctrl Pts',(-2.282548149704,1.94904178049793,21.8744299437397));
#25090=CARTESIAN_POINT('Ctrl Pts',(-2.22046648084456,2.01948669411621,21.8738376841246));
#25091=CARTESIAN_POINT('Ctrl Pts',(-2.15521897788651,2.08687114057333,21.8731985334558));
#25092=CARTESIAN_POINT('Ctrl Pts',(-2.08994940172927,2.15427838315662,21.8725591665625));
#25093=CARTESIAN_POINT('Ctrl Pts',(-2.0215121604408,2.21862275891459,21.8718728768836));
#25094=CARTESIAN_POINT('Ctrl Pts',(-1.95023698961227,2.27959989567207,21.8711385478849));
#25095=CARTESIAN_POINT('Ctrl Pts',(-1.87895152209695,2.34058584142251,21.8704041128022));
#25096=CARTESIAN_POINT('Ctrl Pts',(-1.80482766067384,2.39820329494175,21.8696216245189));
#25097=CARTESIAN_POINT('Ctrl Pts',(-1.72822787640916,2.45218849340794,21.8687899660169));
#25098=CARTESIAN_POINT('Ctrl Pts',(-1.65154355910333,2.5062332681908,21.8679573897236));
#25099=CARTESIAN_POINT('Ctrl Pts',(-1.57237823920555,2.55663753166712,21.8670755346263));
#25100=CARTESIAN_POINT('Ctrl Pts',(-1.49112266929207,2.60318135847722,21.8661432800049));
#25101=CARTESIAN_POINT('Ctrl Pts',(-1.42636912281268,2.64027269702651,21.8654003550212));
#25102=CARTESIAN_POINT('Ctrl Pts',(-1.36028872917732,2.67491323132945,21.8646254228678));
#25103=CARTESIAN_POINT('Ctrl Pts',(-1.29308896453722,2.70701328585437,21.8638179163547));
#25104=CARTESIAN_POINT('Ctrl Pts',(-1.20152769001504,2.75075037214142,21.862717669562));
#25105=CARTESIAN_POINT('Ctrl Pts',(-1.10785107791141,2.78978775972883,21.8615569494174));
#25106=CARTESIAN_POINT('Ctrl Pts',(-1.01255088571331,2.82395833960793,21.8603402470613));
#25107=CARTESIAN_POINT('Ctrl Pts',(-0.91698029339272,2.85822587342566,21.8591200924933));
#25108=CARTESIAN_POINT('Ctrl Pts',(-0.819777235734428,2.8875988784158,21.8578436375807));
#25109=CARTESIAN_POINT('Ctrl Pts',(-0.72144856800572,2.91196015833365,21.8565154118015));
#25110=CARTESIAN_POINT('Ctrl Pts',(-0.648189723848912,2.93011029959139,
21.8555258297436));
#25111=CARTESIAN_POINT('Ctrl Pts',(-0.574306323359667,2.94547956728581,
21.8545075104328));
#25112=CARTESIAN_POINT('Ctrl Pts',(-0.500010187139659,2.95803816959088,
21.8534623270851));
#25113=CARTESIAN_POINT('',(-3.00000000000001,-3.67394039744206E-16,50.1419356690201));
#25114=CARTESIAN_POINT('',(-3.00000000000001,3.67394039744206E-16,39.1419356690201));
#25115=CARTESIAN_POINT('Origin',(-1.041818884589E-14,0.,50.1419356690201));
#25116=CARTESIAN_POINT('Ctrl Pts',(-0.500000469469731,0.249901395376665,
19.1419331299742));
#25117=CARTESIAN_POINT('Ctrl Pts',(-0.499985448781684,0.249900114156667,
19.1419329138876));
#25118=CARTESIAN_POINT('Ctrl Pts',(-0.499957241892457,0.233340033373888,
19.1419289227389));
#25119=CARTESIAN_POINT('Ctrl Pts',(-0.499923116233831,0.161617725953644,
19.141926874418));
#25120=CARTESIAN_POINT('Ctrl Pts',(-0.499903664359004,0.0578516765404966,
19.1419267769168));
#25121=CARTESIAN_POINT('Ctrl Pts',(-0.499903654163716,-0.057515157620163,
19.141926775308));
#25122=CARTESIAN_POINT('Ctrl Pts',(-0.49992318239623,-0.161934834392146,
19.1419268788806));
#25123=CARTESIAN_POINT('Ctrl Pts',(-0.499957222592849,-0.233146393750517,
19.1419289247299));
#25124=CARTESIAN_POINT('Ctrl Pts',(-0.499985489109375,-0.249900109243623,
19.1419329215289));
#25125=CARTESIAN_POINT('Ctrl Pts',(-0.500000469469731,-0.249901395376665,
19.1419331299742));
#25126=CARTESIAN_POINT('Ctrl Pts',(-0.500005900053987,1.07273098952165,
19.1419037595993));
#25127=CARTESIAN_POINT('Ctrl Pts',(-0.617766856411166,1.05838431779768,
19.1642178069961));
#25128=CARTESIAN_POINT('Ctrl Pts',(-0.846046992725819,0.968758392758925,
19.1965193366959));
#25129=CARTESIAN_POINT('Ctrl Pts',(-1.12222824035265,0.664689422677935,
19.213096972248));
#25130=CARTESIAN_POINT('Ctrl Pts',(-1.27965361509687,0.238169805111735,
19.2138860499928));
#25131=CARTESIAN_POINT('Ctrl Pts',(-1.27973612410747,-0.237098012192637,
19.2138990693925));
#25132=CARTESIAN_POINT('Ctrl Pts',(-1.12169278387221,-0.666446671624522,
19.2130608557749));
#25133=CARTESIAN_POINT('Ctrl Pts',(-0.846203186258647,-0.968026539109895,
19.196503222222));
#25134=CARTESIAN_POINT('Ctrl Pts',(-0.61744048192897,-1.05842407959735,
19.1641559636152));
#25135=CARTESIAN_POINT('Ctrl Pts',(-0.500005900053987,-1.07273098952165,
19.1419037595993));
#25136=CARTESIAN_POINT('Ctrl Pts',(-0.374651529457775,2.49809898142235,
19.8198611757815));
#25137=CARTESIAN_POINT('Ctrl Pts',(-0.709304281794272,2.46080198574607,
19.8562158762544));
#25138=CARTESIAN_POINT('Ctrl Pts',(-1.35614981263617,2.24374050137417,19.9090264719253));
#25139=CARTESIAN_POINT('Ctrl Pts',(-2.13291772239582,1.53846891438119,19.9370353986983));
#25140=CARTESIAN_POINT('Ctrl Pts',(-2.57376446971679,0.551283320370357,
19.9395318251872));
#25141=CARTESIAN_POINT('Ctrl Pts',(-2.57408736573143,-0.547866663199184,
19.9396043925739));
#25142=CARTESIAN_POINT('Ctrl Pts',(-2.131400781918,-1.5414737450019,19.9369687673424));
#25143=CARTESIAN_POINT('Ctrl Pts',(-1.35656745347333,-2.24213214922828,
19.9089983547958));
#25144=CARTESIAN_POINT('Ctrl Pts',(-0.708376791714899,-2.46090535436693,
19.8561151192046));
#25145=CARTESIAN_POINT('Ctrl Pts',(-0.374651529457774,-2.49809898142235,
19.8198611757815));
#25146=CARTESIAN_POINT('Ctrl Pts',(-0.112199737628213,3.,21.2392862649499));
#25147=CARTESIAN_POINT('Ctrl Pts',(-0.545410746577865,2.98330036684518,
21.254809362827));
#25148=CARTESIAN_POINT('Ctrl Pts',(-1.40427372201026,2.76191164610531,21.2789029635529));
#25149=CARTESIAN_POINT('Ctrl Pts',(-2.44430047244797,1.90558668934363,21.2949283871888));
#25150=CARTESIAN_POINT('Ctrl Pts',(-3.02549086011703,0.682397094945288,
21.2989773348059));
#25151=CARTESIAN_POINT('Ctrl Pts',(-3.02590131894121,-0.678601175881948,
21.2990103838934));
#25152=CARTESIAN_POINT('Ctrl Pts',(-2.44234533102359,-1.90963444251436,
21.2948917804808));
#25153=CARTESIAN_POINT('Ctrl Pts',(-1.40492064000836,-2.75971763396258,
21.2788949026146));
#25154=CARTESIAN_POINT('Ctrl Pts',(-0.544210102297275,-2.98334664987728,
21.2547663405623));
#25155=CARTESIAN_POINT('Ctrl Pts',(-0.112199737628212,-3.,21.2392862649499));
#25156=CARTESIAN_POINT('Ctrl Pts',(-7.45975288878436E-15,3.,21.846099125618));
#25157=CARTESIAN_POINT('Ctrl Pts',(-0.443076107560811,3.,21.8529261923905));
#25158=CARTESIAN_POINT('Ctrl Pts',(-1.33511668480881,2.80117070574288,21.864996243952));
#25159=CARTESIAN_POINT('Ctrl Pts',(-2.42205080766271,1.94015854780963,21.8760313557109));
#25160=CARTESIAN_POINT('Ctrl Pts',(-3.02500193874651,0.694487451784985,
21.8807368994193));
#25161=CARTESIAN_POINT('Ctrl Pts',(-3.02547311532246,-0.690448134612415,
21.8807469396456));
#25162=CARTESIAN_POINT('Ctrl Pts',(-2.42004712161993,-1.94396598412946,
21.8760083073826));
#25163=CARTESIAN_POINT('Ctrl Pts',(-1.33584762052156,-2.79884623232731,
21.8649974020032));
#25164=CARTESIAN_POINT('Ctrl Pts',(-0.44184812216012,-3.,21.8529072711754));
#25165=CARTESIAN_POINT('Ctrl Pts',(-6.13614521966489E-15,-3.,21.846099125618));
#25166=CARTESIAN_POINT('',(-0.500000234886957,-0.25000317233103,19.141934398682));
#25167=CARTESIAN_POINT('Ctrl Pts',(-0.500000469773915,-0.250006344662061,
19.1419331283439));
#25168=CARTESIAN_POINT('Ctrl Pts',(-0.500000469773915,-0.267897236362903,
19.141933220399));
#25169=CARTESIAN_POINT('Ctrl Pts',(-0.5,-0.285781329331433,19.142122715467));
#25170=CARTESIAN_POINT('Ctrl Pts',(-0.5,-0.64758885702648,19.1497656467621));
#25171=CARTESIAN_POINT('Ctrl Pts',(-0.500000000107091,-0.988812928155548,
19.2265798854459));
#25172=CARTESIAN_POINT('Ctrl Pts',(-0.500000000107091,-1.62419910157496,
19.497759752549));
#25173=CARTESIAN_POINT('Ctrl Pts',(-0.500000000136194,-1.91845070856788,
19.6932873379294));
#25174=CARTESIAN_POINT('Ctrl Pts',(-0.500000000136194,-2.44455442803125,
20.2134309729014));
#25175=CARTESIAN_POINT('Ctrl Pts',(-0.499999999833597,-2.6227758687745,
20.5122259888824));
#25176=CARTESIAN_POINT('Ctrl Pts',(-0.499999999833597,-2.81084481109436,
20.956140074914));
#25177=CARTESIAN_POINT('Ctrl Pts',(-0.499999999999005,-2.86545145668325,
21.1318273751738));
#25178=CARTESIAN_POINT('Ctrl Pts',(-0.499999999999005,-2.93869500034237,
21.489376554184));
#25179=CARTESIAN_POINT('Ctrl Pts',(-0.499999999999999,-2.95754295724416,
21.6714024771996));
#25180=CARTESIAN_POINT('Ctrl Pts',(-0.499999999999999,-2.95745528673186,
21.8534537921611));
#25181=CARTESIAN_POINT('',(-0.500000234886961,0.250003167770442,19.141934398682));
#25182=CARTESIAN_POINT('Ctrl Pts',(-0.500000000000001,2.9579076296201,21.8534495050302));
#25183=CARTESIAN_POINT('Ctrl Pts',(-0.500000000000001,2.95794617404091,
21.6714260178936));
#25184=CARTESIAN_POINT('Ctrl Pts',(-0.499999999999072,2.93905792987264,
21.4894257571556));
#25185=CARTESIAN_POINT('Ctrl Pts',(-0.499999999999072,2.86575578974211,
21.131933596822));
#25186=CARTESIAN_POINT('Ctrl Pts',(-0.499999999845839,2.81112780850596,
20.9562698452876));
#25187=CARTESIAN_POINT('Ctrl Pts',(-0.499999999845839,2.62298756861714,
20.5123154976842));
#25188=CARTESIAN_POINT('Ctrl Pts',(-0.500000000065174,2.44468731250608,
20.2134475716897));
#25189=CARTESIAN_POINT('Ctrl Pts',(-0.500000000065174,1.91839767990519,
19.693207353235));
#25190=CARTESIAN_POINT('Ctrl Pts',(-0.500000000096103,1.6240521846631,19.4976513579156));
#25191=CARTESIAN_POINT('Ctrl Pts',(-0.500000000096103,0.988611016087444,
19.2265302537515));
#25192=CARTESIAN_POINT('Ctrl Pts',(-0.5,0.647449189595379,19.1497522054971));
#25193=CARTESIAN_POINT('Ctrl Pts',(-0.5,0.285729471252588,19.1421221660728));
#25194=CARTESIAN_POINT('Ctrl Pts',(-0.500000469773922,0.267871306763669,
19.141933220169));
#25195=CARTESIAN_POINT('Ctrl Pts',(-0.500000469773922,0.250006335540885,
19.1419331283438));
#25196=CARTESIAN_POINT('',(-0.5,-5.55111512312568E-17,19.1419356690201));
#25197=CARTESIAN_POINT('Origin',(-0.5,0.,0.));
#25198=CARTESIAN_POINT('Origin',(-0.5,0.,0.));
#25199=CARTESIAN_POINT('Origin',(-0.5,0.,0.));
#25200=CARTESIAN_POINT('Ctrl Pts',(-3.18327948107155,-0.464668609862618,
60.6133098318917));
#25201=CARTESIAN_POINT('Ctrl Pts',(-3.3370532982496,0.588781153171032,60.5474729574974));
#25202=CARTESIAN_POINT('Ctrl Pts',(-2.51393860486939,2.84257920150003,60.4157992087088));
#25203=CARTESIAN_POINT('Ctrl Pts',(1.01311494220538,3.66090406549081,60.2182885855259));
#25204=CARTESIAN_POINT('Ctrl Pts',(3.61694504820724,1.15041235324949,60.0207779623431));
#25205=CARTESIAN_POINT('Ctrl Pts',(2.94104075517665,-2.40027689070238,59.8232673391602));
#25206=CARTESIAN_POINT('Ctrl Pts',(-0.404228016077643,-3.77497842620744,
59.6257567159773));
#25207=CARTESIAN_POINT('Ctrl Pts',(-3.38226164936567,-1.7237444337863,59.4282460927945));
#25208=CARTESIAN_POINT('Ctrl Pts',(-3.29180676033138,1.89099555051049,59.2307354696115));
#25209=CARTESIAN_POINT('Ctrl Pts',(-0.214572769937683,3.79025880578182,
59.0332248464286));
#25210=CARTESIAN_POINT('Ctrl Pts',(3.05728290832011,2.25050459215375,58.8357142232458));
#25211=CARTESIAN_POINT('Ctrl Pts',(3.55529376345934,-1.33107756875446,58.6382036000628));
#25212=CARTESIAN_POINT('Ctrl Pts',(0.827568737366059,-3.70500041251386,
58.4406929768801));
#25213=CARTESIAN_POINT('Ctrl Pts',(-2.65100241828356,-2.71735937131622,
58.2431823536971));
#25214=CARTESIAN_POINT('Ctrl Pts',(-3.72432089987947,0.735736741130725,
58.0456717305143));
#25215=CARTESIAN_POINT('Ctrl Pts',(-1.4185583128274,3.52130193062268,57.8481611073313));
#25216=CARTESIAN_POINT('Ctrl Pts',(2.1742623397949,3.11198543505612,57.6506504841485));
#25217=CARTESIAN_POINT('Ctrl Pts',(3.79437361613089,-0.12083688877652,57.4531398609656));
#25218=CARTESIAN_POINT('Ctrl Pts',(1.97184661356077,-3.24402426334415,57.2556292377827));
#25219=CARTESIAN_POINT('Ctrl Pts',(-1.63973818462279,-3.42390575612951,
57.0581186145998));
#25220=CARTESIAN_POINT('Ctrl Pts',(-3.76358735442354,-0.497275092791353,
56.860607991417));
#25221=CARTESIAN_POINT('Ctrl Pts',(-2.47273085453206,2.88053369334928,56.6630973682341));
#25222=CARTESIAN_POINT('Ctrl Pts',(1.06163619548771,3.64483206301732,56.4655867450512));
#25223=CARTESIAN_POINT('Ctrl Pts',(3.63277993397126,1.10217157297284,56.2680761218683));
#25224=CARTESIAN_POINT('Ctrl Pts',(2.90789970035265,-2.44049002193061,56.0705654986855));
#25225=CARTESIAN_POINT('Ctrl Pts',(-0.45532011802947,-3.76889317954298,
55.8730548755026));
#25226=CARTESIAN_POINT('Ctrl Pts',(-3.40542765166225,-1.677776720555,55.6755442523197));
#25227=CARTESIAN_POINT('Ctrl Pts',(-3.26578811328327,1.93558782065046,55.4780336291368));
#25228=CARTESIAN_POINT('Ctrl Pts',(-0.16309656227425,3.79279207493464,55.2805230059539));
#25229=CARTESIAN_POINT('Ctrl Pts',(3.08757262307394,2.20879322526724,55.0830123827711));
#25230=CARTESIAN_POINT('Ctrl Pts',(3.53688484260436,-1.37924538021458,54.8855017595881));
#25231=CARTESIAN_POINT('Ctrl Pts',(0.777178784528909,-3.71589361410309,
54.6879911364054));
#25232=CARTESIAN_POINT('Ctrl Pts',(-2.68766217377324,-2.68110877522757,
54.4904805132223));
#25233=CARTESIAN_POINT('Ctrl Pts',(-3.71398521084471,0.786248073317566,
54.2929698900396));
#25234=CARTESIAN_POINT('Ctrl Pts',(-1.37060668705354,3.54024145318923,54.0954592668566));
#25235=CARTESIAN_POINT('Ctrl Pts',(2.21632434779813,3.08217109804834,53.8979486436738));
#25236=CARTESIAN_POINT('Ctrl Pts',(3.79238256933727,-0.17235541405342,53.7004380204909));
#25237=CARTESIAN_POINT('Ctrl Pts',(1.92760936000513,-3.27050372936606,53.502927397308));
#25238=CARTESIAN_POINT('Ctrl Pts',(-1.68608552885002,-3.40132154932197,
53.3054167741251));
#25239=CARTESIAN_POINT('Ctrl Pts',(-3.76999323703601,-0.446117768032975,
53.1079061509423));
#25240=CARTESIAN_POINT('Ctrl Pts',(-2.43338426356776,2.91384900077535,52.9103955277594));
#25241=CARTESIAN_POINT('Ctrl Pts',(1.11103811731961,3.63007837648053,52.7128849045765));
#25242=CARTESIAN_POINT('Ctrl Pts',(3.64741072255014,1.05273491233617,52.5153742813936));
#25243=CARTESIAN_POINT('Ctrl Pts',(2.87449292200031,-2.47975573659254,52.3178636582107));
#25244=CARTESIAN_POINT('Ctrl Pts',(-0.506470599677197,-3.76236212640368,
52.1203530350279));
#25245=CARTESIAN_POINT('Ctrl Pts',(-3.42788079845058,-1.63137455307642,
51.9228424118449));
#25246=CARTESIAN_POINT('Ctrl Pts',(-3.23923631769043,1.97976043160802,51.7253317886621));
#25247=CARTESIAN_POINT('Ctrl Pts',(-0.111502357959493,3.79465718393418,
51.5278211654792));
#25248=CARTESIAN_POINT('Ctrl Pts',(3.1171426479274,2.16665882183862,51.3303105422963));
#25249=CARTESIAN_POINT('Ctrl Pts',(3.51811058329886,-1.427151124091,51.1327999191135));
#25250=CARTESIAN_POINT('Ctrl Pts',(0.726079346912793,-3.72610502504112,
50.9352892959306));
#25251=CARTESIAN_POINT('Ctrl Pts',(-2.72269906505329,-2.64436190137017,
50.7377786727477));
#25252=CARTESIAN_POINT('Ctrl Pts',(-3.70522749830404,0.83660602953753,50.5402680495648));
#25253=CARTESIAN_POINT('Ctrl Pts',(-1.31715611094438,3.55923486122354,50.3427135111009));
#25254=CARTESIAN_POINT('Ctrl Pts',(1.05918636994692,3.21910041479783,50.2109958470314));
#25255=CARTESIAN_POINT('Ctrl Pts',(1.9151416701175,2.58484374727087,50.1451150573561));
#25256=CARTESIAN_POINT('Ctrl Pts',(-3.42030586252901,-0.49926774569958,
60.4750123196129));
#25257=CARTESIAN_POINT('Ctrl Pts',(-3.58552964872969,0.632621685250075,
60.4091754452186));
#25258=CARTESIAN_POINT('Ctrl Pts',(-2.70112599267545,3.05423710528894,60.2775016964301));
#25259=CARTESIAN_POINT('Ctrl Pts',(1.08855128707529,3.9334942821733,60.0799910732471));
#25260=CARTESIAN_POINT('Ctrl Pts',(3.88626208486859,1.2360718370919,59.8824804500643));
#25261=CARTESIAN_POINT('Ctrl Pts',(3.16003008742461,-2.57900104900582,59.6849698268814));
#25262=CARTESIAN_POINT('Ctrl Pts',(-0.434326756858761,-4.05606259797573,
59.4874592036985));
#25263=CARTESIAN_POINT('Ctrl Pts',(-3.63410420502517,-1.85209411471355,
59.2899485805156));
#25264=CARTESIAN_POINT('Ctrl Pts',(-3.53691406225007,2.03179871760746,59.0924379573328));
#25265=CARTESIAN_POINT('Ctrl Pts',(-0.230549817356877,4.07248075169131,
58.8949273341499));
#25266=CARTESIAN_POINT('Ctrl Pts',(3.28492760906342,2.41807673374656,58.697416710967));
#25267=CARTESIAN_POINT('Ctrl Pts',(3.82002025724725,-1.43018934999676,58.4999060877841));
#25268=CARTESIAN_POINT('Ctrl Pts',(0.889189347303573,-3.98087403476363,
58.3023954646013));
#25269=CARTESIAN_POINT('Ctrl Pts',(-2.84839555142724,-2.91969343049402,
58.1048848414183));
#25270=CARTESIAN_POINT('Ctrl Pts',(-4.00163312192405,0.790519558188566,
57.9073742182355));
#25271=CARTESIAN_POINT('Ctrl Pts',(-1.52418389354541,3.78349739903745,57.7098635950526));
#25272=CARTESIAN_POINT('Ctrl Pts',(2.33615749785601,3.34370327548005,57.5123529718697));
#25273=CARTESIAN_POINT('Ctrl Pts',(4.07690195003213,-0.129834380408526,
57.3148423486869));
#25274=CARTESIAN_POINT('Ctrl Pts',(2.11866993535222,-3.48557368967409,57.117331725504));
#25275=CARTESIAN_POINT('Ctrl Pts',(-1.76183277630091,-3.6788491240155,56.9198211023211));
#25276=CARTESIAN_POINT('Ctrl Pts',(-4.04382334916498,-0.534302101112215,
56.7223104791382));
#25277=CARTESIAN_POINT('Ctrl Pts',(-2.6568499211277,3.09501768134366,56.5247998559553));
#25278=CARTESIAN_POINT('Ctrl Pts',(1.14068542359885,3.9162255614689,56.3272892327724));
#25279=CARTESIAN_POINT('Ctrl Pts',(3.90327603319866,1.1842390575404,56.1297786095896));
#25280=CARTESIAN_POINT('Ctrl Pts',(3.1244213559956,-2.62220844229581,55.9322679864067));
#25281=CARTESIAN_POINT('Ctrl Pts',(-0.489223166952141,-4.04952424500823,
55.7347573632238));
#25282=CARTESIAN_POINT('Ctrl Pts',(-3.65899514342298,-1.80270365434495,
55.5372467400409));
#25283=CARTESIAN_POINT('Ctrl Pts',(-3.50895807171802,2.07971131965516,55.3397361168581));
#25284=CARTESIAN_POINT('Ctrl Pts',(-0.175240701114049,4.07520264758084,
55.1422254936751));
#25285=CARTESIAN_POINT('Ctrl Pts',(3.31747269018585,2.37325954645769,54.9447148704923));
#25286=CARTESIAN_POINT('Ctrl Pts',(3.80024061166555,-1.4819437274876,54.7472042473094));
#25287=CARTESIAN_POINT('Ctrl Pts',(0.835047368213682,-3.99257834206022,
54.5496936241266));
#25288=CARTESIAN_POINT('Ctrl Pts',(-2.88778498530066,-2.88074362195241,
54.3521830009436));
#25289=CARTESIAN_POINT('Ctrl Pts',(-3.99052783946013,0.844791954511317,
54.1546723777608));
#25290=CARTESIAN_POINT('Ctrl Pts',(-1.47266179888568,3.80384715483272,53.9571617545778));
#25291=CARTESIAN_POINT('Ctrl Pts',(2.38135143493212,3.31166896863973,53.7596511313951));
#25292=CARTESIAN_POINT('Ctrl Pts',(4.074762650275,-0.185188965226226,53.5621405082121));
#25293=CARTESIAN_POINT('Ctrl Pts',(2.07113878435583,-3.51402481167261,53.3646298850293));
#25294=CARTESIAN_POINT('Ctrl Pts',(-1.81163113491682,-3.65458330148761,
53.1671192618463));
#25295=CARTESIAN_POINT('Ctrl Pts',(-4.05070621257184,-0.479335611734573,
52.9696086386635));
#25296=CARTESIAN_POINT('Ctrl Pts',(-2.61457359052401,3.13081364019015,52.7720980154806));
#25297=CARTESIAN_POINT('Ctrl Pts',(1.19376580308377,3.90037331825376,52.5745873922978));
#25298=CARTESIAN_POINT('Ctrl Pts',(3.91899622749745,1.13112135260593,52.3770767691148));
#25299=CARTESIAN_POINT('Ctrl Pts',(3.08852711531516,-2.66439787456312,52.179566145932));
#25300=CARTESIAN_POINT('Ctrl Pts',(-0.544182303682422,-4.04250689090106,
51.9820555227491));
#25301=CARTESIAN_POINT('Ctrl Pts',(-3.68312014722769,-1.75284639034888,
51.7845448995661));
#25302=CARTESIAN_POINT('Ctrl Pts',(-3.48042923450254,2.12717301477798,51.5870342763833));
#25303=CARTESIAN_POINT('Ctrl Pts',(-0.119804802211798,4.07720663223984,
51.3895236532005));
#25304=CARTESIAN_POINT('Ctrl Pts',(3.34924449343556,2.32798782340666,51.1920130300175));
#25305=CARTESIAN_POINT('Ctrl Pts',(3.78006842460215,-1.53341652389258,50.9945024068347));
#25306=CARTESIAN_POINT('Ctrl Pts',(0.780143076243845,-4.00355009270407,
50.7969917836518));
#25307=CARTESIAN_POINT('Ctrl Pts',(-2.92543071680569,-2.84126058289429,
50.5994811604689));
#25308=CARTESIAN_POINT('Ctrl Pts',(-3.98111802931833,0.89889955452203,50.401970537286));
#25309=CARTESIAN_POINT('Ctrl Pts',(-1.41523130310019,3.82425480839735,50.2044159988222));
#25310=CARTESIAN_POINT('Ctrl Pts',(1.13805318451675,3.45879401613092,50.0726983347526));
#25311=CARTESIAN_POINT('Ctrl Pts',(2.05774275266322,2.77731071842175,50.0068175450773));
#25312=CARTESIAN_POINT('Ctrl Pts',(-3.65733224398648,-0.533866881536543,
60.3367148073341));
#25313=CARTESIAN_POINT('Ctrl Pts',(-3.83400599920978,0.67646221732912,60.2708779329399));
#25314=CARTESIAN_POINT('Ctrl Pts',(-2.8883133804815,3.26589500907783,60.1392041841513));
#25315=CARTESIAN_POINT('Ctrl Pts',(1.1639876319452,4.20608449885579,59.9416935609684));
#25316=CARTESIAN_POINT('Ctrl Pts',(4.15557912152994,1.3217313209343,59.7441829377855));
#25317=CARTESIAN_POINT('Ctrl Pts',(3.37901941967257,-2.75772520730928,59.5466723146026));
#25318=CARTESIAN_POINT('Ctrl Pts',(-0.46442549763987,-4.33714676974401,
59.3491616914197));
#25319=CARTESIAN_POINT('Ctrl Pts',(-3.88594676068467,-1.98044379564081,
59.1516510682369));
#25320=CARTESIAN_POINT('Ctrl Pts',(-3.78202136416876,2.17260188470443,58.954140445054));
#25321=CARTESIAN_POINT('Ctrl Pts',(-0.246526864776077,4.3547026976008,58.7566298218711));
#25322=CARTESIAN_POINT('Ctrl Pts',(3.51257230980675,2.58564887533937,58.5591191986882));
#25323=CARTESIAN_POINT('Ctrl Pts',(4.08474675103516,-1.52930113123906,58.3616085755053));
#25324=CARTESIAN_POINT('Ctrl Pts',(0.950809957241094,-4.25674765701341,
58.1640979523225));
#25325=CARTESIAN_POINT('Ctrl Pts',(-3.04578868457094,-3.12202748967183,
57.9665873291396));
#25326=CARTESIAN_POINT('Ctrl Pts',(-4.27894534396861,0.845302375246406,
57.7690767059567));
#25327=CARTESIAN_POINT('Ctrl Pts',(-1.62980947426342,4.04569286745222,57.5715660827738));
#25328=CARTESIAN_POINT('Ctrl Pts',(2.49805265591715,3.57542111590398,57.3740554595909));
#25329=CARTESIAN_POINT('Ctrl Pts',(4.35943028393339,-0.138831872040531,
57.1765448364081));
#25330=CARTESIAN_POINT('Ctrl Pts',(2.26549325714367,-3.72712311600402,56.9790342132252));
#25331=CARTESIAN_POINT('Ctrl Pts',(-1.88392736797904,-3.9337924919015,56.7815235900423));
#25332=CARTESIAN_POINT('Ctrl Pts',(-4.32405934390643,-0.571329109433077,
56.5840129668594));
#25333=CARTESIAN_POINT('Ctrl Pts',(-2.84096898772335,3.30950166933803,56.3865023436765));
#25334=CARTESIAN_POINT('Ctrl Pts',(1.21973465170998,4.18761905992049,56.1889917204937));
#25335=CARTESIAN_POINT('Ctrl Pts',(4.17377213242608,1.26630654210795,55.9914810973108));
#25336=CARTESIAN_POINT('Ctrl Pts',(3.34094301163854,-2.80392686266102,55.7939704741279));
#25337=CARTESIAN_POINT('Ctrl Pts',(-0.52312621587481,-4.33015531047348,
55.596459850945));
#25338=CARTESIAN_POINT('Ctrl Pts',(-3.91256263518371,-1.92763058813491,
55.3989492277621));
#25339=CARTESIAN_POINT('Ctrl Pts',(-3.75212803015276,2.22383481865987,55.2014386045793));
#25340=CARTESIAN_POINT('Ctrl Pts',(-0.187384839953852,4.35761322022704,
55.0039279813963));
#25341=CARTESIAN_POINT('Ctrl Pts',(3.54737275729779,2.53772586764813,54.8064173582136));
#25342=CARTESIAN_POINT('Ctrl Pts',(4.06359638072673,-1.58464207476064,54.6089067350305));
#25343=CARTESIAN_POINT('Ctrl Pts',(0.892915951898455,-4.26926307001734,
54.4113961118479));
#25344=CARTESIAN_POINT('Ctrl Pts',(-3.08790779682808,-3.08037846867725,
54.2138854886648));
#25345=CARTESIAN_POINT('Ctrl Pts',(-4.26707046807556,0.903335835705069,
54.0163748654821));
#25346=CARTESIAN_POINT('Ctrl Pts',(-1.57471691071782,4.0674528564762,53.8188642422991));
#25347=CARTESIAN_POINT('Ctrl Pts',(2.54637852206613,3.54116683923112,53.6213536191163));
#25348=CARTESIAN_POINT('Ctrl Pts',(4.35714273121273,-0.198022516399034,
53.4238429959333));
#25349=CARTESIAN_POINT('Ctrl Pts',(2.21466820870652,-3.75754589397916,53.2263323727505));
#25350=CARTESIAN_POINT('Ctrl Pts',(-1.93717674098361,-3.90784505365324,
53.0288217495676));
#25351=CARTESIAN_POINT('Ctrl Pts',(-4.33141918810767,-0.51255345543617,
52.8313111263847));
#25352=CARTESIAN_POINT('Ctrl Pts',(-2.79576291748028,3.34777827960495,52.6338005032018));
#25353=CARTESIAN_POINT('Ctrl Pts',(1.27649348884792,4.170668260027,52.436289880019));
#25354=CARTESIAN_POINT('Ctrl Pts',(4.19058173244477,1.2095077928757,52.238779256836));
#25355=CARTESIAN_POINT('Ctrl Pts',(3.30256130863,-2.8490400125337,52.0412686336532));
#25356=CARTESIAN_POINT('Ctrl Pts',(-0.581894007687646,-4.32265165539842,
51.8437580104704));
#25357=CARTESIAN_POINT('Ctrl Pts',(-3.93835949600481,-1.87431822762135,
51.6462473872874));
#25358=CARTESIAN_POINT('Ctrl Pts',(-3.72162215131465,2.27458559794796,51.4487367641046));
#25359=CARTESIAN_POINT('Ctrl Pts',(-0.128107246464106,4.3597560805455,51.2512261409216));
#25360=CARTESIAN_POINT('Ctrl Pts',(3.58134633894373,2.4893168249747,51.0537155177388));
#25361=CARTESIAN_POINT('Ctrl Pts',(4.04202626590543,-1.63968192369417,50.8562048945559));
#25362=CARTESIAN_POINT('Ctrl Pts',(0.834206805574899,-4.28099516036702,
50.658694271373));
#25363=CARTESIAN_POINT('Ctrl Pts',(-3.12816236855811,-3.03815926441841,
50.4611836481901));
#25364=CARTESIAN_POINT('Ctrl Pts',(-4.25700856033262,0.961193079506533,
50.2636730250073));
#25365=CARTESIAN_POINT('Ctrl Pts',(-1.513306495256,4.08927475557118,50.0661184865434));
#25366=CARTESIAN_POINT('Ctrl Pts',(1.21691999908657,3.69848761746401,49.9344008224738));
#25367=CARTESIAN_POINT('Ctrl Pts',(2.20034383520893,2.96977768957263,49.8685200327985));
#25368=CARTESIAN_POINT('Ctrl Pts',(-3.89435862544394,-0.568466017373507,
60.1984172950554));
#25369=CARTESIAN_POINT('Ctrl Pts',(-4.08248234968987,0.720302749408164,
60.1325804206611));
#25370=CARTESIAN_POINT('Ctrl Pts',(-3.07550076828757,3.47755291286672,60.0009066718726));
#25371=CARTESIAN_POINT('Ctrl Pts',(1.23942397681511,4.47867471553828,59.8033960486895));
#25372=CARTESIAN_POINT('Ctrl Pts',(4.42489615819129,1.4073908047767,59.6058854255068));
#25373=CARTESIAN_POINT('Ctrl Pts',(3.59800875192051,-2.93644936561273,59.4083748023238));
#25374=CARTESIAN_POINT('Ctrl Pts',(-0.494524238420983,-4.61823094151229,
59.2108641791409));
#25375=CARTESIAN_POINT('Ctrl Pts',(-4.13778931634418,-2.10879347656808,
59.0133535559581));
#25376=CARTESIAN_POINT('Ctrl Pts',(-4.02712866608745,2.3134050518014,58.8158429327752));
#25377=CARTESIAN_POINT('Ctrl Pts',(-0.262503912195272,4.63692464351029,
58.6183323095923));
#25378=CARTESIAN_POINT('Ctrl Pts',(3.74021701055006,2.75322101693219,58.4208216864095));
#25379=CARTESIAN_POINT('Ctrl Pts',(4.34947324482307,-1.62841291248137,58.2233110632265));
#25380=CARTESIAN_POINT('Ctrl Pts',(1.01243056717861,-4.53262127926318,58.0258004400437));
#25381=CARTESIAN_POINT('Ctrl Pts',(-3.24318181771463,-3.32436154884964,
57.8282898168608));
#25382=CARTESIAN_POINT('Ctrl Pts',(-4.55625756601319,0.900085192304248,
57.6307791936779));
#25383=CARTESIAN_POINT('Ctrl Pts',(-1.73543505498141,4.307888335867,57.4332685704951));
#25384=CARTESIAN_POINT('Ctrl Pts',(2.65994781397828,3.80713895632791,57.2357579473121));
#25385=CARTESIAN_POINT('Ctrl Pts',(4.64195861783464,-0.147829363672537,
57.0382473241294));
#25386=CARTESIAN_POINT('Ctrl Pts',(2.41231657893511,-3.96867254233396,56.8407367009463));
#25387=CARTESIAN_POINT('Ctrl Pts',(-2.00602195965716,-4.18873585978749,
56.6432260777636));
#25388=CARTESIAN_POINT('Ctrl Pts',(-4.60429533864786,-0.608356117753937,
56.4457154545806));
#25389=CARTESIAN_POINT('Ctrl Pts',(-3.025088054319,3.52398565733241,56.2482048313978));
#25390=CARTESIAN_POINT('Ctrl Pts',(1.29878387982112,4.45901255837208,56.0506942082149));
#25391=CARTESIAN_POINT('Ctrl Pts',(4.44426823165348,1.3483740266755,55.853183585032));
#25392=CARTESIAN_POINT('Ctrl Pts',(3.55746466728151,-2.98564528302621,55.6556729618491));
#25393=CARTESIAN_POINT('Ctrl Pts',(-0.557029264797485,-4.61078637593874,
55.4581623386663));
#25394=CARTESIAN_POINT('Ctrl Pts',(-4.16613012694443,-2.05255752192486,
55.2606517154833));
#25395=CARTESIAN_POINT('Ctrl Pts',(-3.9952979885875,2.36795831766459,55.0631410923005));
#25396=CARTESIAN_POINT('Ctrl Pts',(-0.199528978793653,4.64002379287325,
54.8656304691176));
#25397=CARTESIAN_POINT('Ctrl Pts',(3.77727282440971,2.70219218883858,54.6681198459347));
#25398=CARTESIAN_POINT('Ctrl Pts',(4.32695214978791,-1.68734042203366,54.4706092227519));
#25399=CARTESIAN_POINT('Ctrl Pts',(0.950784535583229,-4.54594779797445,
54.273098599569));
#25400=CARTESIAN_POINT('Ctrl Pts',(-3.2880306083555,-3.2800133154021,54.0755879763861));
#25401=CARTESIAN_POINT('Ctrl Pts',(-4.54361309669097,0.961879716898822,
53.8780773532032));
#25402=CARTESIAN_POINT('Ctrl Pts',(-1.67677202254996,4.33105855811969,53.6805667300203));
#25403=CARTESIAN_POINT('Ctrl Pts',(2.71140560920012,3.77066470982251,53.4830561068375));
#25404=CARTESIAN_POINT('Ctrl Pts',(4.63952281215046,-0.210856067571843,
53.2855454836546));
#25405=CARTESIAN_POINT('Ctrl Pts',(2.35819763305721,-4.00106697628572,53.0880348604717));
#25406=CARTESIAN_POINT('Ctrl Pts',(-2.06272234705041,-4.16110680581888,
52.8905242372888));
#25407=CARTESIAN_POINT('Ctrl Pts',(-4.61213216364352,-0.545771299137771,
52.693013614106));
#25408=CARTESIAN_POINT('Ctrl Pts',(-2.97695224443653,3.56474291901975,52.495502990923));
#25409=CARTESIAN_POINT('Ctrl Pts',(1.35922117461208,4.44096320180024,52.2979923677402));
#25410=CARTESIAN_POINT('Ctrl Pts',(4.46216723739208,1.28789423314547,52.1004817445573));
#25411=CARTESIAN_POINT('Ctrl Pts',(3.51659550194484,-3.03368215050428,51.9029711213744));
#25412=CARTESIAN_POINT('Ctrl Pts',(-0.619605711692866,-4.60279641989579,
51.7054604981916));
#25413=CARTESIAN_POINT('Ctrl Pts',(-4.19359884478193,-1.9957900648938,51.5079498750086));
#25414=CARTESIAN_POINT('Ctrl Pts',(-3.96281506812675,2.42199818111792,51.3104392518258));
#25415=CARTESIAN_POINT('Ctrl Pts',(-0.136409690716418,4.64230552885116,
51.1129286286429));
#25416=CARTESIAN_POINT('Ctrl Pts',(3.8134481844519,2.65064582654275,50.91541800546));
#25417=CARTESIAN_POINT('Ctrl Pts',(4.30398410720872,-1.74594732349575,50.7179073822772));
#25418=CARTESIAN_POINT('Ctrl Pts',(0.888270534905953,-4.55844022802997,
50.5203967590942));
#25419=CARTESIAN_POINT('Ctrl Pts',(-3.33089402031053,-3.23505794594252,
50.3228861359114));
#25420=CARTESIAN_POINT('Ctrl Pts',(-4.5328990913469,1.02348660449103,50.1253755127285));
#25421=CARTESIAN_POINT('Ctrl Pts',(-1.61138168741181,4.35429470274499,49.9278209742646));
#25422=CARTESIAN_POINT('Ctrl Pts',(1.29578681365639,3.9381812187971,49.7961033101951));
#25423=CARTESIAN_POINT('Ctrl Pts',(2.34294491775465,3.1622446607235,49.7302225205197));
#25424=CARTESIAN_POINT('Ctrl Pts',(-3.89612849629295,0.579535085171301,
50.1419356690201));
#25425=CARTESIAN_POINT('Ctrl Pts',(-3.87378467426801,0.674953501696104,
50.1419356690201));
#25426=CARTESIAN_POINT('Ctrl Pts',(-3.84767496861433,0.769312903700949,
50.1419356690201));
#25427=CARTESIAN_POINT('Ctrl Pts',(-3.81772557524066,0.862409043007997,
50.1419356690201));
#25428=CARTESIAN_POINT('Ctrl Pts',(-3.78035729159179,0.978566418779723,
50.1419356690201));
#25429=CARTESIAN_POINT('Ctrl Pts',(-3.73701237818807,1.09275838157917,50.1419356690201));
#25430=CARTESIAN_POINT('Ctrl Pts',(-3.68803000615501,1.20468203541671,50.1419356690201));
#25431=CARTESIAN_POINT('Ctrl Pts',(-3.63914263045098,1.31638862471031,50.1419356690201));
#25432=CARTESIAN_POINT('Ctrl Pts',(-3.5846388856755,1.42583629348278,50.1419356690201));
#25433=CARTESIAN_POINT('Ctrl Pts',(-3.52481692824774,1.53268991237077,50.1419356690201));
#25434=CARTESIAN_POINT('Ctrl Pts',(-3.51432549294881,1.55142965070804,50.1419356690201));
#25435=CARTESIAN_POINT('Ctrl Pts',(-3.50367040283234,1.57008950539708,50.1419356690201));
#25436=CARTESIAN_POINT('Ctrl Pts',(-3.49285316887854,1.58866753931983,50.1419356690201));
#25437=CARTESIAN_POINT('Ctrl Pts',(-3.48296828602639,1.60564430895741,50.1419356690201));
#25438=CARTESIAN_POINT('Ctrl Pts',(-3.47295262127336,1.62254480368252,50.1419356690201));
#25439=CARTESIAN_POINT('Ctrl Pts',(-3.46280887008029,1.63936581395016,50.1419356690201));
#25440=CARTESIAN_POINT('Ctrl Pts',(-3.40044038534557,1.74278918289247,50.1419356690201));
#25441=CARTESIAN_POINT('Ctrl Pts',(-3.33321848428269,1.84323554294225,50.1419356690201));
#25442=CARTESIAN_POINT('Ctrl Pts',(-3.26147120928829,1.94041070411502,50.1419356690201));
#25443=CARTESIAN_POINT('Ctrl Pts',(-3.18993639848207,2.03729810186083,50.1419356690201));
#25444=CARTESIAN_POINT('Ctrl Pts',(-3.11390221728981,2.13093420721513,50.1419356690201));
#25445=CARTESIAN_POINT('Ctrl Pts',(-3.03366045198661,2.22098857179085,50.1419356690201));
#25446=CARTESIAN_POINT('Ctrl Pts',(-2.97045908890593,2.29191869865241,50.1419356690201));
#25447=CARTESIAN_POINT('Ctrl Pts',(-2.90464668830478,2.36062614854751,50.1419356690201));
#25448=CARTESIAN_POINT('Ctrl Pts',(-2.83635575923465,2.42692897605195,50.1419356690201));
#25449=CARTESIAN_POINT('Ctrl Pts',(-2.82453123970119,2.43840925739568,50.1419356690201));
#25450=CARTESIAN_POINT('Ctrl Pts',(-2.81263489701748,2.44981492176028,50.1419356690201));
#25451=CARTESIAN_POINT('Ctrl Pts',(-2.80067361886952,2.46113940299019,50.1419356690201));
#25452=CARTESIAN_POINT('Ctrl Pts',(-2.71480504293152,2.54243649051047,50.1419356690201));
#25453=CARTESIAN_POINT('Ctrl Pts',(-2.62550045622586,2.61964271914596,50.1419356690201));
#25454=CARTESIAN_POINT('Ctrl Pts',(-2.53305872915569,2.69247759565464,50.1419356690201));
#25455=CARTESIAN_POINT('Ctrl Pts',(-2.44149007077266,2.7646245809693,50.1419356690201));
#25456=CARTESIAN_POINT('Ctrl Pts',(-2.34684250503465,2.8324828433291,50.1419356690201));
#25457=CARTESIAN_POINT('Ctrl Pts',(-2.24938224755213,2.8957353593087,50.1419356690201));
#25458=CARTESIAN_POINT('Ctrl Pts',(-2.15449925673441,2.95731520783275,50.1419356690201));
#25459=CARTESIAN_POINT('Ctrl Pts',(-2.05694969435008,3.01452992641812,50.1419356690201));
#25460=CARTESIAN_POINT('Ctrl Pts',(-1.95696652726181,3.06703984578374,50.1419356690201));
#25461=CARTESIAN_POINT('Ctrl Pts',(-1.89667591165149,3.09870372937933,50.1419356690201));
#25462=CARTESIAN_POINT('Ctrl Pts',(-1.83550019348387,3.12865593444139,50.1419356690201));
#25463=CARTESIAN_POINT('Ctrl Pts',(-1.77348962752687,3.15681277973307,50.1419356690201));
#25464=CARTESIAN_POINT('Ctrl Pts',(-1.74929795611695,3.16779737790153,50.1419356690201));
#25465=CARTESIAN_POINT('Ctrl Pts',(-1.72497922357456,3.17850865291385,50.1419356690201));
#25466=CARTESIAN_POINT('Ctrl Pts',(-1.70053641711253,3.18894132850405,50.1419356690201));
#25467=CARTESIAN_POINT('Ctrl Pts',(-1.68181840755981,3.19693054699503,50.1419356690201));
#25468=CARTESIAN_POINT('Ctrl Pts',(-1.66302528100851,3.2047573351356,50.1419356690201));
#25469=CARTESIAN_POINT('Ctrl Pts',(-1.64416607327307,3.21241614219289,50.1419356690201));
#25470=CARTESIAN_POINT('Ctrl Pts',(-1.63050764989237,3.21796288789117,50.1419356690201));
#25471=CARTESIAN_POINT('Ctrl Pts',(-1.61681763107548,3.22342028814485,50.1419356690201));
#25472=CARTESIAN_POINT('Ctrl Pts',(-1.60310048450323,3.22878616897892,50.1419356690201));
#25473=CARTESIAN_POINT('Ctrl Pts',(-1.49934935361373,3.26937159261787,50.1419356690201));
#25474=CARTESIAN_POINT('Ctrl Pts',(-1.39396358293742,3.30475931357794,50.1419356690201));
#25475=CARTESIAN_POINT('Ctrl Pts',(-1.28718164270173,3.33466271573062,50.1419356690201));
#25476=CARTESIAN_POINT('Ctrl Pts',(-1.27250705830324,3.33877221212788,50.1419356690201));
#25477=CARTESIAN_POINT('Ctrl Pts',(-1.2578060890262,3.34277805381692,50.1419356690201));
#25478=CARTESIAN_POINT('Ctrl Pts',(-1.24307933955038,3.34667942017771,50.1419356690201));
#25479=CARTESIAN_POINT('Ctrl Pts',(-1.1343142888667,3.37549313162601,50.1419356690201));
#25480=CARTESIAN_POINT('Ctrl Pts',(-1.02414300966639,3.39861243996722,50.1419356690201));
#25481=CARTESIAN_POINT('Ctrl Pts',(-0.912964352790102,3.41614626393955,
50.1419356690201));
#25482=CARTESIAN_POINT('Ctrl Pts',(-0.800839823126348,3.43382926013092,
50.1419356690201));
#25483=CARTESIAN_POINT('Ctrl Pts',(-0.687689772958802,3.44583109383719,
50.1419356690201));
#25484=CARTESIAN_POINT('Ctrl Pts',(-0.57393170863822,3.45221162946615,50.1419356690201));
#25485=CARTESIAN_POINT('Ctrl Pts',(-0.517744174485096,3.45536311209474,
50.1419356690201));
#25486=CARTESIAN_POINT('Ctrl Pts',(-0.461408526409719,3.45714246118396,
50.1419356690201));
#25487=CARTESIAN_POINT('Ctrl Pts',(-0.404976884272194,3.45755255339111,
50.1419356690201));
#25488=CARTESIAN_POINT('Ctrl Pts',(-0.382828817917752,3.45771350474874,
50.1419356690201));
#25489=CARTESIAN_POINT('Ctrl Pts',(-0.360665981431297,3.45766350932293,
50.1419356690201));
#25490=CARTESIAN_POINT('Ctrl Pts',(-0.338491595318107,3.45740262660176,
50.1419356690201));
#25491=CARTESIAN_POINT('Ctrl Pts',(-0.319069607657413,3.45717412598102,
50.1419356690201));
#25492=CARTESIAN_POINT('Ctrl Pts',(-0.29963625765142,3.45678368122754,50.1419356690201));
#25493=CARTESIAN_POINT('Ctrl Pts',(-0.280217211800923,3.45623222480351,
50.1419356690201));
#25494=CARTESIAN_POINT('Ctrl Pts',(-0.169127678463448,3.45307753650039,
50.1419356690201));
#25495=CARTESIAN_POINT('Ctrl Pts',(-0.0583427143113645,3.4446575462879,
50.1419356690201));
#25496=CARTESIAN_POINT('Ctrl Pts',(0.0517566714309187,3.43109029249483,
50.1419356690201));
#25497=CARTESIAN_POINT('Ctrl Pts',(0.1619205923774,3.41751508620058,50.1419356690201));
#25498=CARTESIAN_POINT('Ctrl Pts',(0.271399017497807,3.39878624930298,50.1419356690201));
#25499=CARTESIAN_POINT('Ctrl Pts',(0.379795820539998,3.37497200733603,50.1419356690201));
#25500=CARTESIAN_POINT('Ctrl Pts',(0.486364561209112,3.35155938163876,50.1419356690201));
#25501=CARTESIAN_POINT('Ctrl Pts',(0.591888593020798,3.32323100631305,50.1419356690201));
#25502=CARTESIAN_POINT('Ctrl Pts',(0.695965598027709,3.29000918333453,50.1419356690201));
#25503=CARTESIAN_POINT('Ctrl Pts',(0.752494111669767,3.27196504117911,50.1419356690201));
#25504=CARTESIAN_POINT('Ctrl Pts',(0.808595232251325,3.25247661609081,50.1419356690201));
#25505=CARTESIAN_POINT('Ctrl Pts',(0.864200056320583,3.23154273761965,50.1419356690201));
#25506=CARTESIAN_POINT('Ctrl Pts',(0.895132425874015,3.21989744468158,50.1419356690201));
#25507=CARTESIAN_POINT('Ctrl Pts',(0.925911151271962,3.20780478753332,50.1419356690201));
#25508=CARTESIAN_POINT('Ctrl Pts',(0.95652386930051,3.19526414787022,50.1419356690201));
#25509=CARTESIAN_POINT('Ctrl Pts',(0.971283574996722,3.18921776706545,50.1419356690201));
#25510=CARTESIAN_POINT('Ctrl Pts',(0.986005114395488,3.18306698947413,50.1419356690201));
#25511=CARTESIAN_POINT('Ctrl Pts',(1.0006729614489,3.17681794427023,50.1419356690201));
#25512=CARTESIAN_POINT('Ctrl Pts',(1.09911941328325,3.13487611562723,50.1419356690201));
#25513=CARTESIAN_POINT('Ctrl Pts',(1.19530574259082,3.08844806575148,50.1419356690201));
#25514=CARTESIAN_POINT('Ctrl Pts',(1.2888754082226,3.03759818775854,50.1419356690201));
#25515=CARTESIAN_POINT('Ctrl Pts',(1.38113377414939,2.98746092778726,50.1419356690201));
#25516=CARTESIAN_POINT('Ctrl Pts',(1.47084895575196,2.9330245060841,50.1419356690201));
#25517=CARTESIAN_POINT('Ctrl Pts',(1.55764760760897,2.87431181658939,50.1419356690201));
#25518=CARTESIAN_POINT('Ctrl Pts',(1.6420441453812,2.81722397466285,50.1419356690201));
#25519=CARTESIAN_POINT('Ctrl Pts',(1.72368379584051,2.7560928654494,50.1419356690201));
#25520=CARTESIAN_POINT('Ctrl Pts',(1.8021854173623,2.6909086108042,50.1419356690201));
#25521=CARTESIAN_POINT('Ctrl Pts',(1.84119638382351,2.65851563951943,50.1419356690201));
#25522=CARTESIAN_POINT('Ctrl Pts',(1.87943176375489,2.6251212793804,50.1419356690201));
#25523=CARTESIAN_POINT('Ctrl Pts',(1.91684063918177,2.59072181572648,50.1419356690201));
#25524=CARTESIAN_POINT('',(1.09167700819691,3.03490005447944,60.2013629539769));
#25525=CARTESIAN_POINT('Ctrl Pts',(-3.89175630324294,-0.568086152065643,
60.1999356690201));
#25526=CARTESIAN_POINT('Ctrl Pts',(-3.8987272303941,-0.447109501454028,
60.1999356690201));
#25527=CARTESIAN_POINT('Ctrl Pts',(-3.89963247433286,-0.326050566837215,
60.1999356690201));
#25528=CARTESIAN_POINT('Ctrl Pts',(-3.89469346032466,-0.205273455014232,
60.1999356690201));
#25529=CARTESIAN_POINT('Ctrl Pts',(-3.88967463525396,-0.0825446683014876,
60.1999356690201));
#25530=CARTESIAN_POINT('Ctrl Pts',(-3.87862081872039,0.0398939529422601,
60.1999356690201));
#25531=CARTESIAN_POINT('Ctrl Pts',(-3.86171172561488,0.161648217750859,
60.1999356690201));
#25532=CARTESIAN_POINT('Ctrl Pts',(-3.84497309684275,0.282175050700306,
60.1999356690201));
#25533=CARTESIAN_POINT('Ctrl Pts',(-3.82249613254274,0.402031999762345,
60.1999356690201));
#25534=CARTESIAN_POINT('Ctrl Pts',(-3.79441072525008,0.520813100294654,
60.1999356690201));
#25535=CARTESIAN_POINT('Ctrl Pts',(-3.78992600069583,0.539780264010207,
60.1999356690201));
#25536=CARTESIAN_POINT('Ctrl Pts',(-3.78530028918843,0.558710999976427,
60.1999356690201));
#25537=CARTESIAN_POINT('Ctrl Pts',(-3.78053494608037,0.577601735753827,
60.1999356690201));
#25538=CARTESIAN_POINT('Ctrl Pts',(-3.75095064085873,0.694879606502539,
60.1999356690201));
#25539=CARTESIAN_POINT('Ctrl Pts',(-3.71598243568719,0.810643347701233,
60.1999356690201));
#25540=CARTESIAN_POINT('Ctrl Pts',(-3.67581069153357,0.924515931242179,
60.1999356690201));
#25541=CARTESIAN_POINT('Ctrl Pts',(-3.63593607793549,1.03754625551056,60.1999356690201));
#25542=CARTESIAN_POINT('Ctrl Pts',(-3.59093410589017,1.14871401938861,60.1999356690201));
#25543=CARTESIAN_POINT('Ctrl Pts',(-3.54093868932249,1.25762272055214,60.1999356690201));
#25544=CARTESIAN_POINT('Ctrl Pts',(-3.5082103591865,1.32891725455281,60.1999356690201));
#25545=CARTESIAN_POINT('Ctrl Pts',(-3.47334131077137,1.39924310877329,60.1999356690201));
#25546=CARTESIAN_POINT('Ctrl Pts',(-3.4363606857526,1.46848029561757,60.1999356690201));
#25547=CARTESIAN_POINT('Ctrl Pts',(-3.42737390205831,1.48530585282365,60.1999356690201));
#25548=CARTESIAN_POINT('Ctrl Pts',(-3.41826239001577,1.50206708169468,60.1999356690201));
#25549=CARTESIAN_POINT('Ctrl Pts',(-3.40902651492644,1.51876218737697,60.1999356690201));
#25550=CARTESIAN_POINT('Ctrl Pts',(-3.40039237704251,1.53436957087373,60.1999356690201));
#25551=CARTESIAN_POINT('Ctrl Pts',(-3.39165409022965,1.54991094148913,60.1999356690201));
#25552=CARTESIAN_POINT('Ctrl Pts',(-3.38281350142322,1.56538292504736,60.1999356690201));
#25553=CARTESIAN_POINT('Ctrl Pts',(-3.32466726855337,1.66714510159842,60.1999356690201));
#25554=CARTESIAN_POINT('Ctrl Pts',(-3.2620816872634,1.7659391973382,60.1999356690201));
#25555=CARTESIAN_POINT('Ctrl Pts',(-3.19521186487262,1.8614144002759,60.1999356690201));
#25556=CARTESIAN_POINT('Ctrl Pts',(-3.12913578401535,1.95575631720682,60.1999356690201));
#25557=CARTESIAN_POINT('Ctrl Pts',(-3.05887605633773,2.04685826973845,60.1999356690201));
#25558=CARTESIAN_POINT('Ctrl Pts',(-2.98454669867674,2.13434644657347,60.1999356690201));
#25559=CARTESIAN_POINT('Ctrl Pts',(-2.91228904583423,2.21939615651987,60.1999356690201));
#25560=CARTESIAN_POINT('Ctrl Pts',(-2.83618495656178,2.3010311258843,60.1999356690201));
#25561=CARTESIAN_POINT('Ctrl Pts',(-2.75631280208009,2.37886721205882,60.1999356690201));
#25562=CARTESIAN_POINT('Ctrl Pts',(-2.69729820240156,2.43637743568984,60.1999356690201));
#25563=CARTESIAN_POINT('Ctrl Pts',(-2.63622598358031,2.49181298681209,60.1999356690201));
#25564=CARTESIAN_POINT('Ctrl Pts',(-2.57312038377187,2.54500207854132,60.1999356690201));
#25565=CARTESIAN_POINT('Ctrl Pts',(-2.55330118941283,2.5617068551374,60.1999356690201));
#25566=CARTESIAN_POINT('Ctrl Pts',(-2.53328138931353,2.57818993465074,60.1999356690201));
#25567=CARTESIAN_POINT('Ctrl Pts',(-2.51306162809949,2.59444567022016,60.1999356690201));
#25568=CARTESIAN_POINT('Ctrl Pts',(-2.50195032082291,2.60337863787526,60.1999356690201));
#25569=CARTESIAN_POINT('Ctrl Pts',(-2.49077942647284,2.61224225258535,60.1999356690201));
#25570=CARTESIAN_POINT('Ctrl Pts',(-2.47955702841876,2.62102952177222,60.1999356690201));
#25571=CARTESIAN_POINT('Ctrl Pts',(-2.44671026938688,2.64674891901145,60.1999356690201));
#25572=CARTESIAN_POINT('Ctrl Pts',(-2.413404245263,2.67182898317495,60.1999356690201));
#25573=CARTESIAN_POINT('Ctrl Pts',(-2.37964494215065,2.69625243206787,60.1999356690201));
#25574=CARTESIAN_POINT('Ctrl Pts',(-2.28865280762842,2.76208144932471,60.1999356690201));
#25575=CARTESIAN_POINT('Ctrl Pts',(-2.19436954231683,2.82314381468693,60.1999356690201));
#25576=CARTESIAN_POINT('Ctrl Pts',(-2.09722649760078,2.8794215842726,60.1999356690201));
#25577=CARTESIAN_POINT('Ctrl Pts',(-1.99889796386925,2.93638614186099,60.1999356690201));
#25578=CARTESIAN_POINT('Ctrl Pts',(-1.89763846862526,2.98844876165294,60.1999356690201));
#25579=CARTESIAN_POINT('Ctrl Pts',(-1.79387705421774,3.0355402934247,60.1999356690201));
#25580=CARTESIAN_POINT('Ctrl Pts',(-1.69039303401084,3.08250593140553,60.1999356690201));
#25581=CARTESIAN_POINT('Ctrl Pts',(-1.58441947561242,3.1245270555689,60.1999356690201));
#25582=CARTESIAN_POINT('Ctrl Pts',(-1.47637852350488,3.16148394148629,60.1999356690201));
#25583=CARTESIAN_POINT('Ctrl Pts',(-1.42830734780708,3.17792734485811,60.1999356690201));
#25584=CARTESIAN_POINT('Ctrl Pts',(-1.37982693903537,3.193367516023,60.1999356690201));
#25585=CARTESIAN_POINT('Ctrl Pts',(-1.33097503044475,3.20779061651805,60.1999356690201));
#25586=CARTESIAN_POINT('Ctrl Pts',(-1.31592975202495,3.21223260392212,60.1999356690201));
#25587=CARTESIAN_POINT('Ctrl Pts',(-1.30084698790465,3.21657873798348,60.1999356690201));
#25588=CARTESIAN_POINT('Ctrl Pts',(-1.28573522280096,3.2208265122493,60.1999356690201));
#25589=CARTESIAN_POINT('Ctrl Pts',(-1.17699127245041,3.2513934083526,60.1999356690201));
#25590=CARTESIAN_POINT('Ctrl Pts',(-1.06700275791658,3.27680121139375,60.1999356690201));
#25591=CARTESIAN_POINT('Ctrl Pts',(-0.95619161988832,3.29700942866175,60.1999356690201));
#25592=CARTESIAN_POINT('Ctrl Pts',(-0.847048097392534,3.31691352905487,
60.1999356690201));
#25593=CARTESIAN_POINT('Ctrl Pts',(-0.737105558427078,3.33177324724764,
60.19993566902));
#25594=CARTESIAN_POINT('Ctrl Pts',(-0.626766108775439,3.34149844302225,
60.19993566902));
#25595=CARTESIAN_POINT('Ctrl Pts',(-0.513897826777057,3.35144652725363,
60.19993566902));
#25596=CARTESIAN_POINT('Ctrl Pts',(-0.400613190132631,3.35602226634987,
60.1999356690201));
#25597=CARTESIAN_POINT('Ctrl Pts',(-0.287356666109463,3.35507364513194,
60.1999356690201));
#25598=CARTESIAN_POINT('Ctrl Pts',(-0.230728404097879,3.35459933452298,
60.1999356690201));
#25599=CARTESIAN_POINT('Ctrl Pts',(-0.174107487097954,3.35274305441458,
60.1999356690201));
#25600=CARTESIAN_POINT('Ctrl Pts',(-0.117552012598016,3.34948051185152,
60.1999356690201));
#25601=CARTESIAN_POINT('Ctrl Pts',(-0.088900957870724,3.34782770482708,
60.1999356690201));
#25602=CARTESIAN_POINT('Ctrl Pts',(-0.0602667307051432,3.34581393210833,
60.19993566902));
#25603=CARTESIAN_POINT('Ctrl Pts',(-0.0316571036748412,3.3434356885107,
60.19993566902));
#25604=CARTESIAN_POINT('Ctrl Pts',(-0.0117570385253347,3.34178144805227,
60.19993566902));
#25605=CARTESIAN_POINT('Ctrl Pts',(0.00813420303698488,3.3399505393087,
60.1999356690201));
#25606=CARTESIAN_POINT('Ctrl Pts',(0.0280024783019314,3.33794291627126,
60.1999356690201));
#25607=CARTESIAN_POINT('Ctrl Pts',(0.0359537625046807,3.33713946548705,
60.1999356690201));
#25608=CARTESIAN_POINT('Ctrl Pts',(0.0439007585439898,3.33630777992627,
60.1999356690201));
#25609=CARTESIAN_POINT('Ctrl Pts',(0.051841555696066,3.33544802060429,60.1999356690201));
#25610=CARTESIAN_POINT('Ctrl Pts',(0.157654292629215,3.32399155279385,60.19993566902));
#25611=CARTESIAN_POINT('Ctrl Pts',(0.262528675282593,3.3075376814079,60.19993566902));
#25612=CARTESIAN_POINT('Ctrl Pts',(0.366101449193363,3.28600352068117,60.19993566902));
#25613=CARTESIAN_POINT('Ctrl Pts',(0.466999985779342,3.26502536955233,60.19993566902));
#25614=CARTESIAN_POINT('Ctrl Pts',(0.566663925722094,3.23922566881805,60.1999356690201));
#25615=CARTESIAN_POINT('Ctrl Pts',(0.664738724796578,3.20848274425607,60.1999356690201));
#25616=CARTESIAN_POINT('Ctrl Pts',(0.733222271488591,3.18701561376427,60.1999356690201));
#25617=CARTESIAN_POINT('Ctrl Pts',(0.800930585390643,3.1631372754956,60.19993566902));
#25618=CARTESIAN_POINT('Ctrl Pts',(0.867734791776628,3.13679351929711,60.19993566902));
#25619=CARTESIAN_POINT('Ctrl Pts',(0.943633142286453,3.10686355305895,60.1999356690201));
#25620=CARTESIAN_POINT('Ctrl Pts',(1.01836477737186,3.07375102185424,60.1999356690201));
#25621=CARTESIAN_POINT('Ctrl Pts',(1.09179082753359,3.03758696058814,60.1999356690201));
#25622=CARTESIAN_POINT('Ctrl Pts',(1.09082349994205,3.03252727184343,60.2013629539769));
#25623=CARTESIAN_POINT('Ctrl Pts',(1.10461504357036,3.02756634699704,60.2008871923247));
#25624=CARTESIAN_POINT('Ctrl Pts',(1.11837274419444,3.02251133744672,60.2004114306724));
#25625=CARTESIAN_POINT('Ctrl Pts',(1.13209532136445,3.01736271366979,60.1999356690201));
#25626=CARTESIAN_POINT('Ctrl Pts',(3.93531215953305,-0.0522584680823885,
60.611665739885));
#25627=CARTESIAN_POINT('Ctrl Pts',(3.91807438294499,-1.35546450485723,60.5457849464951));
#25628=CARTESIAN_POINT('Ctrl Pts',(2.48753474466723,-3.92031944802341,60.4140672787108));
#25629=CARTESIAN_POINT('Ctrl Pts',(-1.93244502466786,-4.22618854783819,
60.2165127365322));
#25630=CARTESIAN_POINT('Ctrl Pts',(-4.59187364716804,-0.689556313732268,
60.0190021133494));
#25631=CARTESIAN_POINT('Ctrl Pts',(-3.08810139139498,3.46876832474886,59.8214914901664));
#25632=CARTESIAN_POINT('Ctrl Pts',(1.2190055499893,4.48184773125158,59.6239808669837));
#25633=CARTESIAN_POINT('Ctrl Pts',(4.41935766022409,1.42755566308068,59.4264702438007));
#25634=CARTESIAN_POINT('Ctrl Pts',(3.61039927513463,-2.92146360824966,59.2289596206179));
#25635=CARTESIAN_POINT('Ctrl Pts',(-0.474465609420469,-4.62008497587082,
59.031448997435));
#25636=CARTESIAN_POINT('Ctrl Pts',(-4.12875297584294,-2.12677531987275,
58.8339383742521));
#25637=CARTESIAN_POINT('Ctrl Pts',(-4.03706704399223,2.29609679293635,58.6364277510693));
#25638=CARTESIAN_POINT('Ctrl Pts',(-0.282523388749893,4.63574983727625,
58.4389171278863));
#25639=CARTESIAN_POINT('Ctrl Pts',(3.72834203975631,2.76936788312511,58.2414065047037));
#25640=CARTESIAN_POINT('Ctrl Pts',(4.35648590055403,-1.60965577352385,58.0438958815205));
#25641=CARTESIAN_POINT('Ctrl Pts',(1.03198383136335,-4.52824147705999,57.846385258338));
#25642=CARTESIAN_POINT('Ctrl Pts',(-3.22883644391126,-3.33834830418739,
57.6488746351548));
#25643=CARTESIAN_POINT('Ctrl Pts',(-4.56013173592111,0.880429806891776,
57.4513640119722));
#25644=CARTESIAN_POINT('Ctrl Pts',(-1.75401569458227,4.30039378824156,57.2538533887891));
#25645=CARTESIAN_POINT('Ctrl Pts',(2.64351991746123,3.81860699986849,57.0563427656064));
#25646=CARTESIAN_POINT('Ctrl Pts',(4.64258801360327,-0.127804668657566,
56.8588321424235));
#25647=CARTESIAN_POINT('Ctrl Pts',(2.42943246328811,-3.95825912771161,56.6613215192406));
#25648=CARTESIAN_POINT('Ctrl Pts',(-1.98794896560828,-4.19738206968733,
56.4638108960578));
#25649=CARTESIAN_POINT('Ctrl Pts',(-4.60166281376544,-0.628217116468037,
56.2663002728748));
#25650=CARTESIAN_POINT('Ctrl Pts',(-3.04028452160891,3.51092970722542,56.0687896496921));
#25651=CARTESIAN_POINT('Ctrl Pts',(1.27954620218712,4.46460736115508,55.8712790265091));
#25652=CARTESIAN_POINT('Ctrl Pts',(4.43844369529037,1.36754339805686,55.6737684033263));
#25653=CARTESIAN_POINT('Ctrl Pts',(3.5703378822165,-2.9702937203288,55.4762577801434));
#25654=CARTESIAN_POINT('Ctrl Pts',(-0.537138177867132,-4.61318111026358,
55.2787471569606));
#25655=CARTESIAN_POINT('Ctrl Pts',(-4.15726836571013,-2.07052580696252,
55.0812365337776));
#25656=CARTESIAN_POINT('Ctrl Pts',(-4.0055058351096,2.3507191192728,54.8837259105949));
#25657=CARTESIAN_POINT('Ctrl Pts',(-0.219544848133634,4.6391548196919,54.6862152874118));
#25658=CARTESIAN_POINT('Ctrl Pts',(3.76560934971691,2.7184818598511,54.4887046642291));
#25659=CARTESIAN_POINT('Ctrl Pts',(4.33422334064896,-1.6686717358934,54.2911940410462));
#25660=CARTESIAN_POINT('Ctrl Pts',(0.970393252027999,-4.54183821290554,
54.0936834178634));
#25661=CARTESIAN_POINT('Ctrl Pts',(-3.27387540341237,-3.29419145471466,
53.8961727946805));
#25662=CARTESIAN_POINT('Ctrl Pts',(-4.54775436371161,0.942277677121238,
53.6986621714976));
#25663=CARTESIAN_POINT('Ctrl Pts',(-1.69545252177553,4.3238175883347,53.5011515483147));
#25664=CARTESIAN_POINT('Ctrl Pts',(2.69513497791465,3.78235449748423,53.3036409251319));
#25665=CARTESIAN_POINT('Ctrl Pts',(4.64042386796999,-0.190841576116406,
53.106130301949));
#25666=CARTESIAN_POINT('Ctrl Pts',(2.37545391819541,-3.99088714264033,52.9086196787661));
#25667=CARTESIAN_POINT('Ctrl Pts',(-2.04476960905902,-4.1699974048953,52.7111090555833));
#25668=CARTESIAN_POINT('Ctrl Pts',(-4.60976724491823,-0.56566667320796,
52.5135984324004));
#25669=CARTESIAN_POINT('Ctrl Pts',(-2.99232933597807,3.55189543258844,52.3160878092175));
#25670=CARTESIAN_POINT('Ctrl Pts',(1.34007067120665,4.44681699605373,52.1185771860347));
#25671=CARTESIAN_POINT('Ctrl Pts',(4.45658477518138,1.30714442139082,51.9210665628518));
#25672=CARTESIAN_POINT('Ctrl Pts',(3.52971349926043,-3.0185137753419,51.7235559396689));
#25673=CARTESIAN_POINT('Ctrl Pts',(-0.59982375698502,-4.60544720963951,
51.5260453164861));
#25674=CARTESIAN_POINT('Ctrl Pts',(-4.18483276393422,-2.01390467452604,
51.3285346933032));
#25675=CARTESIAN_POINT('Ctrl Pts',(-3.97355361721659,2.40495431726563,51.1310240701203));
#25676=CARTESIAN_POINT('Ctrl Pts',(-0.155841917726807,4.64159855987091,
50.9335134469375));
#25677=CARTESIAN_POINT('Ctrl Pts',(3.80082132445766,2.66731114812503,50.7360028237546));
#25678=CARTESIAN_POINT('Ctrl Pts',(4.31389481065517,-1.7278093001962,50.5384922005718));
#25679=CARTESIAN_POINT('Ctrl Pts',(0.90291182050654,-4.55380384351974,50.3409815773889));
#25680=CARTESIAN_POINT('Ctrl Pts',(-1.90071216242741,-3.68416167811652,
50.2093078286003));
#25681=CARTESIAN_POINT('Ctrl Pts',(-2.81196449438821,-2.75359200998455,
50.143470954206));
#25682=CARTESIAN_POINT('Ctrl Pts',(3.69578503881393,-0.0490776987086958,
60.4733624971722));
#25683=CARTESIAN_POINT('Ctrl Pts',(3.67959645853517,-1.27296266080429,60.4074817037822));
#25684=CARTESIAN_POINT('Ctrl Pts',(2.33612819521839,-3.68170487524816,60.2757640359979));
#25685=CARTESIAN_POINT('Ctrl Pts',(-1.81482462406369,-3.96895691450318,
60.0782094938193));
#25686=CARTESIAN_POINT('Ctrl Pts',(-4.31238418640244,-0.647585707156146,
59.8806988706365));
#25687=CARTESIAN_POINT('Ctrl Pts',(-2.90014068973178,3.25763790978137,59.6831882474536));
#25688=CARTESIAN_POINT('Ctrl Pts',(1.14480943092864,4.20905511937002,59.4856776242708));
#25689=CARTESIAN_POINT('Ctrl Pts',(4.15036857552919,1.34066591106553,59.2881670010878));
#25690=CARTESIAN_POINT('Ctrl Pts',(3.39064833595576,-2.74364549929111,59.0906563779051));
#25691=CARTESIAN_POINT('Ctrl Pts',(-0.445586736106843,-4.33887840142735,
58.8931457547221));
#25692=CARTESIAN_POINT('Ctrl Pts',(-3.87745186620453,-1.99732679123403,
58.6956351315393));
#25693=CARTESIAN_POINT('Ctrl Pts',(-3.79134649985317,2.15634232584225,58.4981245083564));
#25694=CARTESIAN_POINT('Ctrl Pts',(-0.265327290676925,4.35358980374317,
58.3006138851735));
#25695=CARTESIAN_POINT('Ctrl Pts',(3.50141238395363,2.60080724844964,58.1031032619907));
#25696=CARTESIAN_POINT('Ctrl Pts',(4.09132357494655,-1.51168229717659,57.9055926388077));
#25697=CARTESIAN_POINT('Ctrl Pts',(0.969170995752236,-4.25262505860291,
57.7080820156251));
#25698=CARTESIAN_POINT('Ctrl Pts',(-3.03230974784991,-3.13515604780627,
57.5105713924419));
#25699=CARTESIAN_POINT('Ctrl Pts',(-4.28257428163909,0.82684147435525,57.3130607692593));
#25700=CARTESIAN_POINT('Ctrl Pts',(-1.64725559220977,4.03864557099769,57.1155501460762));
#25701=CARTESIAN_POINT('Ctrl Pts',(2.48261915820144,3.58618326758065,56.9180395228936));
#25702=CARTESIAN_POINT('Ctrl Pts',(4.36001176691602,-0.120025696353209,
56.7205288997105));
#25703=CARTESIAN_POINT('Ctrl Pts',(2.28156237336314,-3.71733531443183,56.5230182765278));
#25704=CARTESIAN_POINT('Ctrl Pts',(-1.86695025634065,-3.94190377445863,
56.3255076533448));
#25705=CARTESIAN_POINT('Ctrl Pts',(-4.3215775245638,-0.589979987875952,
56.127997030162));
#25706=CARTESIAN_POINT('Ctrl Pts',(-2.85523424653382,3.2972330931508,55.9304864069791));
#25707=CARTESIAN_POINT('Ctrl Pts',(1.20166520946979,4.19286410343959,55.7329757837963));
#25708=CARTESIAN_POINT('Ctrl Pts',(4.16829291799269,1.28430635882949,55.5354651606134));
#25709=CARTESIAN_POINT('Ctrl Pts',(3.35302532396108,-2.78950351267095,55.3379545374305));
#25710=CARTESIAN_POINT('Ctrl Pts',(-0.504444669459887,-4.33239474722486,
55.1404439142477));
#25711=CARTESIAN_POINT('Ctrl Pts',(-3.90423163537527,-1.94450096704862,
54.9429332910648));
#25712=CARTESIAN_POINT('Ctrl Pts',(-3.76170629880514,2.20764000396175,54.745422667882));
#25713=CARTESIAN_POINT('Ctrl Pts',(-0.206182008488301,4.35678753814367,
54.5479120446991));
#25714=CARTESIAN_POINT('Ctrl Pts',(3.53641137793574,2.55301845918035,54.3504014215162));
#25715=CARTESIAN_POINT('Ctrl Pts',(4.07041605033671,-1.56710618781973,54.1528907983333));
#25716=CARTESIAN_POINT('Ctrl Pts',(0.911329195048302,-4.26539421410509,
53.9553801751505));
#25717=CARTESIAN_POINT('Ctrl Pts',(-3.07460736134031,-3.09368685374319,
53.7578695519676));
#25718=CARTESIAN_POINT('Ctrl Pts',(-4.27095027185859,0.884924905658877,
53.5603589287848));
#25719=CARTESIAN_POINT('Ctrl Pts',(-1.59225693159265,4.06064365562909,53.3628483056018));
#25720=CARTESIAN_POINT('Ctrl Pts',(2.53109261099707,3.55213731379099,53.165337682419));
#25721=CARTESIAN_POINT('Ctrl Pts',(4.35797934439678,-0.179225792822079,
52.9678270592361));
#25722=CARTESIAN_POINT('Ctrl Pts',(2.23086929203101,-3.74797738919779,52.7703164360533));
#25723=CARTESIAN_POINT('Ctrl Pts',(-1.92031244857547,-3.91618590753258,
52.5728058128704));
#25724=CARTESIAN_POINT('Ctrl Pts',(-4.32918867056402,-0.531236746425136,
52.3752951896875));
#25725=CARTESIAN_POINT('Ctrl Pts',(-2.81019790623775,3.33570539439735,52.1777845665047));
#25726=CARTESIAN_POINT('Ctrl Pts',(1.25850578983969,4.17615656855767,51.9802739433218));
#25727=CARTESIAN_POINT('Ctrl Pts',(4.18532982102126,1.2275836325824,51.782763320139));
#25728=CARTESIAN_POINT('Ctrl Pts',(3.31487358893889,-2.83478860078181,51.5852526969561));
#25729=CARTESIAN_POINT('Ctrl Pts',(-0.563314821575283,-4.32513157900353,
51.3877420737732));
#25730=CARTESIAN_POINT('Ctrl Pts',(-3.93011829605955,-1.89132614236984,
51.1902314505903));
#25731=CARTESIAN_POINT('Ctrl Pts',(-3.73169888794198,2.2585741167318,50.9927208274075));
#25732=CARTESIAN_POINT('Ctrl Pts',(-0.146356427293726,4.35908253737783,
50.7952102042246));
#25733=CARTESIAN_POINT('Ctrl Pts',(3.56948013694607,2.50496230933603,50.5976995810418));
#25734=CARTESIAN_POINT('Ctrl Pts',(4.05132483877166,-1.62264427896017,50.4001889578589));
#25735=CARTESIAN_POINT('Ctrl Pts',(0.847955095382388,-4.2766315433972,50.202678334676));
#25736=CARTESIAN_POINT('Ctrl Pts',(-1.78502321752906,-3.45992110881751,
50.0710045858874));
#25737=CARTESIAN_POINT('Ctrl Pts',(-2.64081116992483,-2.58599159125054,
50.0051677114931));
#25738=CARTESIAN_POINT('Ctrl Pts',(3.45625791809479,-0.045896929335003,
60.3350592544593));
#25739=CARTESIAN_POINT('Ctrl Pts',(3.44111853412534,-1.19046081675135,60.2691784610693));
#25740=CARTESIAN_POINT('Ctrl Pts',(2.18472164576956,-3.4430903024729,60.1374607932851));
#25741=CARTESIAN_POINT('Ctrl Pts',(-1.69720422345953,-3.71172528116816,
59.9399062511065));
#25742=CARTESIAN_POINT('Ctrl Pts',(-4.03289472563685,-0.605615100580024,
59.7423956279237));
#25743=CARTESIAN_POINT('Ctrl Pts',(-2.71217998806857,3.04650749481388,59.5448850047407));
#25744=CARTESIAN_POINT('Ctrl Pts',(1.07061331186798,3.93626250748847,59.3473743815579));
#25745=CARTESIAN_POINT('Ctrl Pts',(3.88137949083429,1.25377615905039,59.149863758375));
#25746=CARTESIAN_POINT('Ctrl Pts',(3.17089739677689,-2.56582739033256,58.9523531351921));
#25747=CARTESIAN_POINT('Ctrl Pts',(-0.416707862793216,-4.05767182698388,
58.7548425120093));
#25748=CARTESIAN_POINT('Ctrl Pts',(-3.62615075656612,-1.8678782625953,58.5573318888264));
#25749=CARTESIAN_POINT('Ctrl Pts',(-3.5456259557141,2.01658785874816,58.3598212656436));
#25750=CARTESIAN_POINT('Ctrl Pts',(-0.248131192603958,4.07142977021011,
58.1623106424607));
#25751=CARTESIAN_POINT('Ctrl Pts',(3.27448272815097,2.43224661377418,57.9648000192779));
#25752=CARTESIAN_POINT('Ctrl Pts',(3.82616124933907,-1.41370882082934,57.7672893960949));
#25753=CARTESIAN_POINT('Ctrl Pts',(0.906358160141125,-3.97700864014582,
57.5697787729122));
#25754=CARTESIAN_POINT('Ctrl Pts',(-2.83578305178858,-2.93196379142515,
57.3722681497291));
#25755=CARTESIAN_POINT('Ctrl Pts',(-4.00501682735706,0.773253141818731,
57.1747575265465));
#25756=CARTESIAN_POINT('Ctrl Pts',(-1.54049548983728,3.77689735375381,56.9772469033634));
#25757=CARTESIAN_POINT('Ctrl Pts',(2.32171839894166,3.35375953529281,56.7797362801807));
#25758=CARTESIAN_POINT('Ctrl Pts',(4.07743552022877,-0.112246724048854,
56.5822256569977));
#25759=CARTESIAN_POINT('Ctrl Pts',(2.13369228343817,-3.47641150115206,56.3847150338149));
#25760=CARTESIAN_POINT('Ctrl Pts',(-1.74595154707302,-3.68642547922993,
56.187204410632));
#25761=CARTESIAN_POINT('Ctrl Pts',(-4.04149223536218,-0.551742859283865,
55.9896937874491));
#25762=CARTESIAN_POINT('Ctrl Pts',(-2.67018397145873,3.08353647907615,55.7921831642663));
#25763=CARTESIAN_POINT('Ctrl Pts',(1.12378421675247,3.9211208457241,55.5946725410834));
#25764=CARTESIAN_POINT('Ctrl Pts',(3.898142140695,1.20106931960212,55.3971619179006));
#25765=CARTESIAN_POINT('Ctrl Pts',(3.13571276570568,-2.60871330501309,55.1996512947176));
#25766=CARTESIAN_POINT('Ctrl Pts',(-0.471751161052643,-4.05160838418615,
55.0021406715349));
#25767=CARTESIAN_POINT('Ctrl Pts',(-3.65119490504041,-1.81847612713471,
54.8046300483519));
#25768=CARTESIAN_POINT('Ctrl Pts',(-3.51790676250068,2.0645608886507,54.6071194251692));
#25769=CARTESIAN_POINT('Ctrl Pts',(-0.192819168842966,4.07442025659543,
54.4096088019862));
#25770=CARTESIAN_POINT('Ctrl Pts',(3.30721340615459,2.38755505850958,54.2120981788034));
#25771=CARTESIAN_POINT('Ctrl Pts',(3.80660876002445,-1.46554063974607,54.0145875556205));
#25772=CARTESIAN_POINT('Ctrl Pts',(0.85226513806861,-3.98895021530463,53.8170769324376));
#25773=CARTESIAN_POINT('Ctrl Pts',(-2.87533931926824,-2.89318225277171,
53.6195663092547));
#25774=CARTESIAN_POINT('Ctrl Pts',(-3.99414618000558,0.827572134196515,
53.4220556860719));
#25775=CARTESIAN_POINT('Ctrl Pts',(-1.48906134140977,3.79746972292347,53.2245450628891));
#25776=CARTESIAN_POINT('Ctrl Pts',(2.3670502440795,3.32192013009776,53.0270344397061));
#25777=CARTESIAN_POINT('Ctrl Pts',(4.07553482082357,-0.167610009527757,
52.8295238165233));
#25778=CARTESIAN_POINT('Ctrl Pts',(2.0862846658666,-3.50506763575524,52.6320131933405));
#25779=CARTESIAN_POINT('Ctrl Pts',(-1.79585528809192,-3.66237441016986,
52.4345025701575));
#25780=CARTESIAN_POINT('Ctrl Pts',(-4.04861009620979,-0.496806819642315,
52.2369919469747));
#25781=CARTESIAN_POINT('Ctrl Pts',(-2.62806647649744,3.11951535620625,52.0394813237918));
#25782=CARTESIAN_POINT('Ctrl Pts',(1.17694090847273,3.90549614106162,51.841970700609));
#25783=CARTESIAN_POINT('Ctrl Pts',(3.91407486686113,1.14802284377398,51.6444600774261));
#25784=CARTESIAN_POINT('Ctrl Pts',(3.10003367861737,-2.65106342622172,51.4469494542432));
#25785=CARTESIAN_POINT('Ctrl Pts',(-0.526805886165546,-4.04481594836757,
51.2494388310604));
#25786=CARTESIAN_POINT('Ctrl Pts',(-3.67540382818486,-1.76874761021364,
51.0519282078775));
#25787=CARTESIAN_POINT('Ctrl Pts',(-3.48984415866736,2.11219391619798,50.8544175846946));
#25788=CARTESIAN_POINT('Ctrl Pts',(-0.136870936860638,4.07656651488476,
50.6569069615117));
#25789=CARTESIAN_POINT('Ctrl Pts',(3.33813894943446,2.34261347054704,50.4593963383289));
#25790=CARTESIAN_POINT('Ctrl Pts',(3.78875486688816,-1.51747925772413,50.261885715146));
#25791=CARTESIAN_POINT('Ctrl Pts',(0.792998370258228,-3.99945924327466,
50.0643750919632));
#25792=CARTESIAN_POINT('Ctrl Pts',(-1.6693342726307,-3.23568053951851,49.9327013431746));
#25793=CARTESIAN_POINT('Ctrl Pts',(-2.46965784546145,-2.41839117251652,
49.8668644687803));
#25794=CARTESIAN_POINT('Ctrl Pts',(3.21673079737567,-0.0427161599613103,
60.1967560117465));
#25795=CARTESIAN_POINT('Ctrl Pts',(3.20264060971551,-1.10795897269841,60.1308752183565));
#25796=CARTESIAN_POINT('Ctrl Pts',(2.03331509632072,-3.20447572969764,59.9991575505722));
#25797=CARTESIAN_POINT('Ctrl Pts',(-1.57958382285538,-3.45449364783315,
59.8016030083936));
#25798=CARTESIAN_POINT('Ctrl Pts',(-3.75340526487125,-0.563644494003902,
59.6040923852108));
#25799=CARTESIAN_POINT('Ctrl Pts',(-2.52421928640537,2.83537707984639,59.4065817620279));
#25800=CARTESIAN_POINT('Ctrl Pts',(0.996417192807324,3.66346989560692,59.2090711388451));
#25801=CARTESIAN_POINT('Ctrl Pts',(3.61239040613939,1.16688640703525,59.0115605156621));
#25802=CARTESIAN_POINT('Ctrl Pts',(2.95114645759801,-2.38800928137401,58.8140498924793));
#25803=CARTESIAN_POINT('Ctrl Pts',(-0.387828989479593,-3.77646525254041,
58.6165392692965));
#25804=CARTESIAN_POINT('Ctrl Pts',(-3.3748496469277,-1.73842973395658,58.4190286461135));
#25805=CARTESIAN_POINT('Ctrl Pts',(-3.29990541157504,1.87683339165406,58.2215180229308));
#25806=CARTESIAN_POINT('Ctrl Pts',(-0.230935094530989,3.78926973667704,
58.0240073997477));
#25807=CARTESIAN_POINT('Ctrl Pts',(3.04755307234829,2.2636859790987,57.826496776565));
#25808=CARTESIAN_POINT('Ctrl Pts',(3.56099892373158,-1.31573534448208,57.628986153382));
#25809=CARTESIAN_POINT('Ctrl Pts',(0.843545324530011,-3.70139222168874,
57.4314755301993));
#25810=CARTESIAN_POINT('Ctrl Pts',(-2.63925635572723,-2.72877153504402,
57.2339649070163));
#25811=CARTESIAN_POINT('Ctrl Pts',(-3.72745937307503,0.719664809282207,
57.0364542838335));
#25812=CARTESIAN_POINT('Ctrl Pts',(-1.43373538746479,3.51514913650993,56.8389436606506));
#25813=CARTESIAN_POINT('Ctrl Pts',(2.16081763968186,3.12133580300496,56.6414330374678));
#25814=CARTESIAN_POINT('Ctrl Pts',(3.79485927354153,-0.104467751744498,
56.4439224142849));
#25815=CARTESIAN_POINT('Ctrl Pts',(1.9858221935132,-3.23548768787228,56.246411791102));
#25816=CARTESIAN_POINT('Ctrl Pts',(-1.62495283780538,-3.43094718400122,
56.0489011679192));
#25817=CARTESIAN_POINT('Ctrl Pts',(-3.76140694616054,-0.513505730691779,
55.8513905447362));
#25818=CARTESIAN_POINT('Ctrl Pts',(-2.48513369638366,2.86983986500152,55.6538799215535));
#25819=CARTESIAN_POINT('Ctrl Pts',(1.04590322403516,3.6493775880086,55.4563692983705));
#25820=CARTESIAN_POINT('Ctrl Pts',(3.62799136339733,1.11783228037474,55.2588586751877));
#25821=CARTESIAN_POINT('Ctrl Pts',(2.91840020745027,-2.42792309735524,55.0613480520048));
#25822=CARTESIAN_POINT('Ctrl Pts',(-0.439057652645399,-3.77082202114744,
54.863837428822));
#25823=CARTESIAN_POINT('Ctrl Pts',(-3.39815817470555,-1.69245128722081,
54.666326805639));
#25824=CARTESIAN_POINT('Ctrl Pts',(-3.27410722619621,1.92148177333965,54.4688161824563));
#25825=CARTESIAN_POINT('Ctrl Pts',(-0.179456329197637,3.79205297504719,
54.2713055592733));
#25826=CARTESIAN_POINT('Ctrl Pts',(3.07801543437343,2.22209165783883,54.0737949360905));
#25827=CARTESIAN_POINT('Ctrl Pts',(3.54280146971219,-1.3639750916724,53.8762843129076));
#25828=CARTESIAN_POINT('Ctrl Pts',(0.793201081088917,-3.71250621650416,
53.6787736897248));
#25829=CARTESIAN_POINT('Ctrl Pts',(-2.67607127719618,-2.69267765180024,
53.4812630665419));
#25830=CARTESIAN_POINT('Ctrl Pts',(-3.71734208815255,0.770219362734153,
53.283752443359));
#25831=CARTESIAN_POINT('Ctrl Pts',(-1.3858657512269,3.53429579021786,53.0862418201761));
#25832=CARTESIAN_POINT('Ctrl Pts',(2.20300787716194,3.09170294640452,52.8887311969933));
#25833=CARTESIAN_POINT('Ctrl Pts',(3.79309029725036,-0.155994226233431,
52.6912205738104));
#25834=CARTESIAN_POINT('Ctrl Pts',(1.9417000397022,-3.26215788231269,52.4937099506275));
#25835=CARTESIAN_POINT('Ctrl Pts',(-1.67139812760836,-3.40856291280714,
52.2961993274447));
#25836=CARTESIAN_POINT('Ctrl Pts',(-3.76803152185558,-0.46237689285949,
52.0986887042618));
#25837=CARTESIAN_POINT('Ctrl Pts',(-2.44593504675712,2.90332531801516,51.901178081079));
#25838=CARTESIAN_POINT('Ctrl Pts',(1.09537602710576,3.63483571356557,51.7036674578961));
#25839=CARTESIAN_POINT('Ctrl Pts',(3.64281991270102,1.06846205496556,51.5061568347132));
#25840=CARTESIAN_POINT('Ctrl Pts',(2.88519376829585,-2.46733825166162,51.3086462115304));
#25841=CARTESIAN_POINT('Ctrl Pts',(-0.49029695075581,-3.76450031773161,
51.1111355883475));
#25842=CARTESIAN_POINT('Ctrl Pts',(-3.42068936031018,-1.64616907805743,
50.9136249651647));
#25843=CARTESIAN_POINT('Ctrl Pts',(-3.24798942939275,1.96581371566414,50.7161143419817));
#25844=CARTESIAN_POINT('Ctrl Pts',(-0.127385446427556,3.79405049239167,
50.518603718799));
#25845=CARTESIAN_POINT('Ctrl Pts',(3.10679776192287,2.18026463175804,50.3210930956159));
#25846=CARTESIAN_POINT('Ctrl Pts',(3.52618489500465,-1.41231423648809,50.1235824724332));
#25847=CARTESIAN_POINT('Ctrl Pts',(0.738041645134074,-3.72228694315212,
49.9260718492503));
#25848=CARTESIAN_POINT('Ctrl Pts',(-1.55364532773234,-3.0114399702195,49.7943981004617));
#25849=CARTESIAN_POINT('Ctrl Pts',(-2.29850452099808,-2.25079075378251,
49.7285612260674));
#25850=CARTESIAN_POINT('',(3.07560303099836,-0.971134045656492,50.1404703033481));
#25851=CARTESIAN_POINT('Ctrl Pts',(3.07800019312434,-0.972037304811885,
50.1419356690201));
#25852=CARTESIAN_POINT('Ctrl Pts',(3.06227520141822,-1.05237632326202,50.1419356690201));
#25853=CARTESIAN_POINT('Ctrl Pts',(3.04333312529428,-1.13189057331352,50.1419356690201));
#25854=CARTESIAN_POINT('Ctrl Pts',(3.02115771737946,-1.21038988389693,50.1419356690201));
#25855=CARTESIAN_POINT('Ctrl Pts',(2.99336557492601,-1.30877202101979,50.1419356690201));
#25856=CARTESIAN_POINT('Ctrl Pts',(2.9604970300754,-1.40556061416761,50.1419356690201));
#25857=CARTESIAN_POINT('Ctrl Pts',(2.9229018831501,-1.50055476344149,50.1419356690201));
#25858=CARTESIAN_POINT('Ctrl Pts',(2.88423982723554,-1.59824474236563,50.1419356690201));
#25859=CARTESIAN_POINT('Ctrl Pts',(2.84057890699813,-1.69403760766469,50.1419356690201));
#25860=CARTESIAN_POINT('Ctrl Pts',(2.79224445502312,-1.78770962551524,50.1419356690202));
#25861=CARTESIAN_POINT('Ctrl Pts',(2.76578616493641,-1.83898570955108,50.1419356690202));
#25862=CARTESIAN_POINT('Ctrl Pts',(2.73792652669981,-1.88962614202262,50.1419356690202));
#25863=CARTESIAN_POINT('Ctrl Pts',(2.70871256304879,-1.93959251956205,50.1419356690202));
#25864=CARTESIAN_POINT('Ctrl Pts',(2.69706069008747,-1.95952141008791,50.1419356690202));
#25865=CARTESIAN_POINT('Ctrl Pts',(2.68519332639328,-1.97934305583239,50.1419356690202));
#25866=CARTESIAN_POINT('Ctrl Pts',(2.67311327275347,-1.99905494404161,50.1419356690202));
#25867=CARTESIAN_POINT('Ctrl Pts',(2.66446129450681,-2.01317299625164,50.1419356690202));
#25868=CARTESIAN_POINT('Ctrl Pts',(2.65570515937501,-2.02722665323309,50.1419356690202));
#25869=CARTESIAN_POINT('Ctrl Pts',(2.64684719817748,-2.04121370216548,50.1419356690202));
#25870=CARTESIAN_POINT('Ctrl Pts',(2.58908448250295,-2.13242317041571,50.1419356690202));
#25871=CARTESIAN_POINT('Ctrl Pts',(2.52698395322515,-2.22082070907395,50.1419356690202));
#25872=CARTESIAN_POINT('Ctrl Pts',(2.460918055731,-2.30618506499463,50.1419356690202));
#25873=CARTESIAN_POINT('Ctrl Pts',(2.39187403139581,-2.39539748609383,50.1419356690202));
#25874=CARTESIAN_POINT('Ctrl Pts',(2.31849891374532,-2.48129793395378,50.1419356690202));
#25875=CARTESIAN_POINT('Ctrl Pts',(2.24116020239773,-2.5636195351057,50.1419356690202));
#25876=CARTESIAN_POINT('Ctrl Pts',(2.16382149105007,-2.64594113625767,50.1419356690202));
#25877=CARTESIAN_POINT('Ctrl Pts',(2.08251855748945,-2.72468469072004,50.1419356690202));
#25878=CARTESIAN_POINT('Ctrl Pts',(1.99756923591343,-2.79955699478053,50.1419356690202));
#25879=CARTESIAN_POINT('Ctrl Pts',(1.97312667799664,-2.82110008181654,50.1419356690202));
#25880=CARTESIAN_POINT('Ctrl Pts',(1.94838195754849,-2.84232246238748,50.1419356690202));
#25881=CARTESIAN_POINT('Ctrl Pts',(1.9233419986283,-2.86321660162443,50.1419356690202));
#25882=CARTESIAN_POINT('Ctrl Pts',(1.91194750369415,-2.87272453110817,50.1419356690202));
#25883=CARTESIAN_POINT('Ctrl Pts',(1.90049372334605,-2.88216289265972,50.1419356690202));
#25884=CARTESIAN_POINT('Ctrl Pts',(1.88898826977189,-2.89152553551587,50.1419356690202));
#25885=CARTESIAN_POINT('Ctrl Pts',(1.80049123610051,-2.96354061208404,50.1419356690202));
#25886=CARTESIAN_POINT('Ctrl Pts',(1.70882666426025,-3.03117349173495,50.1419356690202));
#25887=CARTESIAN_POINT('Ctrl Pts',(1.61437075449497,-3.09417590432581,50.1419356690202));
#25888=CARTESIAN_POINT('Ctrl Pts',(1.51941266904254,-3.15751326980542,50.1419356690202));
#25889=CARTESIAN_POINT('Ctrl Pts',(1.42163289527908,-3.21617156831816,50.1419356690202));
#25890=CARTESIAN_POINT('Ctrl Pts',(1.3213682282809,-3.26987175410814,50.1419356690202));
#25891=CARTESIAN_POINT('Ctrl Pts',(1.2224245598561,-3.32286443374522,50.1419356690202));
#25892=CARTESIAN_POINT('Ctrl Pts',(1.12106035282451,-3.37102943937167,50.1419356690202));
#25893=CARTESIAN_POINT('Ctrl Pts',(1.01756488383265,-3.41406217225391,50.1419356690202));
#25894=CARTESIAN_POINT('Ctrl Pts',(0.966275322332376,-3.43538803338761,
50.1419356690202));
#25895=CARTESIAN_POINT('Ctrl Pts',(0.91446186828967,-3.45545281962562,50.1419356690202));
#25896=CARTESIAN_POINT('Ctrl Pts',(0.862157328497213,-3.47421531578325,
50.1419356690202));
#25897=CARTESIAN_POINT('Ctrl Pts',(0.81733495941787,-3.49029383460712,50.1419356690202));
#25898=CARTESIAN_POINT('Ctrl Pts',(0.772151923918596,-3.50541596154927,
50.1419356690202));
#25899=CARTESIAN_POINT('Ctrl Pts',(0.726628142940982,-3.51955390646554,
50.1419356690202));
#25900=CARTESIAN_POINT('Ctrl Pts',(0.718762362529219,-3.52199671696583,
50.1419356690202));
#25901=CARTESIAN_POINT('Ctrl Pts',(0.710888867590843,-3.52440937617116,
50.1419356690202));
#25902=CARTESIAN_POINT('Ctrl Pts',(0.703008125814777,-3.52679168831568,
50.1419356690202));
#25903=CARTESIAN_POINT('Ctrl Pts',(0.595193612326785,-3.55938352194457,
50.1419356690202));
#25904=CARTESIAN_POINT('Ctrl Pts',(0.486004814809058,-3.58630600421687,
50.1419356690202));
#25905=CARTESIAN_POINT('Ctrl Pts',(0.375834415117319,-3.60778456100658,
50.1419356690202));
#25906=CARTESIAN_POINT('Ctrl Pts',(0.265437021161436,-3.6293073720534,50.1419356690202));
#25907=CARTESIAN_POINT('Ctrl Pts',(0.154053290098907,-3.64536375893427,
50.1419356690202));
#25908=CARTESIAN_POINT('Ctrl Pts',(0.0420494266149386,-3.65613226637667,
50.1419356690202));
#25909=CARTESIAN_POINT('Ctrl Pts',(-0.0727136961382722,-3.66716606023914,
50.1419356690202));
#25910=CARTESIAN_POINT('Ctrl Pts',(-0.188128572258745,-3.67264837361943,
50.1419356690202));
#25911=CARTESIAN_POINT('Ctrl Pts',(-0.303821229732827,-3.67271959388211,
50.1419356690202));
#25912=CARTESIAN_POINT('Ctrl Pts',(-0.413254182712562,-3.67278696067813,
50.1419356690202));
#25913=CARTESIAN_POINT('Ctrl Pts',(-0.522936411188278,-3.66801249049235,
50.1419356690202));
#25914=CARTESIAN_POINT('Ctrl Pts',(-0.632558318696721,-3.65847265496365,
50.1419356690202));
#25915=CARTESIAN_POINT('Ctrl Pts',(-0.656240589624941,-3.65641170770651,
50.1419356690202));
#25916=CARTESIAN_POINT('Ctrl Pts',(-0.679926094463313,-3.65412746565096,
50.1419356690202));
#25917=CARTESIAN_POINT('Ctrl Pts',(-0.703578099800705,-3.65162429841491,
50.1419356690202));
#25918=CARTESIAN_POINT('Ctrl Pts',(-0.822930318687432,-3.63899287204724,
50.1419356690202));
#25919=CARTESIAN_POINT('Ctrl Pts',(-0.941557594243896,-3.62078266779788,
50.1419356690202));
#25920=CARTESIAN_POINT('Ctrl Pts',(-1.05905125671003,-3.59719277930163,
50.1419356690202));
#25921=CARTESIAN_POINT('Ctrl Pts',(-1.17679134286499,-3.57355341488284,
50.1419356690202));
#25922=CARTESIAN_POINT('Ctrl Pts',(-1.29339391787156,-3.54451169179539,
50.1419356690202));
#25923=CARTESIAN_POINT('Ctrl Pts',(-1.40846037353927,-3.51021482329977,
50.1419356690202));
#25924=CARTESIAN_POINT('Ctrl Pts',(-1.52316558732171,-3.47602562706504,
50.1419356690202));
#25925=CARTESIAN_POINT('Ctrl Pts',(-1.63634518520109,-3.43661410589424,
50.1419356690202));
#25926=CARTESIAN_POINT('Ctrl Pts',(-1.74760384492387,-3.39207497720295,
50.1419356690202));
#25927=CARTESIAN_POINT('Ctrl Pts',(-1.8032331747853,-3.36980541285729,50.1419356690202));
#25928=CARTESIAN_POINT('Ctrl Pts',(-1.85838218161433,-3.34625315838058,
50.1419356690202));
#25929=CARTESIAN_POINT('Ctrl Pts',(-1.91300035582,-3.32142538195897,50.1419356690202));
#25930=CARTESIAN_POINT('Ctrl Pts',(-1.94936455815574,-3.30489531118176,
50.1419356690202));
#25931=CARTESIAN_POINT('Ctrl Pts',(-1.98549343725982,-3.28779976900701,
50.1419356690202));
#25932=CARTESIAN_POINT('Ctrl Pts',(-2.02137178270244,-3.27014011787672,
50.1419356690202));
#25933=CARTESIAN_POINT('Ctrl Pts',(-2.03938186587157,-3.26127538953792,
50.1419356690202));
#25934=CARTESIAN_POINT('Ctrl Pts',(-2.05733089912592,-3.252267440223,50.1419356690202));
#25935=CARTESIAN_POINT('Ctrl Pts',(-2.07521052413803,-3.24311966611299,
50.1419356690202));
#25936=CARTESIAN_POINT('Ctrl Pts',(-2.18541124809655,-3.1867375367982,50.1419356690202));
#25937=CARTESIAN_POINT('Ctrl Pts',(-2.29261698285448,-3.12523274643722,
50.1419356690202));
#25938=CARTESIAN_POINT('Ctrl Pts',(-2.3964196822934,-3.05876555109958,50.1419356690202));
#25939=CARTESIAN_POINT('Ctrl Pts',(-2.49996259686187,-2.99246470183795,
50.1419356690201));
#25940=CARTESIAN_POINT('Ctrl Pts',(-2.60012039529287,-2.92122610018819,
50.1419356690201));
#25941=CARTESIAN_POINT('Ctrl Pts',(-2.69648100191037,-2.84515796161608,
50.1419356690201));
#25942=CARTESIAN_POINT('Ctrl Pts',(-2.73495674613104,-2.81478477960966,
50.1419356690201));
#25943=CARTESIAN_POINT('Ctrl Pts',(-2.77282694295787,-2.78364105966542,
50.1419356690201));
#25944=CARTESIAN_POINT('Ctrl Pts',(-2.81006454495679,-2.75173150091943,
50.1419356690201));
#25945=CARTESIAN_POINT('Ctrl Pts',(3.08633327008855,-0.927720059309073,
50.1419356690201));
#25946=CARTESIAN_POINT('Ctrl Pts',(3.08205063481698,-0.941967503448788,
50.1414472137961));
#25947=CARTESIAN_POINT('Ctrl Pts',(3.07766934222995,-0.956185292203961,
50.1409587585721));
#25948=CARTESIAN_POINT('Ctrl Pts',(3.0731898124641,-0.970372062183785,50.1404703033481));
#25949=CARTESIAN_POINT('Ctrl Pts',(3.22243683749933,-0.0449265047301374,
60.1999356690201));
#25950=CARTESIAN_POINT('Ctrl Pts',(3.23190969153617,-0.146959477571174,
60.1999356690201));
#25951=CARTESIAN_POINT('Ctrl Pts',(3.23609830245048,-0.249183173425684,
60.1999356690201));
#25952=CARTESIAN_POINT('Ctrl Pts',(3.23526888419945,-0.351287921296696,
60.1999356690201));
#25953=CARTESIAN_POINT('Ctrl Pts',(3.23441346753709,-0.456593178958777,
60.19993566902));
#25954=CARTESIAN_POINT('Ctrl Pts',(3.22822059903152,-0.561772520799036,
60.19993566902));
#25955=CARTESIAN_POINT('Ctrl Pts',(3.21692873692298,-0.666504456816874,
60.19993566902));
#25956=CARTESIAN_POINT('Ctrl Pts',(3.205645923797,-0.771152463589466,60.1999356690201));
#25957=CARTESIAN_POINT('Ctrl Pts',(3.18927208808766,-0.875354527570815,
60.19993566902));
#25958=CARTESIAN_POINT('Ctrl Pts',(3.16799367544636,-0.978797438385924,
60.19993566902));
#25959=CARTESIAN_POINT('Ctrl Pts',(3.16387062690766,-0.99884123345022,60.19993566902));
#25960=CARTESIAN_POINT('Ctrl Pts',(3.15956328353731,-1.01885652861755,60.19993566902));
#25961=CARTESIAN_POINT('Ctrl Pts',(3.155072787946,-1.03884104070003,60.19993566902));
#25962=CARTESIAN_POINT('Ctrl Pts',(3.15075715067165,-1.05804736291971,60.19993566902));
#25963=CARTESIAN_POINT('Ctrl Pts',(3.1462740972738,-1.0772172541688,60.19993566902));
#25964=CARTESIAN_POINT('Ctrl Pts',(3.14162701596928,-1.09634105452731,60.19993566902));
#25965=CARTESIAN_POINT('Ctrl Pts',(3.11602725935698,-1.20168989664972,60.19993566902));
#25966=CARTESIAN_POINT('Ctrl Pts',(3.08543783388726,-1.30571176782322,60.19993566902));
#25967=CARTESIAN_POINT('Ctrl Pts',(3.0501086657506,-1.40807351735763,60.19993566902));
#25968=CARTESIAN_POINT('Ctrl Pts',(3.01408121476251,-1.51245845221204,60.19993566902));
#25969=CARTESIAN_POINT('Ctrl Pts',(2.97312473432208,-1.61511781792578,60.19993566902));
#25970=CARTESIAN_POINT('Ctrl Pts',(2.92745013565406,-1.71570108022376,60.19993566902));
#25971=CARTESIAN_POINT('Ctrl Pts',(2.89842288396775,-1.77962404299296,60.19993566902));
#25972=CARTESIAN_POINT('Ctrl Pts',(2.86748894951469,-1.84270850865144,60.19993566902));
#25973=CARTESIAN_POINT('Ctrl Pts',(2.83469170847284,-1.90486266936677,60.19993566902));
#25974=CARTESIAN_POINT('Ctrl Pts',(2.81595808148896,-1.94036482824812,60.19993566902));
#25975=CARTESIAN_POINT('Ctrl Pts',(2.79661637492879,-1.97556342443468,60.19993566902));
#25976=CARTESIAN_POINT('Ctrl Pts',(2.77667350924734,-2.01044092927213,60.19993566902));
#25977=CARTESIAN_POINT('Ctrl Pts',(2.76841891872605,-2.02487714548278,60.19993566902));
#25978=CARTESIAN_POINT('Ctrl Pts',(2.76006622223582,-2.03924977505433,60.19993566902));
#25979=CARTESIAN_POINT('Ctrl Pts',(2.7516167194928,-2.053556959919,60.19993566902));
#25980=CARTESIAN_POINT('Ctrl Pts',(2.69392882598369,-2.15123742491092,60.19993566902));
#25981=CARTESIAN_POINT('Ctrl Pts',(2.63172633617838,-2.24587894137787,60.19993566902));
#25982=CARTESIAN_POINT('Ctrl Pts',(2.56525668975559,-2.33712629647658,60.19993566902));
#25983=CARTESIAN_POINT('Ctrl Pts',(2.49866320152646,-2.42854365755376,60.19993566902));
#25984=CARTESIAN_POINT('Ctrl Pts',(2.42778635625904,-2.51655510291817,60.19993566902));
#25985=CARTESIAN_POINT('Ctrl Pts',(2.35282359530363,-2.60079329271395,60.19993566902));
#25986=CARTESIAN_POINT('Ctrl Pts',(2.27928471630906,-2.68343141819332,60.19993566902));
#25987=CARTESIAN_POINT('Ctrl Pts',(2.20181324314207,-2.76243906231675,60.19993566902));
#25988=CARTESIAN_POINT('Ctrl Pts',(2.1205516927396,-2.83744719687121,60.19993566902));
#25989=CARTESIAN_POINT('Ctrl Pts',(2.05269464105882,-2.90008236489019,60.19993566902));
#25990=CARTESIAN_POINT('Ctrl Pts',(1.98219392384327,-2.95992853986898,60.19993566902));
#25991=CARTESIAN_POINT('Ctrl Pts',(1.90911141620034,-3.01675254204845,60.19993566902));
#25992=CARTESIAN_POINT('Ctrl Pts',(1.89622466318962,-3.02677240733202,60.19993566902));
#25993=CARTESIAN_POINT('Ctrl Pts',(1.88325740636086,-3.03669830080153,60.19993566902));
#25994=CARTESIAN_POINT('Ctrl Pts',(1.87022294168935,-3.04652123647435,60.19993566902));
#25995=CARTESIAN_POINT('Ctrl Pts',(1.78116472099078,-3.1136366259517,60.19993566902));
#25996=CARTESIAN_POINT('Ctrl Pts',(1.68883725354168,-3.1760549216553,60.19993566902));
#25997=CARTESIAN_POINT('Ctrl Pts',(1.59369488622457,-3.2338371928481,60.19993566902));
#25998=CARTESIAN_POINT('Ctrl Pts',(1.49780680382872,-3.29207235492567,60.19993566902));
#25999=CARTESIAN_POINT('Ctrl Pts',(1.39905888922488,-3.34559878068317,60.19993566902));
#26000=CARTESIAN_POINT('Ctrl Pts',(1.29787166956309,-3.39444464211518,60.19993566902));
#26001=CARTESIAN_POINT('Ctrl Pts',(1.19409883891314,-3.44453864927613,60.19993566902));
#26002=CARTESIAN_POINT('Ctrl Pts',(1.08775982993701,-3.48971023405494,60.19993566902));
#26003=CARTESIAN_POINT('Ctrl Pts',(0.9792709270014,-3.52994870798746,60.19993566902));
#26004=CARTESIAN_POINT('Ctrl Pts',(0.87865632453916,-3.56726660824138,60.19993566902));
#26005=CARTESIAN_POINT('Ctrl Pts',(0.776191695095459,-3.6003412563449,60.19993566902));
#26006=CARTESIAN_POINT('Ctrl Pts',(0.672189142038902,-3.62912941459683,
60.19993566902));
#26007=CARTESIAN_POINT('Ctrl Pts',(0.650407555589505,-3.63515861041226,
60.19993566902));
#26008=CARTESIAN_POINT('Ctrl Pts',(0.62855355524072,-3.64100084058666,60.19993566902));
#26009=CARTESIAN_POINT('Ctrl Pts',(0.606659738943875,-3.64664810681024,
60.19993566902));
#26010=CARTESIAN_POINT('Ctrl Pts',(0.491699373233907,-3.67630085357315,
60.19993566902));
#26011=CARTESIAN_POINT('Ctrl Pts',(0.375508042115669,-3.70062174153854,
60.19993566902));
#26012=CARTESIAN_POINT('Ctrl Pts',(0.258541788795668,-3.71964227030934,
60.19993566902));
#26013=CARTESIAN_POINT('Ctrl Pts',(0.140091959710903,-3.738904051533,60.19993566902));
#26014=CARTESIAN_POINT('Ctrl Pts',(0.0208466229849164,-3.7527304787693,
60.19993566902));
#26015=CARTESIAN_POINT('Ctrl Pts',(-0.098751394978667,-3.76110953310029,
60.19993566902));
#26016=CARTESIAN_POINT('Ctrl Pts',(-0.218381330657788,-3.76949082359101,
60.19993566902));
#26017=CARTESIAN_POINT('Ctrl Pts',(-0.338365031743393,-3.7724220719954,
60.19993566902));
#26018=CARTESIAN_POINT('Ctrl Pts',(-0.458277031791744,-3.76984273951047,
60.19993566902));
#26019=CARTESIAN_POINT('Ctrl Pts',(-0.557812449297683,-3.76770171162611,
60.19993566902));
#26020=CARTESIAN_POINT('Ctrl Pts',(-0.657299034614091,-3.7617630037591,
60.19993566902));
#26021=CARTESIAN_POINT('Ctrl Pts',(-0.756495963167153,-3.75196478708744,
60.19993566902));
#26022=CARTESIAN_POINT('Ctrl Pts',(-0.775448827008612,-3.7500927103087,
60.19993566902));
#26023=CARTESIAN_POINT('Ctrl Pts',(-0.794391113280761,-3.74807966670157,
60.19993566902));
#26024=CARTESIAN_POINT('Ctrl Pts',(-0.813321133086311,-3.74592511735631,
60.19993566902));
#26025=CARTESIAN_POINT('Ctrl Pts',(-0.828796076691622,-3.74416381282756,
60.19993566902));
#26026=CARTESIAN_POINT('Ctrl Pts',(-0.844252778619867,-3.74230909014765,
60.19993566902));
#26027=CARTESIAN_POINT('Ctrl Pts',(-0.85969142305059,-3.74036085764192,
60.19993566902));
#26028=CARTESIAN_POINT('Ctrl Pts',(-0.982113292440273,-3.72491220433385,
60.19993566902));
#26029=CARTESIAN_POINT('Ctrl Pts',(-1.10337504609058,-3.70359051818525,
60.19993566902));
#26030=CARTESIAN_POINT('Ctrl Pts',(-1.22302031683542,-3.6763861302258,60.19993566902));
#26031=CARTESIAN_POINT('Ctrl Pts',(-1.34198409077688,-3.64933669785562,
60.19993566902));
#26032=CARTESIAN_POINT('Ctrl Pts',(-1.45935068501764,-3.6164715536994,60.1999356690201));
#26033=CARTESIAN_POINT('Ctrl Pts',(-1.57468060825087,-3.57773092054377,
60.19993566902));
#26034=CARTESIAN_POINT('Ctrl Pts',(-1.59224316998028,-3.57183145627502,
60.19993566902));
#26035=CARTESIAN_POINT('Ctrl Pts',(-1.6097585039616,-3.5657956440463,60.19993566902));
#26036=CARTESIAN_POINT('Ctrl Pts',(-1.62722505555305,-3.55962316586745,
60.1999356690201));
#26037=CARTESIAN_POINT('Ctrl Pts',(-1.7202915870815,-3.52673452542617,60.1999356690201));
#26038=CARTESIAN_POINT('Ctrl Pts',(-1.81197361471366,-3.48996787671853,
60.1999356690201));
#26039=CARTESIAN_POINT('Ctrl Pts',(-1.90215316220673,-3.44952007606408,
60.1999356690201));
#26040=CARTESIAN_POINT('Origin',(-1.041818884589E-14,0.,50.1419356690201));
#26041=CARTESIAN_POINT('Origin',(-1.16499385964724E-14,0.,60.1999356690201));
#26042=CARTESIAN_POINT('',(0.,0.,0.));
#26043=CARTESIAN_POINT('Origin',(0.,0.,-25.2396150285955));
#26044=CARTESIAN_POINT('',(2.48705727606859,3.24064362520075,-38.7031482120265));
#26045=CARTESIAN_POINT('',(2.49067940755002,3.24534996886546,-38.8073295092502));
#26046=CARTESIAN_POINT('',(2.4870572760686,3.24064362520075,-25.2396150285955));
#26047=CARTESIAN_POINT('',(4.07943565862452,-0.213142457391218,-39.));
#26048=CARTESIAN_POINT('Ctrl Pts',(2.49067940755052,3.24534996886507,-38.8073295092502));
#26049=CARTESIAN_POINT('Ctrl Pts',(3.52935397857082,2.44593384313725,-38.8715530061668));
#26050=CARTESIAN_POINT('Ctrl Pts',(4.14824284080374,1.10379118401926,-38.9357765030834));
#26051=CARTESIAN_POINT('Ctrl Pts',(4.07943565862452,-0.213142457391218,
-39.));
#26052=CARTESIAN_POINT('',(3.42517145598067,-2.22607850201542,-38.9999998622677));
#26053=CARTESIAN_POINT('Origin',(0.,0.,-39.));
#26054=CARTESIAN_POINT('Ctrl Pts',(2.48705727606859,3.24064362520075,-38.7031482120265));
#26055=CARTESIAN_POINT('Ctrl Pts',(2.58203140296112,3.16775498928613,-38.7089631647656));
#26056=CARTESIAN_POINT('Ctrl Pts',(2.67381530421241,3.09067498482409,-38.7147781175047));
#26057=CARTESIAN_POINT('Ctrl Pts',(2.76202883781055,3.00972119956366,-38.7205930702438));
#26058=CARTESIAN_POINT('Ctrl Pts',(2.85024920780721,2.92876114052283,-38.7264084736318));
#26059=CARTESIAN_POINT('Ctrl Pts',(2.93489836057956,2.84392697867096,-38.7322238770199));
#26060=CARTESIAN_POINT('Ctrl Pts',(3.0156317065863,2.75557442473097,-38.7380392804079));
#26061=CARTESIAN_POINT('Ctrl Pts',(3.096390141849,2.66719441373697,-38.7438564910311));
#26062=CARTESIAN_POINT('Ctrl Pts',(3.17323007601772,2.57529413591597,-38.7496737016544));
#26063=CARTESIAN_POINT('Ctrl Pts',(3.24584644002518,2.48026326985179,-38.7554909122776));
#26064=CARTESIAN_POINT('Ctrl Pts',(3.31854039094952,2.3851308681075,-38.7613143382965));
#26065=CARTESIAN_POINT('Ctrl Pts',(3.38700151711333,2.286861524617,-38.7671377643155));
#26066=CARTESIAN_POINT('Ctrl Pts',(3.45096734123387,2.18587497577908,-38.7729611903344));
#26067=CARTESIAN_POINT('Ctrl Pts',(3.51497417259674,2.08482368643423,-38.7787883496382));
#26068=CARTESIAN_POINT('Ctrl Pts',(3.5744797600348,1.98105207395486,-38.784615508942));
#26069=CARTESIAN_POINT('Ctrl Pts',(3.62926773202761,1.87500419446549,-38.7904426682458));
#26070=CARTESIAN_POINT('Ctrl Pts',(3.68413107705314,1.76881042254755,-38.7962778441023));
#26071=CARTESIAN_POINT('Ctrl Pts',(3.73426368290503,1.66033450106111,-38.8021130199589));
#26072=CARTESIAN_POINT('Ctrl Pts',(3.77949735438832,1.55004024082334,-38.8079481958155));
#26073=CARTESIAN_POINT('Ctrl Pts',(3.7891274022615,1.52655908239872,-38.8091904788538));
#26074=CARTESIAN_POINT('Ctrl Pts',(3.79853558888994,1.5029955610706,-38.8104327618922));
#26075=CARTESIAN_POINT('Ctrl Pts',(3.80772058580551,1.4793542308835,-38.8116750449306));
#26076=CARTESIAN_POINT('Ctrl Pts',(3.85054135128359,1.36913755200637,-38.8174666103641));
#26077=CARTESIAN_POINT('Ctrl Pts',(3.88864421705721,1.25687596525225,-38.8232581757977));
#26078=CARTESIAN_POINT('Ctrl Pts',(3.92182946063559,1.14301298404293,-38.8290497412312));
#26079=CARTESIAN_POINT('Ctrl Pts',(3.95497352447858,1.02929129597876,-38.8348341198822));
#26080=CARTESIAN_POINT('Ctrl Pts',(3.98321198630328,0.913972558369433,-38.8406184985331));
#26081=CARTESIAN_POINT('Ctrl Pts',(4.00639324377989,0.797520016171896,-38.846402877184));
#26082=CARTESIAN_POINT('Ctrl Pts',(4.02955195414875,0.681180740824569,-38.8521816296946));
#26083=CARTESIAN_POINT('Ctrl Pts',(4.04766316351743,0.563710257410262,-38.8579603822051));
#26084=CARTESIAN_POINT('Ctrl Pts',(4.06062532717396,0.445586077333446,-38.8637391347157));
#26085=CARTESIAN_POINT('Ctrl Pts',(4.0735787196456,0.327541829052746,-38.8695139768832));
#26086=CARTESIAN_POINT('Ctrl Pts',(4.08138995193574,0.208845173517891,-38.8752888190507));
#26087=CARTESIAN_POINT('Ctrl Pts',(4.08400883807448,0.0899822789749685,
-38.8810636612182));
#26088=CARTESIAN_POINT('Ctrl Pts',(4.08662679830471,-0.0288385915317061,
-38.8868364616873));
#26089=CARTESIAN_POINT('Ctrl Pts',(4.08405605265242,-0.147825171524291,
-38.8926092621564));
#26090=CARTESIAN_POINT('Ctrl Pts',(4.07629844063419,-0.266488316598069,
-38.8983820626256));
#26091=CARTESIAN_POINT('Ctrl Pts',(4.06854168767119,-0.385138321262834,
-38.9041542238317));
#26092=CARTESIAN_POINT('Ctrl Pts',(4.0555992376166,-0.503464549876765,-38.9099263850378));
#26093=CARTESIAN_POINT('Ctrl Pts',(4.03752497766301,-0.620980720109175,
-38.9156985462439));
#26094=CARTESIAN_POINT('Ctrl Pts',(4.01944833046838,-0.738512411830461,
-38.9214714698348));
#26095=CARTESIAN_POINT('Ctrl Pts',(3.99623858913628,-0.855233424042061,
-38.9272443934257));
#26096=CARTESIAN_POINT('Ctrl Pts',(3.96800103914963,-0.970666138951715,
-38.9330173170165));
#26097=CARTESIAN_POINT('Ctrl Pts',(3.93973585225294,-1.08621183121103,-38.9387958907353));
#26098=CARTESIAN_POINT('Ctrl Pts',(3.90643312665145,-1.20046630562591,-38.9445744644541));
#26099=CARTESIAN_POINT('Ctrl Pts',(3.86824853021083,-1.31296546356776,-38.9503530381729));
#26100=CARTESIAN_POINT('Ctrl Pts',(3.83004492559059,-1.42552062325906,-38.9561344884487));
#26101=CARTESIAN_POINT('Ctrl Pts',(3.78695475915395,-1.53631834078466,-38.9619159387245));
#26102=CARTESIAN_POINT('Ctrl Pts',(3.73918186636588,-1.64491457840235,-38.9676973890003));
#26103=CARTESIAN_POINT('Ctrl Pts',(3.69133422795344,-1.75368072604874,-38.9734878849521));
#26104=CARTESIAN_POINT('Ctrl Pts',(3.63878940876722,-1.86023814152513,-38.9792783809039));
#26105=CARTESIAN_POINT('Ctrl Pts',(3.5817974250089,-1.96416705150035,-38.9850688768557));
#26106=CARTESIAN_POINT('Ctrl Pts',(3.53281218637065,-2.0534950959169,-38.990045871993));
#26107=CARTESIAN_POINT('Ctrl Pts',(3.48054239181174,-2.14088161936829,-38.9950228671304));
#26108=CARTESIAN_POINT('Ctrl Pts',(3.42517145598068,-2.22607850201542,-38.9999998622677));
#26109=CARTESIAN_POINT('Origin',(0.,0.,-25.2396150285955));
#26110=CARTESIAN_POINT('',(2.48705727606859,3.24064362520075,-37.4531876190354));
#26111=CARTESIAN_POINT('',(2.4870572760686,3.24064362520074,-37.5572541797712));
#26112=CARTESIAN_POINT('',(2.4870572760686,3.24064362520075,-25.2396150285955));
#26113=CARTESIAN_POINT('',(-4.08499877004747,0.0031699701342642,-38.3646150285955));
#26114=CARTESIAN_POINT('Ctrl Pts',(2.4870572760686,3.24064362520074,-37.5572541797712));
#26115=CARTESIAN_POINT('Ctrl Pts',(2.58191367553083,3.16784534012255,-37.5630654428848));
#26116=CARTESIAN_POINT('Ctrl Pts',(2.67352246407981,3.09091617849925,-37.5688767059985));
#26117=CARTESIAN_POINT('Ctrl Pts',(2.76151875527619,3.01018922399537,-37.5746879691121));
#26118=CARTESIAN_POINT('Ctrl Pts',(2.84956217068161,2.92941903819358,-37.5805023443021));
#26119=CARTESIAN_POINT('Ctrl Pts',(2.9339889461399,2.84484729630921,-37.5863167194922));
#26120=CARTESIAN_POINT('Ctrl Pts',(3.01447201343793,2.75684302784897,-37.5921310946822));
#26121=CARTESIAN_POINT('Ctrl Pts',(3.09508237545809,2.66869956888225,-37.5979546660833));
#26122=CARTESIAN_POINT('Ctrl Pts',(3.171736305253,2.57711304979982,-37.6037782374843));
#26123=CARTESIAN_POINT('Ctrl Pts',(3.24414755374533,2.48248497468327,-37.6096018088854));
#26124=CARTESIAN_POINT('Ctrl Pts',(3.30369403183372,2.40466876906888,-37.614390749472));
#26125=CARTESIAN_POINT('Ctrl Pts',(3.36037217691526,2.32479640134805,-37.6191796900586));
#26126=CARTESIAN_POINT('Ctrl Pts',(3.41404578623918,2.2431041815891,-37.6239686306452));
#26127=CARTESIAN_POINT('Ctrl Pts',(3.47934871858892,2.14371191847105,-37.6297951786842));
#26128=CARTESIAN_POINT('Ctrl Pts',(3.54041199454479,2.04130679768247,-37.6356217267232));
#26129=CARTESIAN_POINT('Ctrl Pts',(3.59694625009755,1.93628579344816,-37.6414482747623));
#26130=CARTESIAN_POINT('Ctrl Pts',(3.65340951727827,1.8313966609445,-37.6472675065793));
#26131=CARTESIAN_POINT('Ctrl Pts',(3.70535488395295,1.7238985343542,-37.6530867383964));
#26132=CARTESIAN_POINT('Ctrl Pts',(3.75253602496439,1.61421757559025,-37.6589059702135));
#26133=CARTESIAN_POINT('Ctrl Pts',(3.79967018289017,1.50464583737016,-37.6647194072266));
#26134=CARTESIAN_POINT('Ctrl Pts',(3.84204939321694,1.39289596388548,-37.6705328442396));
#26135=CARTESIAN_POINT('Ctrl Pts',(3.87947335467167,1.27941841881089,-37.6763462812527));
#26136=CARTESIAN_POINT('Ctrl Pts',(3.91815149296423,1.16213793831432,-37.6823545420568));
#26137=CARTESIAN_POINT('Ctrl Pts',(3.95153621012533,1.04301234482587,-37.688362802861));
#26138=CARTESIAN_POINT('Ctrl Pts',(3.97946042882905,0.922561485963775,-37.6943710636652));
#26139=CARTESIAN_POINT('Ctrl Pts',(4.00644899369114,0.806146561285478,-37.7001780063103));
#26140=CARTESIAN_POINT('Ctrl Pts',(4.02833702888313,0.688494188699189,-37.7059849489554));
#26141=CARTESIAN_POINT('Ctrl Pts',(4.04502465962916,0.570088153702579,-37.7117918916005));
#26142=CARTESIAN_POINT('Ctrl Pts',(4.06170984580576,0.45169946399464,-37.7175979835872));
#26143=CARTESIAN_POINT('Ctrl Pts',(4.0731960857049,0.332557735198908,-37.7234040755738));
#26144=CARTESIAN_POINT('Ctrl Pts',(4.07943501693327,0.213154738672663,-37.7292101675604));
#26145=CARTESIAN_POINT('Ctrl Pts',(4.08567450227854,0.0937411372504796,
-37.7350167752209));
#26146=CARTESIAN_POINT('Ctrl Pts',(4.08666573107,-0.0259333707249715,-37.7408233828814));
#26147=CARTESIAN_POINT('Ctrl Pts',(4.08241242132786,-0.145374764618867,
-37.7466299905419));
#26148=CARTESIAN_POINT('Ctrl Pts',(4.07815773300344,-0.264854871844148,
-37.7524384802394));
#26149=CARTESIAN_POINT('Ctrl Pts',(4.06865513996115,-0.384101307339019,
-37.7582469699369));
#26150=CARTESIAN_POINT('Ctrl Pts',(4.05396035404529,-0.502623564737019,
-37.7640554596344));
#26151=CARTESIAN_POINT('Ctrl Pts',(4.03924943015729,-0.621275984554532,
-37.7698703282779));
#26152=CARTESIAN_POINT('Ctrl Pts',(4.01933498187758,-0.739202233838021,
-37.7756851969213));
#26153=CARTESIAN_POINT('Ctrl Pts',(3.9943241614115,-0.855920261218504,-37.7815000655648));
#26154=CARTESIAN_POINT('Ctrl Pts',(3.96929693958899,-0.972714828829665,
-37.7873187474271));
#26155=CARTESIAN_POINT('Ctrl Pts',(3.93916679224495,-1.08829920282149,-37.7931374292895));
#26156=CARTESIAN_POINT('Ctrl Pts',(3.90409077974541,-1.20220638141163,-37.7989561111518));
#26157=CARTESIAN_POINT('Ctrl Pts',(3.86896522204763,-1.31627445496511,-37.8047830119571));
#26158=CARTESIAN_POINT('Ctrl Pts',(3.82887999235549,-1.42866022202432,-37.8106099127624));
#26159=CARTESIAN_POINT('Ctrl Pts',(3.78404033163829,-1.53891642675447,-37.8164368135677));
#26160=CARTESIAN_POINT('Ctrl Pts',(3.77350362207393,-1.56482513320607,-37.8178060558962));
#26161=CARTESIAN_POINT('Ctrl Pts',(3.76270457892702,-1.59061635614294,-37.8191752982246));
#26162=CARTESIAN_POINT('Ctrl Pts',(3.75164622762479,-1.61628449932204,-37.820544540553));
#26163=CARTESIAN_POINT('Ctrl Pts',(3.70458780895145,-1.72551436508384,-37.8263713023365));
#26164=CARTESIAN_POINT('Ctrl Pts',(3.65268010714795,-1.83286134077567,-37.83219806412));
#26165=CARTESIAN_POINT('Ctrl Pts',(3.59609550443534,-1.93786535212846,-37.8380248259034));
#26166=CARTESIAN_POINT('Ctrl Pts',(3.53958176345365,-2.04273786541213,-37.8438442907474));
#26167=CARTESIAN_POINT('Ctrl Pts',(3.47840296306761,-2.14527289457213,-37.8496637555913));
#26168=CARTESIAN_POINT('Ctrl Pts',(3.41277953405773,-2.24503025634772,-37.8554832204352));
#26169=CARTESIAN_POINT('Ctrl Pts',(3.34722123913477,-2.3446886046342,-37.861296909209));
#26170=CARTESIAN_POINT('Ctrl Pts',(3.27722731483667,-2.44157443156378,-37.8671105979828));
#26171=CARTESIAN_POINT('Ctrl Pts',(3.20306380202618,-2.53527262442318,-37.8729242867566));
#26172=CARTESIAN_POINT('Ctrl Pts',(3.12641930508808,-2.63210529298986,-37.8789324602442));
#26173=CARTESIAN_POINT('Ctrl Pts',(3.04532156827027,-2.72553292565708,-37.8849406337319));
#26174=CARTESIAN_POINT('Ctrl Pts',(2.96011278962525,-2.81513006319371,-37.8909488072196));
#26175=CARTESIAN_POINT('Ctrl Pts',(2.87775369479293,-2.9017307546298,-37.8967560460735));
#26176=CARTESIAN_POINT('Ctrl Pts',(2.79155444190347,-2.98475274771809,-37.9025632849274));
#26177=CARTESIAN_POINT('Ctrl Pts',(2.7018641382783,-3.06384646780573,-37.9083705237813));
#26178=CARTESIAN_POINT('Ctrl Pts',(2.61218672843152,-3.14292881746806,-37.914176927793));
#26179=CARTESIAN_POINT('Ctrl Pts',(2.51901957173523,-3.21808374759441,-37.9199833318047));
#26180=CARTESIAN_POINT('Ctrl Pts',(2.42274677984221,-3.28900031024082,-37.9257897358164));
#26181=CARTESIAN_POINT('Ctrl Pts',(2.32646518265715,-3.35992335905047,-37.9315966708928));
#26182=CARTESIAN_POINT('Ctrl Pts',(2.22707771385739,-3.42660702776142,-37.9374036059692));
#26183=CARTESIAN_POINT('Ctrl Pts',(2.12499901165192,-3.48878262442336,-37.9432105410456));
#26184=CARTESIAN_POINT('Ctrl Pts',(2.0228869623055,-3.55097853265217,-37.9490193731356));
#26185=CARTESIAN_POINT('Ctrl Pts',(1.9180822791219,-3.60866322786948,-37.9548282052256));
#26186=CARTESIAN_POINT('Ctrl Pts',(1.81102526660694,-3.66161337168621,-37.9606370373156));
#26187=CARTESIAN_POINT('Ctrl Pts',(1.70385031760053,-3.71462184661117,-37.9664522685499));
#26188=CARTESIAN_POINT('Ctrl Pts',(1.59441845235195,-3.7628851784569,-37.9722674997842));
#26189=CARTESIAN_POINT('Ctrl Pts',(1.4831912131835,-3.80622763706209,-37.9780827310185));
#26190=CARTESIAN_POINT('Ctrl Pts',(1.37189080576485,-3.84959860749477,-37.9839017876674));
#26191=CARTESIAN_POINT('Ctrl Pts',(1.25879305747633,-3.88804212683319,-37.9897208443162));
#26192=CARTESIAN_POINT('Ctrl Pts',(1.14437439735977,-3.92143242179021,-37.995539900965));
#26193=CARTESIAN_POINT('Ctrl Pts',(1.02979383999381,-3.95486996251034,-38.0013671913168));
#26194=CARTESIAN_POINT('Ctrl Pts',(0.9138890351005,-3.98323991156655,-38.0071944816687));
#26195=CARTESIAN_POINT('Ctrl Pts',(0.797146427651654,-4.00646759289055,
-38.0130217720205));
#26196=CARTESIAN_POINT('Ctrl Pts',(0.769775764253665,-4.0119133942216,-38.0143879981673));
#26197=CARTESIAN_POINT('Ctrl Pts',(0.742359067800449,-4.01707675908078,
-38.0157542243141));
#26198=CARTESIAN_POINT('Ctrl Pts',(0.714902633431441,-4.02195713859718,
-38.0171204504609));
#26199=CARTESIAN_POINT('Ctrl Pts',(0.597972576197206,-4.04274144906181,
-38.0229388644397));
#26200=CARTESIAN_POINT('Ctrl Pts',(0.479945563511625,-4.0584560111944,-38.0287572784184));
#26201=CARTESIAN_POINT('Ctrl Pts',(0.361299229961964,-4.06899101331385,
-38.0345756923972));
#26202=CARTESIAN_POINT('Ctrl Pts',(0.242802307684981,-4.07951274871004,
-38.04038677925));
#26203=CARTESIAN_POINT('Ctrl Pts',(0.123688019616775,-4.08486786109853,
-38.0461978661028));
#26204=CARTESIAN_POINT('Ctrl Pts',(0.00444393378988152,-4.0849975827964,
-38.0520089529555));
#26205=CARTESIAN_POINT('Ctrl Pts',(-0.11468121592749,-4.08512717510762,
-38.05781424373));
#26206=CARTESIAN_POINT('Ctrl Pts',(-0.233935499099669,-4.08004174435223,
-38.0636195345044));
#26207=CARTESIAN_POINT('Ctrl Pts',(-0.352827096490942,-4.06973439427953,
-38.0694248252788));
#26208=CARTESIAN_POINT('Ctrl Pts',(-0.475938021876412,-4.05906124803905,
-38.0754361392409));
#26209=CARTESIAN_POINT('Ctrl Pts',(-0.59865959577594,-4.0427886210935,-38.081447453203));
#26210=CARTESIAN_POINT('Ctrl Pts',(-0.720446289394505,-4.02096781187038,
-38.087458767165));
#26211=CARTESIAN_POINT('Ctrl Pts',(-0.837928434466314,-3.99991825876597,
-38.0932576113407));
#26212=CARTESIAN_POINT('Ctrl Pts',(-0.954540230615088,-3.973706162567,-38.0990564555164));
#26213=CARTESIAN_POINT('Ctrl Pts',(-1.06979876696172,-3.94243016402411,
-38.1048552996921));
#26214=CARTESIAN_POINT('Ctrl Pts',(-1.18504102029999,-3.91115858395956,
-38.1106533246432));
#26215=CARTESIAN_POINT('Ctrl Pts',(-1.2989299992701,-3.87482463129699,-38.1164513495942));
#26216=CARTESIAN_POINT('Ctrl Pts',(-1.41099576212991,-3.83357743618822,
-38.1222493745453));
#26217=CARTESIAN_POINT('Ctrl Pts',(-1.5230722653205,-3.79232628796738,-38.1280479551764));
#26218=CARTESIAN_POINT('Ctrl Pts',(-1.63332482102462,-3.74616110239697,
-38.1338465358075));
#26219=CARTESIAN_POINT('Ctrl Pts',(-1.74130196855822,-3.6952797531845,-38.1396451164386));
#26220=CARTESIAN_POINT('Ctrl Pts',(-1.84931506733781,-3.64438146290678,
-38.1454456277208));
#26221=CARTESIAN_POINT('Ctrl Pts',(-1.95505088140968,-3.58876406050027,
-38.151246139003));
#26222=CARTESIAN_POINT('Ctrl Pts',(-2.05808170810105,-3.52867180151114,
-38.1570466502852));
#26223=CARTESIAN_POINT('Ctrl Pts',(-2.16122781774006,-3.46851230426945,
-38.1628536518583));
#26224=CARTESIAN_POINT('Ctrl Pts',(-2.26166254517085,-3.40386816266328,
-38.1686606534315));
#26225=CARTESIAN_POINT('Ctrl Pts',(-2.3589862701395,-3.33502755270378,-38.1744676550046));
#26226=CARTESIAN_POINT('Ctrl Pts',(-2.45637483884643,-3.26614107641007,
-38.1802785256003));
#26227=CARTESIAN_POINT('Ctrl Pts',(-2.55064795489363,-3.19305281395483,
-38.186089396196));
#26228=CARTESIAN_POINT('Ctrl Pts',(-2.64143955913574,-3.11609082913717,
-38.1919002667917));
#26229=CARTESIAN_POINT('Ctrl Pts',(-2.73236176628603,-3.0390181351948,-38.1977194962726));
#26230=CARTESIAN_POINT('Ctrl Pts',(-2.81979216729412,-2.95806087447145,
-38.2035387257535));
#26231=CARTESIAN_POINT('Ctrl Pts',(-2.90340189323373,-2.87358355479126,
-38.2093579552345));
#26232=CARTESIAN_POINT('Ctrl Pts',(-2.92417972218139,-2.85259012037265,
-38.2108040902792));
#26233=CARTESIAN_POINT('Ctrl Pts',(-2.94472179518781,-2.83137945338585,
-38.2122502253239));
#26234=CARTESIAN_POINT('Ctrl Pts',(-2.96502346430134,-2.80995744738999,
-38.2136963603687));
#26235=CARTESIAN_POINT('Ctrl Pts',(-3.04596507285138,-2.72454911894286,
-38.2194620191451));
#26236=CARTESIAN_POINT('Ctrl Pts',(-3.12335661032414,-2.63548923203773,
-38.2252276779216));
#26237=CARTESIAN_POINT('Ctrl Pts',(-3.19684629131144,-2.54310809635145,
-38.2309933366981));
#26238=CARTESIAN_POINT('Ctrl Pts',(-3.27022120562092,-2.45087122957331,
-38.2367499914144));
#26239=CARTESIAN_POINT('Ctrl Pts',(-3.33970613289259,-2.35532376030525,
-38.2425066461308));
#26240=CARTESIAN_POINT('Ctrl Pts',(-3.40498643381326,-2.25683237869976,
-38.2482633008472));
#26241=CARTESIAN_POINT('Ctrl Pts',(-3.47020838077286,-2.15842903838954,
-38.2540148096988));
#26242=CARTESIAN_POINT('Ctrl Pts',(-3.53123294188016,-2.05708736147524,
-38.2597663185503));
#26243=CARTESIAN_POINT('Ctrl Pts',(-3.58778614809329,-1.95320648052117,
-38.2655178274018));
#26244=CARTESIAN_POINT('Ctrl Pts',(-3.6443028410371,-1.84939266969164,-38.271265622823));
#26245=CARTESIAN_POINT('Ctrl Pts',(-3.69635371924347,-1.74304327941579,
-38.2770134182442));
#26246=CARTESIAN_POINT('Ctrl Pts',(-3.74370892814126,-1.63458510373593,
-38.2827612136654));
#26247=CARTESIAN_POINT('Ctrl Pts',(-3.79104531624626,-1.52617003353273,
-38.2885067246903));
#26248=CARTESIAN_POINT('Ctrl Pts',(-3.83368958006656,-1.41564822698566,
-38.2942522357151));
#26249=CARTESIAN_POINT('Ctrl Pts',(-3.87145884581187,-1.30346898896177,
-38.29999774674));
#26250=CARTESIAN_POINT('Ctrl Pts',(-3.90923391853051,-1.19127250353233,
-38.3057441411294));
#26251=CARTESIAN_POINT('Ctrl Pts',(-3.94213235272038,-1.07741847010478,
-38.3114905355187));
#26252=CARTESIAN_POINT('Ctrl Pts',(-3.97002039009557,-0.962373681178677,
-38.3172369299081));
#26253=CARTESIAN_POINT('Ctrl Pts',(-3.99790992310238,-0.847322722416304,
-38.3229836324758));
#26254=CARTESIAN_POINT('Ctrl Pts',(-4.0207884337351,-0.731081288926688,
-38.3287303350435));
#26255=CARTESIAN_POINT('Ctrl Pts',(-4.03857306524437,-0.614127508488797,
-38.3344770376112));
#26256=CARTESIAN_POINT('Ctrl Pts',(-4.05637201751117,-0.497079553103854,
-38.3402283676088));
#26257=CARTESIAN_POINT('Ctrl Pts',(-4.06906884303718,-0.379318519535031,
-38.3459796976063));
#26258=CARTESIAN_POINT('Ctrl Pts',(-4.07663246715613,-0.261328773250282,
-38.3517310276038));
#26259=CARTESIAN_POINT('Ctrl Pts',(-4.08228042108977,-0.173222775229081,
-38.356025694601));
#26260=CARTESIAN_POINT('Ctrl Pts',(-4.08506718194844,-0.0849893876783897,
-38.3603203615983));
#26261=CARTESIAN_POINT('Ctrl Pts',(-4.08499877004747,0.0031699701342642,
-38.3646150285955));
#26262=CARTESIAN_POINT('Ctrl Pts',(-4.0847807681364,0.00317176647937747,
-38.3646151243503));
#26263=CARTESIAN_POINT('Ctrl Pts',(-4.08755373173903,0.315568510627117,
-38.3798341729923));
#26264=CARTESIAN_POINT('Ctrl Pts',(-3.91319964322216,1.97007722952994,-38.4605785249371));
#26265=CARTESIAN_POINT('Ctrl Pts',(-1.66658153270677,4.5182208917146,-38.6068481801843));
#26266=CARTESIAN_POINT('Ctrl Pts',(1.37998923899127,4.08193142921117,-38.7392005931756));
#26267=CARTESIAN_POINT('Ctrl Pts',(2.46962553701302,3.26155408523247,-38.8060277028642));
#26268=CARTESIAN_POINT('Ctrl Pts',(2.49067940755052,3.24534996886507,-38.8073295092502));
#26269=CARTESIAN_POINT('',(-4.0849985769777,-0.00340970529112389,-38.2603849714395));
#26270=CARTESIAN_POINT('Ctrl Pts',(-4.0849985769777,-0.0034097052911255,
-38.2603849714395));
#26271=CARTESIAN_POINT('Ctrl Pts',(-4.08509671274173,0.114161879992395,
-38.2661197666967));
#26272=CARTESIAN_POINT('Ctrl Pts',(-4.08011485793121,0.23189389784994,-38.271854561954));
#26273=CARTESIAN_POINT('Ctrl Pts',(-4.07003816185633,0.349305541085676,
-38.2775893572112));
#26274=CARTESIAN_POINT('Ctrl Pts',(-4.05971995163102,0.469531258801339,
-38.2834616017072));
#26275=CARTESIAN_POINT('Ctrl Pts',(-4.04405951039676,0.589420605878094,
-38.2893338462032));
#26276=CARTESIAN_POINT('Ctrl Pts',(-4.02309759022828,0.708456617937449,
-38.2952060906992));
#26277=CARTESIAN_POINT('Ctrl Pts',(-4.00265473465418,0.824545028879237,
-38.3009329251286));
#26278=CARTESIAN_POINT('Ctrl Pts',(-3.97716996340125,0.939821432329227,
-38.306659759558));
#26279=CARTESIAN_POINT('Ctrl Pts',(-3.94673347793783,1.05381205825554,-38.3123865939874));
#26280=CARTESIAN_POINT('Ctrl Pts',(-3.91630400078119,1.1677764366942,-38.3181121097556));
#26281=CARTESIAN_POINT('Ctrl Pts',(-3.88092518400022,1.28045521990363,-38.3238376255238));
#26282=CARTESIAN_POINT('Ctrl Pts',(-3.84073788806712,1.39138688910228,-38.329563141292));
#26283=CARTESIAN_POINT('Ctrl Pts',(-3.80054973343371,1.50232092862857,-38.3352887794));
#26284=CARTESIAN_POINT('Ctrl Pts',(-3.75555303948203,1.61150738475108,-38.3410144175079));
#26285=CARTESIAN_POINT('Ctrl Pts',(-3.70593760765772,1.71850267621212,-38.3467400556158));
#26286=CARTESIAN_POINT('Ctrl Pts',(-3.65410127539669,1.83028732212992,-38.3527219864074));
#26287=CARTESIAN_POINT('Ctrl Pts',(-3.59722330377182,1.93967961846452,-38.358703917199));
#26288=CARTESIAN_POINT('Ctrl Pts',(-3.53557415443047,2.04620145599676,-38.3646858479906));
#26289=CARTESIAN_POINT('Ctrl Pts',(-3.47648681993481,2.14829680544772,-38.3704192011575));
#26290=CARTESIAN_POINT('Ctrl Pts',(-3.41301717942872,2.24775515243283,-38.3761525543244));
#26291=CARTESIAN_POINT('Ctrl Pts',(-3.34544749077826,2.3441855912972,-38.3818859074913));
#26292=CARTESIAN_POINT('Ctrl Pts',(-3.2778339028369,2.44067867996762,-38.3876229855553));
#26293=CARTESIAN_POINT('Ctrl Pts',(-3.20611522154903,2.5341396135903,-38.3933600636193));
#26294=CARTESIAN_POINT('Ctrl Pts',(-3.13061348641048,2.62421115741566,-38.3990971416833));
#26295=CARTESIAN_POINT('Ctrl Pts',(-3.05500788666663,2.71440660892777,-38.4048421120077));
#26296=CARTESIAN_POINT('Ctrl Pts',(-2.9756091358878,2.80120306273816,-38.410587082332));
#26297=CARTESIAN_POINT('Ctrl Pts',(-2.89277540845927,2.8842807485079,-38.4163320526564));
#26298=CARTESIAN_POINT('Ctrl Pts',(-2.8822442845987,2.89484288818278,-38.4170624434759));
#26299=CARTESIAN_POINT('Ctrl Pts',(-2.87165768176318,2.9053449742801,-38.4177928342954));
#26300=CARTESIAN_POINT('Ctrl Pts',(-2.86101637200142,2.91578639806483,-38.418523225115));
#26301=CARTESIAN_POINT('Ctrl Pts',(-2.77624574557761,2.99896469611309,-38.4243416524225));
#26302=CARTESIAN_POINT('Ctrl Pts',(-2.68770713769223,3.07857813632915,-38.43016007973));
#26303=CARTESIAN_POINT('Ctrl Pts',(-2.59573275325813,3.15426639231105,-38.4359785070375));
#26304=CARTESIAN_POINT('Ctrl Pts',(-2.50387419153435,3.22985933459228,-38.4417896072395));
#26305=CARTESIAN_POINT('Ctrl Pts',(-2.408588771664,3.30153666605369,-38.4476007074415));
#26306=CARTESIAN_POINT('Ctrl Pts',(-2.3102457186713,3.36897457980331,-38.4534118076434));
#26307=CARTESIAN_POINT('Ctrl Pts',(-2.21200075442206,3.43634523002979,-38.4592171117724));
#26308=CARTESIAN_POINT('Ctrl Pts',(-2.11070455936081,3.499484644205,-38.4650224159013));
#26309=CARTESIAN_POINT('Ctrl Pts',(-2.00675915609902,3.55810942628424,-38.4708277200303));
#26310=CARTESIAN_POINT('Ctrl Pts',(-1.89912518552784,3.61881454523179,-38.4768390289883));
#26311=CARTESIAN_POINT('Ctrl Pts',(-1.78865084348428,3.67467839039533,-38.4828503379463));
#26312=CARTESIAN_POINT('Ctrl Pts',(-1.67581533584916,3.72543527123111,-38.4888616469043));
#26313=CARTESIAN_POINT('Ctrl Pts',(-1.56696765723321,3.77439830395504,-38.4946605043672));
#26314=CARTESIAN_POINT('Ctrl Pts',(-1.45592328864224,3.81860906005878,-38.50045936183));
#26315=CARTESIAN_POINT('Ctrl Pts',(-1.34313649121172,3.85787627665474,-38.5062582192929));
#26316=CARTESIAN_POINT('Ctrl Pts',(-1.23036562846781,3.8971379455199,-38.5120562574845));
#26317=CARTESIAN_POINT('Ctrl Pts',(-1.1158532126979,3.93145732928513,-38.5178542956761));
#26318=CARTESIAN_POINT('Ctrl Pts',(-1.00007130982692,3.96069215860827,-38.5236523338678));
#26319=CARTESIAN_POINT('Ctrl Pts',(-0.884278311697346,3.98992978947452,
-38.5294509276793));
#26320=CARTESIAN_POINT('Ctrl Pts',(-0.767215981280507,4.01408179697358,
-38.5352495214909));
#26321=CARTESIAN_POINT('Ctrl Pts',(-0.649368654361985,4.03305657668376,
-38.5410481153024));
#26322=CARTESIAN_POINT('Ctrl Pts',(-0.531482091484585,4.05203767383613,
-38.5468486396914));
#26323=CARTESIAN_POINT('Ctrl Pts',(-0.412810416039433,4.0658380502612,-38.5526491640804));
#26324=CARTESIAN_POINT('Ctrl Pts',(-0.293844544922322,4.07441779686612,
-38.5584496884694));
#26325=CARTESIAN_POINT('Ctrl Pts',(-0.174745564709313,4.08300714321846,
-38.5642567029765));
#26326=CARTESIAN_POINT('Ctrl Pts',(-0.0553521400692684,4.08636417104349,
-38.5700637174836));
#26327=CARTESIAN_POINT('Ctrl Pts',(0.0638431898660881,4.08450107688904,
-38.5758707319907));
#26328=CARTESIAN_POINT('Ctrl Pts',(0.18311793397613,4.08263674144363,-38.5816816154352));
#26329=CARTESIAN_POINT('Ctrl Pts',(0.302193913172875,4.07554538240647,-38.5874924988797));
#26330=CARTESIAN_POINT('Ctrl Pts',(0.420583764816697,4.06329106719819,-38.5933033823241));
#26331=CARTESIAN_POINT('Ctrl Pts',(0.539143914326865,4.05101912477183,-38.5991226244331));
#26332=CARTESIAN_POINT('Ctrl Pts',(0.657015563335642,4.0335694636176,-38.6049418665421));
#26333=CARTESIAN_POINT('Ctrl Pts',(0.773721465431621,4.01105722895228,-38.6107611086511));
#26334=CARTESIAN_POINT('Ctrl Pts',(0.802721420611276,4.00546322055542,-38.6122071174416));
#26335=CARTESIAN_POINT('Ctrl Pts',(0.831649470699675,3.99955685873833,-38.6136531262322));
#26336=CARTESIAN_POINT('Ctrl Pts',(0.860498453699164,3.99334038258465,-38.6150991350227));
#26337=CARTESIAN_POINT('Ctrl Pts',(0.976932508413389,3.96825077978584,-38.6209352044134));
#26338=CARTESIAN_POINT('Ctrl Pts',(1.09245176881673,3.93802512916553,-38.6267712738042));
#26339=CARTESIAN_POINT('Ctrl Pts',(1.20657033769348,3.90274429346815,-38.6326073431949));
#26340=CARTESIAN_POINT('Ctrl Pts',(1.32151675195873,3.86720752153339,-38.6384857489308));
#26341=CARTESIAN_POINT('Ctrl Pts',(1.43504165260818,3.82654194086775,-38.6443641546668));
#26342=CARTESIAN_POINT('Ctrl Pts',(1.54665721385476,3.78088302686436,-38.6502425604028));
#26343=CARTESIAN_POINT('Ctrl Pts',(1.65720292447244,3.73566175988184,-38.6560646208048));
#26344=CARTESIAN_POINT('Ctrl Pts',(1.76587534697202,3.68554260494187,-38.6618866812068));
#26345=CARTESIAN_POINT('Ctrl Pts',(1.87221503303746,3.63070735120149,-38.6677087416088));
#26346=CARTESIAN_POINT('Ctrl Pts',(1.9800984368018,3.57507606208754,-38.6736153200117));
#26347=CARTESIAN_POINT('Ctrl Pts',(2.08558043486308,3.51459078972929,-38.6795218984147));
#26348=CARTESIAN_POINT('Ctrl Pts',(2.18820258457837,3.44949191169432,-38.6854284768176));
#26349=CARTESIAN_POINT('Ctrl Pts',(2.29082473429369,3.38439303365934,-38.6913350552206));
#26350=CARTESIAN_POINT('Ctrl Pts',(2.39058665078402,3.31468076050162,-38.6972416336235));
#26351=CARTESIAN_POINT('Ctrl Pts',(2.48705727606859,3.24064362520075,-38.7031482120265));
#26352=CARTESIAN_POINT('Ctrl Pts',(2.48705727606859,3.24064362520075,-37.4531876190354));
#26353=CARTESIAN_POINT('Ctrl Pts',(2.58154277521058,3.16812999047195,-37.4590058394181));
#26354=CARTESIAN_POINT('Ctrl Pts',(2.67297790338995,3.09138577162844,-37.4648240598007));
#26355=CARTESIAN_POINT('Ctrl Pts',(2.76096338435899,3.01069862162073,-37.4706422801834));
#26356=CARTESIAN_POINT('Ctrl Pts',(2.84886139384849,2.93009168739763,-37.4764547163351));
#26357=CARTESIAN_POINT('Ctrl Pts',(2.93331627983204,2.84554989453595,-37.4822671524868));
#26358=CARTESIAN_POINT('Ctrl Pts',(3.01396078333165,2.75740192872546,-37.4880795886384));
#26359=CARTESIAN_POINT('Ctrl Pts',(3.09728856948325,2.66632101773949,-37.4940854218403));
#26360=CARTESIAN_POINT('Ctrl Pts',(3.17654763178238,2.57139004090815,-37.5000912550422));
#26361=CARTESIAN_POINT('Ctrl Pts',(3.25137283605238,2.47301429049262,-37.5060970882441));
#26362=CARTESIAN_POINT('Ctrl Pts',(3.32370804148694,2.37791224318769,-37.5119030620828));
#26363=CARTESIAN_POINT('Ctrl Pts',(3.39189952608906,2.27959139420542,-37.5177090359214));
#26364=CARTESIAN_POINT('Ctrl Pts',(3.45565796493207,2.17845198005408,-37.5235150097601));
#26365=CARTESIAN_POINT('Ctrl Pts',(3.51940720336462,2.07732716042766,-37.5293201457905));
#26366=CARTESIAN_POINT('Ctrl Pts',(3.57872445071442,1.97338492955952,-37.535125281821));
#26367=CARTESIAN_POINT('Ctrl Pts',(3.63336409647446,1.86705392060603,-37.5409304178515));
#26368=CARTESIAN_POINT('Ctrl Pts',(3.6880087263778,1.76071321230367,-37.5467360834174));
#26369=CARTESIAN_POINT('Ctrl Pts',(3.73797471985586,1.65198365558448,-37.5525417489833));
#26370=CARTESIAN_POINT('Ctrl Pts',(3.78306305086862,1.54131727854866,-37.5583474145493));
#26371=CARTESIAN_POINT('Ctrl Pts',(3.82816611386769,1.43061474281022,-37.5641549770358));
#26372=CARTESIAN_POINT('Ctrl Pts',(3.86838819097253,1.31797450582789,-37.5699625395224));
#26373=CARTESIAN_POINT('Ctrl Pts',(3.90357912415473,1.20386669588595,-37.5757701020089));
#26374=CARTESIAN_POINT('Ctrl Pts',(3.9388088432354,1.08963312133563,-37.5815840653354));
#26375=CARTESIAN_POINT('Ctrl Pts',(3.96899622984037,0.973929135335255,-37.5873980286619));
#26376=CARTESIAN_POINT('Ctrl Pts',(3.9940415137324,0.857238232104843,-37.5932119919883));
#26377=CARTESIAN_POINT('Ctrl Pts',(4.01910328721948,0.74047050060809,-37.5990297831772));
#26378=CARTESIAN_POINT('Ctrl Pts',(4.03901614768469,0.622714959157353,-37.6048475743661));
#26379=CARTESIAN_POINT('Ctrl Pts',(4.05373201773169,0.50446182057411,-37.6106653655549));
#26380=CARTESIAN_POINT('Ctrl Pts',(4.06846872001307,0.386041279241938,-37.6164913925864));
#26381=CARTESIAN_POINT('Ctrl Pts',(4.07799371587268,0.267122140066809,-37.6223174196179));
#26382=CARTESIAN_POINT('Ctrl Pts',(4.08231096862841,0.14819634076506,-37.6281434466494));
#26383=CARTESIAN_POINT('Ctrl Pts',(4.08331781380324,0.120461141099069,-37.6295021595941));
#26384=CARTESIAN_POINT('Ctrl Pts',(4.08404163839779,0.0927255626395004,
-37.6308608725389));
#26385=CARTESIAN_POINT('Ctrl Pts',(4.08448289814634,0.0649958056342169,
-37.6322195854837));
#26386=CARTESIAN_POINT('Ctrl Pts',(4.08637487043928,-0.0538999969310756,
-37.6380452862279));
#26387=CARTESIAN_POINT('Ctrl Pts',(4.08307412858401,-0.173068543203549,
-37.6438709869722));
#26388=CARTESIAN_POINT('Ctrl Pts',(4.074548991457,-0.29201971888346,-37.6496966877164));
#26389=CARTESIAN_POINT('Ctrl Pts',(4.06603455151596,-0.410821636806022,
-37.655515078478));
#26390=CARTESIAN_POINT('Ctrl Pts',(4.0523087841991,-0.529406323247199,-37.6613334692396));
#26391=CARTESIAN_POINT('Ctrl Pts',(4.03339198666198,-0.647282072925641,
-37.6671518600013));
#26392=CARTESIAN_POINT('Ctrl Pts',(4.01449400599587,-0.765040569524009,
-37.6729644631073));
#26393=CARTESIAN_POINT('Ctrl Pts',(3.99041533198627,-0.882091131739768,
-37.6787770662134));
#26394=CARTESIAN_POINT('Ctrl Pts',(3.96122814319716,-0.997946189703017,
-37.6845896693194));
#26395=CARTESIAN_POINT('Ctrl Pts',(3.93105690298246,-1.11770732220375,-37.6905982454058));
#26396=CARTESIAN_POINT('Ctrl Pts',(3.89542662395564,-1.23619046982341,-37.6966068214921));
#26397=CARTESIAN_POINT('Ctrl Pts',(3.85447479376822,-1.35286697949408,-37.7026153975784));
#26398=CARTESIAN_POINT('Ctrl Pts',(3.81490273676214,-1.46561235548406,-37.7084215291805));
#26399=CARTESIAN_POINT('Ctrl Pts',(3.77036209205679,-1.57667045762548,-37.7142276607826));
#26400=CARTESIAN_POINT('Ctrl Pts',(3.72102769838095,-1.68557938640747,-37.7200337923846));
#26401=CARTESIAN_POINT('Ctrl Pts',(3.67170044924306,-1.79447254315057,-37.7258390831508));
#26402=CARTESIAN_POINT('Ctrl Pts',(3.61758100007945,-1.90121677399024,-37.731644373917));
#26403=CARTESIAN_POINT('Ctrl Pts',(3.55889196242682,-2.00537103793133,-37.7374496646833));
#26404=CARTESIAN_POINT('Ctrl Pts',(3.50019760378482,-2.10953474492607,-37.743255481781));
#26405=CARTESIAN_POINT('Ctrl Pts',(3.43693303321699,-2.21110766270125,-37.7490612988787));
#26406=CARTESIAN_POINT('Ctrl Pts',(3.36936604001376,-2.3096747581428,-37.7548671159764));
#26407=CARTESIAN_POINT('Ctrl Pts',(3.30177701017516,-2.40827400074732,-37.7606748266122));
#26408=CARTESIAN_POINT('Ctrl Pts',(3.22988299753557,-2.50386513500164,-37.766482537248));
#26409=CARTESIAN_POINT('Ctrl Pts',(3.15399380660111,-2.59606395682422,-37.7722902478838));
#26410=CARTESIAN_POINT('Ctrl Pts',(3.07802099064959,-2.68836437583018,-37.778104358244));
#26411=CARTESIAN_POINT('Ctrl Pts',(2.99804446836205,-2.77726470579389,-37.7839184686041));
#26412=CARTESIAN_POINT('Ctrl Pts',(2.91441294484785,-2.86241544624523,-37.7897325789642));
#26413=CARTESIAN_POINT('Ctrl Pts',(2.83072640909019,-2.94762219827053,-37.7955505138063));
#26414=CARTESIAN_POINT('Ctrl Pts',(2.74338038160107,-3.02907417109918,-37.8013684486484));
#26415=CARTESIAN_POINT('Ctrl Pts',(2.65275763747355,-3.10646131745202,-37.8071863834905));
#26416=CARTESIAN_POINT('Ctrl Pts',(2.56200653012263,-3.18395807937268,-37.8130125591874));
#26417=CARTESIAN_POINT('Ctrl Pts',(2.46796976304001,-3.25737827314531,-37.8188387348842));
#26418=CARTESIAN_POINT('Ctrl Pts',(2.37106020636012,-3.32645434326334,-37.824664910581));
#26419=CARTESIAN_POINT('Ctrl Pts',(2.34815821120167,-3.34277863446439,-37.8260417721845));
#26420=CARTESIAN_POINT('Ctrl Pts',(2.32509588605495,-3.35886051195241,-37.827418633788));
#26421=CARTESIAN_POINT('Ctrl Pts',(2.30187887847011,-3.3746968202867,-37.8287954953914));
#26422=CARTESIAN_POINT('Ctrl Pts',(2.20366461610006,-3.44168871560456,-37.8346199947924));
#26423=CARTESIAN_POINT('Ctrl Pts',(2.10236600254592,-3.5044969101477,-37.8404444941933));
#26424=CARTESIAN_POINT('Ctrl Pts',(1.99837463052913,-3.56282526038783,-37.8462689935943));
#26425=CARTESIAN_POINT('Ctrl Pts',(1.89451383237716,-3.62108037226238,-37.8520861796251));
#26426=CARTESIAN_POINT('Ctrl Pts',(1.78796735364336,-3.67486663002221,-37.8579033656559));
#26427=CARTESIAN_POINT('Ctrl Pts',(1.67915672955179,-3.72393040719089,-37.8637205516867));
#26428=CARTESIAN_POINT('Ctrl Pts',(1.57045439961708,-3.77294535346254,-37.8695319481426));
#26429=CARTESIAN_POINT('Ctrl Pts',(1.45949277722068,-3.81724700264141,-37.8753433445985));
#26430=CARTESIAN_POINT('Ctrl Pts',(1.34671850405785,-3.85662731811465,-37.8811547410544));
#26431=CARTESIAN_POINT('Ctrl Pts',(1.23010905677329,-3.89734686072341,-37.8871637687312));
#26432=CARTESIAN_POINT('Ctrl Pts',(1.11156186213879,-3.93280416329357,-37.8931727964081));
#26433=CARTESIAN_POINT('Ctrl Pts',(0.991594234988161,-3.96282296767572,
-37.899181824085));
#26434=CARTESIAN_POINT('Ctrl Pts',(0.875701372069739,-3.99182216740873,
-37.9049867519423));
#26435=CARTESIAN_POINT('Ctrl Pts',(0.75848342851756,-4.01574620389473,-37.9107916797997));
#26436=CARTESIAN_POINT('Ctrl Pts',(0.640422122693153,-4.03448689485605,
-37.9165966076571));
#26437=CARTESIAN_POINT('Ctrl Pts',(0.522377853573187,-4.05322488146296,
-37.9224006978408));
#26438=CARTESIAN_POINT('Ctrl Pts',(0.403490867224466,-4.06678094610007,
-37.9282047880246));
#26439=CARTESIAN_POINT('Ctrl Pts',(0.284251756357326,-4.07509827353989,
-37.9340088782083));
#26440=CARTESIAN_POINT('Ctrl Pts',(0.16500174082723,-4.08341636161648,-37.9398134991881));
#26441=CARTESIAN_POINT('Ctrl Pts',(0.0453999439464807,-4.08649473153917,
-37.9456181201679));
#26442=CARTESIAN_POINT('Ctrl Pts',(-0.0740598973889684,-4.08432860230402,
-37.9514227411477));
#26443=CARTESIAN_POINT('Ctrl Pts',(-0.193558826744508,-4.08216176429761,
-37.9572292614364));
#26444=CARTESIAN_POINT('Ctrl Pts',(-0.312915300296527,-4.07474702170451,
-37.9630357817251));
#26445=CARTESIAN_POINT('Ctrl Pts',(-0.431638205376883,-4.06213163987321,
-37.9688423020138));
#26446=CARTESIAN_POINT('Ctrl Pts',(-0.550492257931542,-4.04950232243729,
-37.9746552364858));
#26447=CARTESIAN_POINT('Ctrl Pts',(-0.668710938938595,-4.03166094186888,
-37.9804681709578));
#26448=CARTESIAN_POINT('Ctrl Pts',(-0.785810709842292,-4.00870634099046,
-37.9862811054297));
#26449=CARTESIAN_POINT('Ctrl Pts',(-0.902987666627895,-3.98573660967158,
-37.992097871476));
#26450=CARTESIAN_POINT('Ctrl Pts',(-1.01904384872924,-3.95764704165268,
-37.9979146375223));
#26451=CARTESIAN_POINT('Ctrl Pts',(-1.13350992009048,-3.92458663569254,
-38.0037314035685));
#26452=CARTESIAN_POINT('Ctrl Pts',(-1.24813853611653,-3.89147928313467,
-38.0095564295671));
#26453=CARTESIAN_POINT('Ctrl Pts',(-1.36117214939061,-3.85338713429346,
-38.0153814555656));
#26454=CARTESIAN_POINT('Ctrl Pts',(-1.47216035055477,-3.81050769612849,
-38.0212064815642));
#26455=CARTESIAN_POINT('Ctrl Pts',(-1.49861272996384,-3.80028802272816,
-38.0225947894759));
#26456=CARTESIAN_POINT('Ctrl Pts',(-1.52494902998922,-3.78979662071743,
-38.0239830973876));
#26457=CARTESIAN_POINT('Ctrl Pts',(-1.55116336329753,-3.77903654657685,
-38.0253714052993));
#26458=CARTESIAN_POINT('Ctrl Pts',(-1.66118149265029,-3.73387792229598,
-38.0311979520825));
#26459=CARTESIAN_POINT('Ctrl Pts',(-1.76940169440656,-3.68383878208755,
-38.0370244988657));
#26460=CARTESIAN_POINT('Ctrl Pts',(-1.87536099697052,-3.62908337339358,
-38.0428510456488));
#26461=CARTESIAN_POINT('Ctrl Pts',(-1.98118724980554,-3.57439671932623,
-38.0486702762224));
#26462=CARTESIAN_POINT('Ctrl Pts',(-2.0847578910019,-3.51500576157751,-38.0544895067959));
#26463=CARTESIAN_POINT('Ctrl Pts',(-2.18562898961654,-3.45112313888505,
-38.0603087373695));
#26464=CARTESIAN_POINT('Ctrl Pts',(-2.28639964077916,-3.38730413051587,
-38.0661221731525));
#26465=CARTESIAN_POINT('Ctrl Pts',(-2.38447575474482,-3.31900257252095,
-38.0719356089356));
#26466=CARTESIAN_POINT('Ctrl Pts',(-2.47943766369157,-3.24647714790474,
-38.0777490447186));
#26467=CARTESIAN_POINT('Ctrl Pts',(-2.57758202805301,-3.17152118105499,
-38.083757305989));
#26468=CARTESIAN_POINT('Ctrl Pts',(-2.67239939373545,-3.09205346904024,
-38.0897655672593));
#26469=CARTESIAN_POINT('Ctrl Pts',(-2.76345833598413,-3.00840871978523,
-38.0957738285297));
#26470=CARTESIAN_POINT('Ctrl Pts',(-2.8514661510376,-2.92756666912177,-38.1015807699856));
#26471=CARTESIAN_POINT('Ctrl Pts',(-2.93596305295684,-2.84282331723503,
-38.1073877114415));
#26472=CARTESIAN_POINT('Ctrl Pts',(-3.01659344417503,-2.75452155420143,
-38.1131946528974));
#26473=CARTESIAN_POINT('Ctrl Pts',(-3.09721202408886,-2.66623272622844,
-38.1190007437118));
#26474=CARTESIAN_POINT('Ctrl Pts',(-3.17396494479635,-2.57438682488607,
-38.1248068345263));
#26475=CARTESIAN_POINT('Ctrl Pts',(-3.24653461441266,-2.47936241752198,
-38.1306129253407));
#26476=CARTESIAN_POINT('Ctrl Pts',(-3.31911072960496,-2.38432957017129,
-38.1364195318472));
#26477=CARTESIAN_POINT('Ctrl Pts',(-3.38750260742348,-2.28611797965193,
-38.1422261383537));
#26478=CARTESIAN_POINT('Ctrl Pts',(-3.45143436962128,-2.18513747672703,
-38.1480327448601));
#26479=CARTESIAN_POINT('Ctrl Pts',(-3.51538685359213,-2.08412424366937,
-38.153841233423));
#26480=CARTESIAN_POINT('Ctrl Pts',(-3.57487612881596,-1.98034065773014,
-38.1596497219859));
#26481=CARTESIAN_POINT('Ctrl Pts',(-3.62967121358454,-1.87422300734884,
-38.1654582105487));
#26482=CARTESIAN_POINT('Ctrl Pts',(-3.68452647523737,-1.76798881677802,
-38.1712730780915));
#26483=CARTESIAN_POINT('Ctrl Pts',(-3.7346770690846,-1.65941580786129,-38.1770879456343));
#26484=CARTESIAN_POINT('Ctrl Pts',(-3.77993924292916,-1.54896233645757,
-38.182902813177));
#26485=CARTESIAN_POINT('Ctrl Pts',(-3.82523109851871,-1.43843643256791,
-38.1887214939572));
#26486=CARTESIAN_POINT('Ctrl Pts',(-3.86562801207002,-1.32602799318487,
-38.1945401747374));
#26487=CARTESIAN_POINT('Ctrl Pts',(-3.90099591993381,-1.21221113369731,
-38.2003588555176));
#26488=CARTESIAN_POINT('Ctrl Pts',(-3.93641378552208,-1.09823350611097,
-38.2061857552756));
#26489=CARTESIAN_POINT('Ctrl Pts',(-3.96678836416692,-0.982843880774551,
-38.2120126550337));
#26490=CARTESIAN_POINT('Ctrl Pts',(-3.99203650673829,-0.866527281087397,
-38.2178395547917));
#26491=CARTESIAN_POINT('Ctrl Pts',(-3.99796952572057,-0.839194237005159,
-38.2192088082635));
#26492=CARTESIAN_POINT('Ctrl Pts',(-4.00361969092606,-0.811810029377355,
-38.2205780617353));
#26493=CARTESIAN_POINT('Ctrl Pts',(-4.00898633942689,-0.784380985420102,
-38.2219473152071));
#26494=CARTESIAN_POINT('Ctrl Pts',(-4.04160802073748,-0.617650943292322,
-38.2302704521488));
#26495=CARTESIAN_POINT('Ctrl Pts',(-4.06383608673867,-0.448826534878653,
-38.2385935890905));
#26496=CARTESIAN_POINT('Ctrl Pts',(-4.07546276612986,-0.278977135065131,
-38.2469167260322));
#26497=CARTESIAN_POINT('Ctrl Pts',(-4.08173407833672,-0.187362102213624,
-38.2514061411563));
#26498=CARTESIAN_POINT('Ctrl Pts',(-4.0849217525647,-0.0954491999141607,
-38.2558955562804));
#26499=CARTESIAN_POINT('Ctrl Pts',(-4.0849985769771,-0.00340970600798366,
-38.2603849714045));
#26500=CARTESIAN_POINT('Origin',(0.,0.,-25.2396150285955));
#26501=CARTESIAN_POINT('',(2.4870572760686,3.24064362520075,-36.2030038303486));
#26502=CARTESIAN_POINT('',(2.4870572760686,3.24064362520075,-36.3074370930634));
#26503=CARTESIAN_POINT('',(2.4870572760686,3.24064362520075,-25.2396150285955));
#26504=CARTESIAN_POINT('',(-4.08499957977947,-0.00185289005459989,-37.1146150285588));
#26505=CARTESIAN_POINT('Ctrl Pts',(2.4870572760686,3.24064362520075,-36.3074370930634));
#26506=CARTESIAN_POINT('Ctrl Pts',(2.58180014386427,3.16793247088731,-36.3132441745903));
#26507=CARTESIAN_POINT('Ctrl Pts',(2.67341078999859,3.09101770294433,-36.3190512561171));
#26508=CARTESIAN_POINT('Ctrl Pts',(2.76150160643884,3.0102049560845,-36.324858337644));
#26509=CARTESIAN_POINT('Ctrl Pts',(2.84956668578501,2.9294158199182,-36.3306637225421));
#26510=CARTESIAN_POINT('Ctrl Pts',(2.93411367992539,2.84473124498611,-36.3364691074403));
#26511=CARTESIAN_POINT('Ctrl Pts',(3.01478912421968,2.7564962427848,-36.3422744923385));
#26512=CARTESIAN_POINT('Ctrl Pts',(3.09546000078508,2.6682662363238,-36.3480795485441));
#26513=CARTESIAN_POINT('Ctrl Pts',(3.1722594882483,2.57648650359193,-36.3538846047496));
#26514=CARTESIAN_POINT('Ctrl Pts',(3.24487241507926,2.48153742866347,-36.3596896609552));
#26515=CARTESIAN_POINT('Ctrl Pts',(3.31749833426117,2.38657136486322,-36.365495755837));
#26516=CARTESIAN_POINT('Ctrl Pts',(3.38593595537108,2.28843515528463,-36.3713018507189));
#26517=CARTESIAN_POINT('Ctrl Pts',(3.44991206848321,2.18754010700007,-36.3771079456008));
#26518=CARTESIAN_POINT('Ctrl Pts',(3.51395407662326,2.08654113739707,-36.3829200207269));
#26519=CARTESIAN_POINT('Ctrl Pts',(3.573525179289,1.9827779985427,-36.3887320958531));
#26520=CARTESIAN_POINT('Ctrl Pts',(3.62839686054799,1.87668889866314,-36.3945441709792));
#26521=CARTESIAN_POINT('Ctrl Pts',(3.68329739593559,1.77054401211074,-36.4003593023697));
#26522=CARTESIAN_POINT('Ctrl Pts',(3.73349341497927,1.66207109787077,-36.4061744337602));
#26523=CARTESIAN_POINT('Ctrl Pts',(3.77880425461889,1.55172916621239,-36.4119895651507));
#26524=CARTESIAN_POINT('Ctrl Pts',(3.82418714418058,1.44121177703344,-36.4178139433299));
#26525=CARTESIAN_POINT('Ctrl Pts',(3.86466919502848,1.32881981642843,-36.4236383215092));
#26526=CARTESIAN_POINT('Ctrl Pts',(3.90011921975187,1.21502883575743,-36.4294626996885));
#26527=CARTESIAN_POINT('Ctrl Pts',(3.93065407232591,1.11701505872468,-36.4344795235251));
#26528=CARTESIAN_POINT('Ctrl Pts',(3.95745634301611,1.01796369683905,-36.4394963473616));
#26529=CARTESIAN_POINT('Ctrl Pts',(3.98047278670977,0.918183747548924,-36.4445131711982));
#26530=CARTESIAN_POINT('Ctrl Pts',(4.00719913262867,0.802320781228317,-36.4503386310762));
#26531=CARTESIAN_POINT('Ctrl Pts',(4.02890525524872,0.685104581897241,-36.4561640909541));
#26532=CARTESIAN_POINT('Ctrl Pts',(4.0454576034012,0.567007741643311,-36.4619895508321));
#26533=CARTESIAN_POINT('Ctrl Pts',(4.06198917531036,0.449059134659096,-36.4678076986857));
#26534=CARTESIAN_POINT('Ctrl Pts',(4.07337978343739,0.330232485900519,-36.4736258465394));
#26535=CARTESIAN_POINT('Ctrl Pts',(4.07954637044436,0.211012822819462,-36.479443994393));
#26536=CARTESIAN_POINT('Ctrl Pts',(4.08570682135357,0.0919117899477465,
-36.4852563528653));
#26537=CARTESIAN_POINT('Ctrl Pts',(4.08665357156166,-0.0275810740777785,
-36.4910687113376));
#26538=CARTESIAN_POINT('Ctrl Pts',(4.08235516152713,-0.146973926778875,
-36.4968810698099));
#26539=CARTESIAN_POINT('Ctrl Pts',(4.07791157546125,-0.270399196207944,
-36.5028897369472));
#26540=CARTESIAN_POINT('Ctrl Pts',(4.06786219252625,-0.393717139271351,
-36.5088984040845));
#26541=CARTESIAN_POINT('Ctrl Pts',(4.05223082381314,-0.516381981229635,
-36.5149070712219));
#26542=CARTESIAN_POINT('Ctrl Pts',(4.0371269886833,-0.634907081825153,-36.5207129554959));
#26543=CARTESIAN_POINT('Ctrl Pts',(4.01681191031066,-0.752822015257029,
-36.5265188397699));
#26544=CARTESIAN_POINT('Ctrl Pts',(3.99135989129911,-0.86963855602702,-36.5323247240439));
#26545=CARTESIAN_POINT('Ctrl Pts',(3.96591156081907,-0.986438167629546,
-36.5381297669235));
#26546=CARTESIAN_POINT('Ctrl Pts',(3.93532785707022,-1.1021393045834,-36.543934809803));
#26547=CARTESIAN_POINT('Ctrl Pts',(3.89973416268372,-1.21626414088285,-36.5497398526826));
#26548=CARTESIAN_POINT('Ctrl Pts',(3.86413724282331,-1.33039931908943,-36.5555454216108));
#26549=CARTESIAN_POINT('Ctrl Pts',(3.82352955114842,-1.44295752310767,-36.561350990539));
#26550=CARTESIAN_POINT('Ctrl Pts',(3.77808609014614,-1.55347690534629,-36.5671565594672));
#26551=CARTESIAN_POINT('Ctrl Pts',(3.7326278074101,-1.66403233433007,-36.5729640219263));
#26552=CARTESIAN_POINT('Ctrl Pts',(3.68233077364905,-1.77254724186748,-36.5787714843854));
#26553=CARTESIAN_POINT('Ctrl Pts',(3.62741752731441,-1.87858113546693,-36.5845789468445));
#26554=CARTESIAN_POINT('Ctrl Pts',(3.57244375577298,-1.98473189928922,-36.5903928102703));
#26555=CARTESIAN_POINT('Ctrl Pts',(3.5128438035658,-2.08839582834566,-36.5962066736962));
#26556=CARTESIAN_POINT('Ctrl Pts',(3.44888551003451,-2.18915822604808,-36.6020205371221));
#26557=CARTESIAN_POINT('Ctrl Pts',(3.38488513850607,-2.28998691507333,-36.6078382254738));
#26558=CARTESIAN_POINT('Ctrl Pts',(3.31652094819986,-2.38790993727525,-36.6136559138255));
#26559=CARTESIAN_POINT('Ctrl Pts',(3.24410234899087,-2.48254404780095,-36.6194736021772));
#26560=CARTESIAN_POINT('Ctrl Pts',(3.17158113638138,-2.5773122499549,-36.6252995338917));
#26561=CARTESIAN_POINT('Ctrl Pts',(3.0949943098072,-2.6687819275656,-36.6311254656062));
#26562=CARTESIAN_POINT('Ctrl Pts',(3.0146895983794,-2.75660509058208,-36.6369513973206));
#26563=CARTESIAN_POINT('Ctrl Pts',(2.9956783043551,-2.77739629877603,-36.6383306252491));
#26564=CARTESIAN_POINT('Ctrl Pts',(2.97645879095806,-2.79798330888898,-36.6397098531776));
#26565=CARTESIAN_POINT('Ctrl Pts',(2.95703594603752,-2.81836183160395,-36.6410890811061));
#26566=CARTESIAN_POINT('Ctrl Pts',(2.87499899282679,-2.90443531472711,-36.6469145746163));
#26567=CARTESIAN_POINT('Ctrl Pts',(2.78906955788716,-2.98706160281669,-36.6527400681266));
#26568=CARTESIAN_POINT('Ctrl Pts',(2.6995687634409,-3.06586912497161,-36.6585655616368));
#26569=CARTESIAN_POINT('Ctrl Pts',(2.6101803029062,-3.14457773451599,-36.6643837434749));
#26570=CARTESIAN_POINT('Ctrl Pts',(2.5172297021419,-3.21947684419097,-36.6702019253129));
#26571=CARTESIAN_POINT('Ctrl Pts',(2.4210762519493,-3.29023020201431,-36.6760201071509));
#26572=CARTESIAN_POINT('Ctrl Pts',(2.32501847416656,-3.36091316044756,-36.6818324999145));
#26573=CARTESIAN_POINT('Ctrl Pts',(2.22576451365462,-3.4274583329537,-36.6876448926782));
#26574=CARTESIAN_POINT('Ctrl Pts',(2.12370774441464,-3.48956880091413,-36.6934572854418));
#26575=CARTESIAN_POINT('Ctrl Pts',(2.01820491961201,-3.55377649500867,-36.6994659398406));
#26576=CARTESIAN_POINT('Ctrl Pts',(1.90970699030915,-3.61324440640284,-36.7054745942395));
#26577=CARTESIAN_POINT('Ctrl Pts',(1.79868276597447,-3.66769209549908,-36.7114832486383));
#26578=CARTESIAN_POINT('Ctrl Pts',(1.69140455987633,-3.72030268969541,-36.7172891677414));
#26579=CARTESIAN_POINT('Ctrl Pts',(1.58176818138103,-3.76822617288067,-36.7230950868445));
#26580=CARTESIAN_POINT('Ctrl Pts',(1.47022218216631,-3.81125592620938,-36.7289010059476));
#26581=CARTESIAN_POINT('Ctrl Pts',(1.35869234558041,-3.85427944467592,-36.7347060837931));
#26582=CARTESIAN_POINT('Ctrl Pts',(1.24525381912777,-3.8924104966771,-36.7405111616386));
#26583=CARTESIAN_POINT('Ctrl Pts',(1.13037457912866,-3.92549083693488,-36.7463162394842));
#26584=CARTESIAN_POINT('Ctrl Pts',(1.01548492698741,-3.95857417544722,-36.7521218434761));
#26585=CARTESIAN_POINT('Ctrl Pts',(0.899154693770183,-3.98660577914462,
-36.757927447468));
#26586=CARTESIAN_POINT('Ctrl Pts',(0.781865818708626,-4.00947762701516,
-36.7637330514599));
#26587=CARTESIAN_POINT('Ctrl Pts',(0.664538688028052,-4.03235693490011,
-36.7695405490412));
#26588=CARTESIAN_POINT('Ctrl Pts',(0.546252693907931,-4.05007306188573,
-36.7753480466226));
#26589=CARTESIAN_POINT('Ctrl Pts',(0.427498102411096,-4.06256942986024,
-36.7811555442039));
#26590=CARTESIAN_POINT('Ctrl Pts',(0.308612622638982,-4.0750795710121,-36.7869694426606));
#26591=CARTESIAN_POINT('Ctrl Pts',(0.189257920571902,-4.0823584270099,-36.7927833411173));
#26592=CARTESIAN_POINT('Ctrl Pts',(0.0699276512532866,-4.08440144006318,
-36.7985972395741));
#26593=CARTESIAN_POINT('Ctrl Pts',(-0.0494811243941398,-4.08644579719668,
-36.8044149629432));
#26594=CARTESIAN_POINT('Ctrl Pts',(-0.168865028371516,-4.08324746214124,
-36.8102326863123));
#26595=CARTESIAN_POINT('Ctrl Pts',(-0.287733791801261,-4.07485389493362,
-36.8160504096814));
#26596=CARTESIAN_POINT('Ctrl Pts',(-0.406770979274152,-4.06644843495884,
-36.8218763761285));
#26597=CARTESIAN_POINT('Ctrl Pts',(-0.525291165562446,-4.05283309748878,
-36.8277023425756));
#26598=CARTESIAN_POINT('Ctrl Pts',(-0.642812432542545,-4.0341067383708,
-36.8335283090228));
#26599=CARTESIAN_POINT('Ctrl Pts',(-0.670627451910066,-4.02967457000729,
-36.8349072030198));
#26600=CARTESIAN_POINT('Ctrl Pts',(-0.698386574971191,-4.02495631525664,
-36.8362860970168));
#26601=CARTESIAN_POINT('Ctrl Pts',(-0.726083535138221,-4.0199536937633,
-36.8376649910139));
#26602=CARTESIAN_POINT('Ctrl Pts',(-0.843093124115286,-3.99881943638582,
-36.8434903169291));
#26603=CARTESIAN_POINT('Ctrl Pts',(-0.959366434350854,-3.97253839256482,
-36.8493156428444));
#26604=CARTESIAN_POINT('Ctrl Pts',(-1.07441652610453,-3.94117420681115,
-36.8551409687596));
#26605=CARTESIAN_POINT('Ctrl Pts',(-1.18932220553573,-3.90984938977799,
-36.8609589826525));
#26606=CARTESIAN_POINT('Ctrl Pts',(-1.30300733016968,-3.87345422796144,
-36.8667769965454));
#26607=CARTESIAN_POINT('Ctrl Pts',(-1.41499344566709,-3.83210367144721,
-36.8725950104383));
#26608=CARTESIAN_POINT('Ctrl Pts',(-1.52686812925343,-3.79079426085108,
-36.8784072351098));
#26609=CARTESIAN_POINT('Ctrl Pts',(-1.63704678640305,-3.74453940564873,
-36.8842194597814));
#26610=CARTESIAN_POINT('Ctrl Pts',(-1.74506504863759,-3.69350415947017,
-36.890031684453));
#26611=CARTESIAN_POINT('Ctrl Pts',(-1.85673506199582,-3.64074357524484,
-36.8960404018058));
#26612=CARTESIAN_POINT('Ctrl Pts',(-1.9660955919792,-3.58287377121514,-36.9020491191587));
#26613=CARTESIAN_POINT('Ctrl Pts',(-2.07265446226879,-3.52013188389828,
-36.9080578365116));
#26614=CARTESIAN_POINT('Ctrl Pts',(-2.17561393055959,-3.45950932530555,
-36.9138635882249));
#26615=CARTESIAN_POINT('Ctrl Pts',(-2.27595757457715,-3.39433873481196,
-36.9196693399383));
#26616=CARTESIAN_POINT('Ctrl Pts',(-2.37326606047514,-3.32488093113074,
-36.9254750916517));
#26617=CARTESIAN_POINT('Ctrl Pts',(-2.47056045552059,-3.25543318535619,
-36.9312800026574));
#26618=CARTESIAN_POINT('Ctrl Pts',(-2.56482023449916,-3.18169969803635,
-36.9370849136632));
#26619=CARTESIAN_POINT('Ctrl Pts',(-2.65565576540302,-3.1039841261968,-36.9428898246689));
#26620=CARTESIAN_POINT('Ctrl Pts',(-2.74649954090315,-3.02626150058096,
-36.9486952625515));
#26621=CARTESIAN_POINT('Ctrl Pts',(-2.83391814032715,-2.94455633711105,
-36.9545007004342));
#26622=CARTESIAN_POINT('Ctrl Pts',(-2.91755618456264,-2.85921158886856,
-36.9603061383169));
#26623=CARTESIAN_POINT('Ctrl Pts',(-3.00122152258653,-2.77383898988517,
-36.9661134707009));
#26624=CARTESIAN_POINT('Ctrl Pts',(-3.0811035663642,-2.68482473527792,-36.971920803085));
#26625=CARTESIAN_POINT('Ctrl Pts',(-3.15688530885822,-2.59254703847686,
-36.9777281354691));
#26626=CARTESIAN_POINT('Ctrl Pts',(-3.23275060673821,-2.50016759819091,
-36.9835418708981));
#26627=CARTESIAN_POINT('Ctrl Pts',(-3.3045063202977,-2.40451784903669,-36.989355606327));
#26628=CARTESIAN_POINT('Ctrl Pts',(-3.3718770139343,-2.30600745942018,-36.995169341756));
#26629=CARTESIAN_POINT('Ctrl Pts',(-3.43929204391157,-2.20743224057366,
-37.0009869031773));
#26630=CARTESIAN_POINT('Ctrl Pts',(-3.50231609198979,-2.10599297779654,
-37.0068044645985));
#26631=CARTESIAN_POINT('Ctrl Pts',(-3.56071902041228,-2.00212513536847,
-37.0126220260198));
#26632=CARTESIAN_POINT('Ctrl Pts',(-3.61920472967253,-1.89811006972326,
-37.0184478333051));
#26633=CARTESIAN_POINT('Ctrl Pts',(-3.67305606280072,-1.79165991683374,
-37.0242736405904));
#26634=CARTESIAN_POINT('Ctrl Pts',(-3.72209039230199,-1.68323144918732,
-37.0300994478757));
#26635=CARTESIAN_POINT('Ctrl Pts',(-3.73370957589475,-1.65753821987064,
-37.0314799322244));
#26636=CARTESIAN_POINT('Ctrl Pts',(-3.74505850319891,-1.63173397917305,
-37.032860416573));
#26637=CARTESIAN_POINT('Ctrl Pts',(-3.75613515493064,-1.60582492753544,
-37.0342409009217));
#26638=CARTESIAN_POINT('Ctrl Pts',(-3.80987693409516,-1.48011920299036,
-37.0409387448915));
#26639=CARTESIAN_POINT('Ctrl Pts',(-3.8573578000689,-1.35158683004276,-37.0476365888612));
#26640=CARTESIAN_POINT('Ctrl Pts',(-3.89830388899858,-1.22084060753995,
-37.054334432831));
#26641=CARTESIAN_POINT('Ctrl Pts',(-3.93744257703139,-1.09586565272087,
-37.0607366273379));
#26642=CARTESIAN_POINT('Ctrl Pts',(-3.97061085531542,-0.968868392783439,
-37.0671388218447));
#26643=CARTESIAN_POINT('Ctrl Pts',(-3.99761682229106,-0.8404074857684,-37.0735410163516));
#26644=CARTESIAN_POINT('Ctrl Pts',(-4.02455076465145,-0.712289182571588,
-37.0799261362766));
#26645=CARTESIAN_POINT('Ctrl Pts',(-4.04535509838463,-0.582715268947795,
-37.0863112562016));
#26646=CARTESIAN_POINT('Ctrl Pts',(-4.05988750416817,-0.452259276852506,
-37.0926963761265));
#26647=CARTESIAN_POINT('Ctrl Pts',(-4.07436256324668,-0.322318080545952,
-37.0990562995634));
#26648=CARTESIAN_POINT('Ctrl Pts',(-4.08261499785419,-0.191502005844116,
-37.1054162230003));
#26649=CARTESIAN_POINT('Ctrl Pts',(-4.08455354278761,-0.0603933448418993,
-37.1117761464372));
#26650=CARTESIAN_POINT('Ctrl Pts',(-4.08484197920292,-0.0408856658898553,
-37.1127224404777));
#26651=CARTESIAN_POINT('Ctrl Pts',(-4.08499072643696,-0.0213715335651584,
-37.1136687345182));
#26652=CARTESIAN_POINT('Ctrl Pts',(-4.08499957977947,-0.00185289005462216,
-37.1146150285587));
#26653=CARTESIAN_POINT('Ctrl Pts',(-4.08499957977981,-0.00185288929646346,
-37.1146150285955));
#26654=CARTESIAN_POINT('Ctrl Pts',(-4.08505473546161,0.119746894016321,
-37.1205103742538));
#26655=CARTESIAN_POINT('Ctrl Pts',(-4.07967598016496,0.241334433021924,
-37.1264057199121));
#26656=CARTESIAN_POINT('Ctrl Pts',(-4.06889302361888,0.362401106987252,
-37.1323010655705));
#26657=CARTESIAN_POINT('Ctrl Pts',(-4.0581063695184,0.483509295597695,-37.1381984327858));
#26658=CARTESIAN_POINT('Ctrl Pts',(-4.04191185845429,0.604095875033717,
-37.1440958000011));
#26659=CARTESIAN_POINT('Ctrl Pts',(-4.02039100139374,0.723658203789787,
-37.1499931672164));
#26660=CARTESIAN_POINT('Ctrl Pts',(-3.9988583612579,0.84328599517664,-37.1558937633516));
#26661=CARTESIAN_POINT('Ctrl Pts',(-3.97199363687583,0.961888035660562,
-37.1617943594867));
#26662=CARTESIAN_POINT('Ctrl Pts',(-3.93992918942795,1.07897311472235,-37.1676949556219));
#26663=CARTESIAN_POINT('Ctrl Pts',(-3.90781874707215,1.1962261466995,-37.1736040158784));
#26664=CARTESIAN_POINT('Ctrl Pts',(-3.87049378751551,1.31195749460793,-37.1795130761349));
#26665=CARTESIAN_POINT('Ctrl Pts',(-3.82813637309824,1.42569172999012,-37.1854221363915));
#26666=CARTESIAN_POINT('Ctrl Pts',(-3.78574545813174,1.5395159179675,-37.1913358701336));
#26667=CARTESIAN_POINT('Ctrl Pts',(-3.73831430745432,1.65133948690727,-37.1972496038757));
#26668=CARTESIAN_POINT('Ctrl Pts',(-3.68607220043215,1.76070915633483,-37.2031633376178));
#26669=CARTESIAN_POINT('Ctrl Pts',(-3.63373917189645,1.87026917137525,-37.2090873635485));
#26670=CARTESIAN_POINT('Ctrl Pts',(-3.57657864329999,1.97736641136903,-37.2150113894793));
#26671=CARTESIAN_POINT('Ctrl Pts',(-3.51486503032096,2.08157363997213,-37.2209354154101));
#26672=CARTESIAN_POINT('Ctrl Pts',(-3.48055184422449,2.13951356367859,-37.2242292138832));
#26673=CARTESIAN_POINT('Ctrl Pts',(-3.44483186559839,2.19656059362429,-37.2275230123564));
#26674=CARTESIAN_POINT('Ctrl Pts',(-3.40775771819042,2.25264562994574,-37.2308168108295));
#26675=CARTESIAN_POINT('Ctrl Pts',(-3.34218511804745,2.35184256144197,-37.2366425127089));
#26676=CARTESIAN_POINT('Ctrl Pts',(-3.27217279490521,2.44833254806676,-37.2424682145883));
#26677=CARTESIAN_POINT('Ctrl Pts',(-3.19797134279151,2.54169319365739,-37.2482939164677));
#26678=CARTESIAN_POINT('Ctrl Pts',(-3.12386299720566,2.63493669213967,-37.2541123083705));
#26679=CARTESIAN_POINT('Ctrl Pts',(-3.04557622945642,2.72505834313826,-37.2599307002734));
#26680=CARTESIAN_POINT('Ctrl Pts',(-2.96340543128871,2.81166378676551,-37.2657490921762));
#26681=CARTESIAN_POINT('Ctrl Pts',(-2.8813163697767,2.89818308252169,-37.2715616964281));
#26682=CARTESIAN_POINT('Ctrl Pts',(-2.79535124321465,2.98119283488133,-37.2773743006801));
#26683=CARTESIAN_POINT('Ctrl Pts',(-2.70584492772651,3.06033139171181,-37.283186904932));
#26684=CARTESIAN_POINT('Ctrl Pts',(-2.61332091521497,3.14213809755591,-37.2891954805905));
#26685=CARTESIAN_POINT('Ctrl Pts',(-2.51701298912991,3.21980761384266,-37.2952040562491));
#26686=CARTESIAN_POINT('Ctrl Pts',(-2.41733312448836,3.29298125795628,-37.3012126319077));
#26687=CARTESIAN_POINT('Ctrl Pts',(-2.32101170661539,3.3636895115971,-37.3070187646598));
#26688=CARTESIAN_POINT('Ctrl Pts',(-2.22154226226428,3.43019970545135,-37.312824897412));
#26689=CARTESIAN_POINT('Ctrl Pts',(-2.11932990166901,3.49222934067791,-37.3186310301642));
#26690=CARTESIAN_POINT('Ctrl Pts',(-2.01713234332954,3.5542499928566,-37.3244363220801));
#26691=CARTESIAN_POINT('Ctrl Pts',(-1.91219300741612,3.61179116524839,-37.330241613996));
#26692=CARTESIAN_POINT('Ctrl Pts',(-1.80494465494147,3.66461454898032,-37.3360469059119));
#26693=CARTESIAN_POINT('Ctrl Pts',(-1.69768657892346,3.71744272188103,-37.3418527241577));
#26694=CARTESIAN_POINT('Ctrl Pts',(-1.58811943612311,3.76555207541462,-37.3476585424034));
#26695=CARTESIAN_POINT('Ctrl Pts',(-1.47669858897939,3.80875127532716,-37.3534643606491));
#26696=CARTESIAN_POINT('Ctrl Pts',(-1.36524140254996,3.85196456441699,-37.35927207243));
#26697=CARTESIAN_POINT('Ctrl Pts',(-1.25192968958113,3.89026436757713,-37.3650797842109));
#26698=CARTESIAN_POINT('Ctrl Pts',(-1.13723608154764,3.92350851851072,-37.3708874959917));
#26699=CARTESIAN_POINT('Ctrl Pts',(-1.02241608874378,3.95678930229991,-37.3767016074869));
#26700=CARTESIAN_POINT('Ctrl Pts',(-0.906211553442713,3.98500320025736,
-37.382515718982));
#26701=CARTESIAN_POINT('Ctrl Pts',(-0.789107617796565,4.00805865320549,
-37.3883298304771));
#26702=CARTESIAN_POINT('Ctrl Pts',(-0.671926652090707,4.03112927185158,
-37.3941477664497));
#26703=CARTESIAN_POINT('Ctrl Pts',(-0.553845510216698,4.04903462673042,
-37.3999657024222));
#26704=CARTESIAN_POINT('Ctrl Pts',(-0.435355176305768,4.06173495817536,
-37.4057836383947));
#26705=CARTESIAN_POINT('Ctrl Pts',(-0.316697006269296,4.07445327905751,
-37.4116098152069));
#26706=CARTESIAN_POINT('Ctrl Pts',(-0.197628893062967,4.08195183605581,
-37.4174359920189));
#26707=CARTESIAN_POINT('Ctrl Pts',(-0.0786426664223028,4.08424293241942,
-37.4232621688311));
#26708=CARTESIAN_POINT('Ctrl Pts',(-0.0505236671123266,4.0847843676669,
-37.4246390194665));
#26709=CARTESIAN_POINT('Ctrl Pts',(-0.0224092201751181,4.08503520577175,
-37.4260158701019));
#26710=CARTESIAN_POINT('Ctrl Pts',(0.00569423172731292,4.08499603129857,
-37.4273927207374));
#26711=CARTESIAN_POINT('Ctrl Pts',(0.12455891370801,4.08483034128609,-37.433216165967));
#26712=CARTESIAN_POINT('Ctrl Pts',(0.24360683494036,4.07947201898683,-37.4390396111966));
#26713=CARTESIAN_POINT('Ctrl Pts',(0.362347851072246,4.06889776657307,-37.4448630564262));
#26714=CARTESIAN_POINT('Ctrl Pts',(0.480949503326026,4.05833592494097,-37.4506796667985));
#26715=CARTESIAN_POINT('Ctrl Pts',(0.59924456398741,4.0425703610407,-37.4564962771707));
#26716=CARTESIAN_POINT('Ctrl Pts',(0.716742062204008,4.02162974629286,-37.462312887543));
#26717=CARTESIAN_POINT('Ctrl Pts',(0.834129368664295,4.00070877011734,-37.4681240429691));
#26718=CARTESIAN_POINT('Ctrl Pts',(0.950720200828518,3.97462246633722,-37.4739351983953));
#26719=CARTESIAN_POINT('Ctrl Pts',(1.06602852163193,3.94345130451325,-37.4797463538215));
#26720=CARTESIAN_POINT('Ctrl Pts',(1.18125589513586,3.9123020250769,-37.4855534297733));
#26721=CARTESIAN_POINT('Ctrl Pts',(1.2952021557613,3.87607509511182,-37.4913605057252));
#26722=CARTESIAN_POINT('Ctrl Pts',(1.40739190563755,3.83490195754023,-37.497167581677));
#26723=CARTESIAN_POINT('Ctrl Pts',(1.51953878294409,3.79374455401042,-37.5029724384932));
#26724=CARTESIAN_POINT('Ctrl Pts',(1.6299301014438,3.74764484111999,-37.5087772953095));
#26725=CARTESIAN_POINT('Ctrl Pts',(1.73810656286463,3.69678381517325,-37.5145821521257));
#26726=CARTESIAN_POINT('Ctrl Pts',(1.84625869051855,3.64593423016601,-37.5203857031677));
#26727=CARTESIAN_POINT('Ctrl Pts',(1.95219658478059,3.59032563997139,-37.5261892542097));
#26728=CARTESIAN_POINT('Ctrl Pts',(2.05548253496176,3.53018647502751,-37.5319928052517));
#26729=CARTESIAN_POINT('Ctrl Pts',(2.15879230275974,3.47003344206399,-37.5377976945857));
#26730=CARTESIAN_POINT('Ctrl Pts',(2.25944855246946,3.40534795340386,-37.5436025839197));
#26731=CARTESIAN_POINT('Ctrl Pts',(2.3570399952545,3.33640337201164,-37.5494074732536));
#26732=CARTESIAN_POINT('Ctrl Pts',(2.40101277785794,3.30533830111272,-37.5520230420928));
#26733=CARTESIAN_POINT('Ctrl Pts',(2.44436372773356,3.27340912252422,-37.554638610932));
#26734=CARTESIAN_POINT('Ctrl Pts',(2.4870572760686,3.24064362520074,-37.5572541797712));
#26735=CARTESIAN_POINT('',(-4.08499880087778,0.00312998835824307,-37.0103849713737));
#26736=CARTESIAN_POINT('Ctrl Pts',(-4.08499880087729,0.00312998898833224,
-37.0103849714045));
#26737=CARTESIAN_POINT('Ctrl Pts',(-4.08485458355566,0.191350327181431,
-37.0195759887022));
#26738=CARTESIAN_POINT('Ctrl Pts',(-4.07169872079374,0.379076168690209,
-37.0287670059998));
#26739=CARTESIAN_POINT('Ctrl Pts',(-4.04575227482873,0.564901346004933,
-37.0379580232975));
#26740=CARTESIAN_POINT('Ctrl Pts',(-4.04148590491574,0.5954565498521,-37.039469300785));
#26741=CARTESIAN_POINT('Ctrl Pts',(-4.0368738005675,0.625960438495345,-37.0409805782726));
#26742=CARTESIAN_POINT('Ctrl Pts',(-4.03191704667525,0.656406831720633,
-37.0424918557601));
#26743=CARTESIAN_POINT('Ctrl Pts',(-4.01281033940161,0.773767978862407,
-37.048317349055));
#26744=CARTESIAN_POINT('Ctrl Pts',(-3.98854459284321,0.890481918751973,
-37.0541428423498));
#26745=CARTESIAN_POINT('Ctrl Pts',(-3.95917503351028,1.00606066120731,-37.0599683356447));
#26746=CARTESIAN_POINT('Ctrl Pts',(-3.92984233639821,1.12149433886671,-37.0657865172663));
#26747=CARTESIAN_POINT('Ctrl Pts',(-3.89541866753644,1.23579526104816,-37.071604698888));
#26748=CARTESIAN_POINT('Ctrl Pts',(-3.85601069792159,1.34848303567908,-37.0774228805096));
#26749=CARTESIAN_POINT('Ctrl Pts',(-3.81664193913112,1.4610586862756,-37.0832352730561));
#26750=CARTESIAN_POINT('Ctrl Pts',(-3.77229887976568,1.57202399953313,-37.0890476656026));
#26751=CARTESIAN_POINT('Ctrl Pts',(-3.72313853025277,1.68091180153725,-37.0948600581491));
#26752=CARTESIAN_POINT('Ctrl Pts',(-3.67231822656987,1.79347632192906,-37.100868712629));
#26753=CARTESIAN_POINT('Ctrl Pts',(-3.61634966291073,1.90382011894975,-37.106877367109));
#26754=CARTESIAN_POINT('Ctrl Pts',(-3.5554614139301,2.01144702491868,-37.1128860215889));
#26755=CARTESIAN_POINT('Ctrl Pts',(-3.496627570872,2.11544253473566,-37.1186919404745));
#26756=CARTESIAN_POINT('Ctrl Pts',(-3.43320089022276,2.21690115161157,-37.12449785936));
#26757=CARTESIAN_POINT('Ctrl Pts',(-3.36543490981202,2.31539907312293,-37.1303037782455));
#26758=CARTESIAN_POINT('Ctrl Pts',(-3.29767874845482,2.41388272262999,-37.1361088558737));
#26759=CARTESIAN_POINT('Ctrl Pts',(-3.22558476896845,2.50940619388783,-37.1419139335019));
#26760=CARTESIAN_POINT('Ctrl Pts',(-3.14944985494286,2.60157464071289,-37.1477190111301));
#26761=CARTESIAN_POINT('Ctrl Pts',(-3.07330804038194,2.69375144128252,-37.1535246149052));
#26762=CARTESIAN_POINT('Ctrl Pts',(-2.99312482293973,2.78257229824525,-37.1593302186802));
#26763=CARTESIAN_POINT('Ctrl Pts',(-2.90923696921039,2.86767593304745,-37.1651358224552));
#26764=CARTESIAN_POINT('Ctrl Pts',(-2.82532175412129,2.95280732575577,-37.1709433198204));
#26765=CARTESIAN_POINT('Ctrl Pts',(-2.73769978589935,3.03421879460071,-37.1767508171856));
#26766=CARTESIAN_POINT('Ctrl Pts',(-2.64674375059762,3.11158681683035,-37.1825583145507));
#26767=CARTESIAN_POINT('Ctrl Pts',(-2.55568746584244,3.18904011214734,-37.1883722127934));
#26768=CARTESIAN_POINT('Ctrl Pts',(-2.46129009004387,3.26244080079951,-37.194186111036));
#26769=CARTESIAN_POINT('Ctrl Pts',(-2.36395647938206,3.33150638054133,-37.2000000092786));
#26770=CARTESIAN_POINT('Ctrl Pts',(-2.2665588337801,3.40061739793037,-37.2058177324346));
#26771=CARTESIAN_POINT('Ctrl Pts',(-2.16622144816884,3.46538740566566,-37.2116354555906));
#26772=CARTESIAN_POINT('Ctrl Pts',(-2.06337575569537,3.52557874551237,-37.2174531787466));
#26773=CARTESIAN_POINT('Ctrl Pts',(-1.96038434205945,3.58585536994223,-37.2232791449836));
#26774=CARTESIAN_POINT('Ctrl Pts',(-1.85487788776261,3.64154018859385,-37.2291051112207));
#26775=CARTESIAN_POINT('Ctrl Pts',(-1.74730995426144,3.69244267710941,-37.2349310774577));
#26776=CARTESIAN_POINT('Ctrl Pts',(-1.72185065794288,3.70449033384398,-37.2363099735278));
#26777=CARTESIAN_POINT('Ctrl Pts',(-1.69627595666987,3.71627031161957,-37.2376888695979));
#26778=CARTESIAN_POINT('Ctrl Pts',(-1.67059199348252,3.72778049129936,-37.239067765668));
#26779=CARTESIAN_POINT('Ctrl Pts',(-1.56208673973579,3.77640674721308,-37.2448930920354));
#26780=CARTESIAN_POINT('Ctrl Pts',(-1.45128304613134,3.82036945305346,-37.2507184184027));
#26781=CARTESIAN_POINT('Ctrl Pts',(-1.33861873677264,3.85944618793438,-37.2565437447701));
#26782=CARTESIAN_POINT('Ctrl Pts',(-1.22609584505556,3.89847387321193,-37.2623617591154));
#26783=CARTESIAN_POINT('Ctrl Pts',(-1.11171736502236,3.9326276534788,-37.2681797734607));
#26784=CARTESIAN_POINT('Ctrl Pts',(-0.995943087002967,3.96173224328084,
-37.273997787806));
#26785=CARTESIAN_POINT('Ctrl Pts',(-0.880284010305376,3.990807872529,-37.2798100129298));
#26786=CARTESIAN_POINT('Ctrl Pts',(-0.763232292185154,4.01484420762205,
-37.2856222380536));
#26787=CARTESIAN_POINT('Ctrl Pts',(-0.645264388233329,4.03371526874145,
-37.2914344631774));
#26788=CARTESIAN_POINT('Ctrl Pts',(-0.523308380602152,4.05322429786537,
-37.2974431803606));
#26789=CARTESIAN_POINT('Ctrl Pts',(-0.400373562924836,4.06721247861894,
-37.3034518975439));
#26790=CARTESIAN_POINT('Ctrl Pts',(-0.277000042696729,4.07559762198699,
-37.3094606147272));
#26791=CARTESIAN_POINT('Ctrl Pts',(-0.157793886046388,4.08369952839299,
-37.3152663668893));
#26792=CARTESIAN_POINT('Ctrl Pts',(-0.0381786251328157,4.08657077786004,
-37.3210721190515));
#26793=CARTESIAN_POINT('Ctrl Pts',(0.0813523796059202,4.08418985728289,
-37.3268778712136));
#26794=CARTESIAN_POINT('Ctrl Pts',(0.200866075497529,4.08180928147814,-37.3326827826661));
#26795=CARTESIAN_POINT('Ctrl Pts',(0.320295131630733,4.07417805629591,-37.3384876941185));
#26796=CARTESIAN_POINT('Ctrl Pts',(0.439146512970421,4.06132679553689,-37.3442926055709));
#26797=CARTESIAN_POINT('Ctrl Pts',(0.558008681684835,4.04847436835166,-37.3500980438978));
#26798=CARTESIAN_POINT('Ctrl Pts',(0.676292665669839,4.03040100744962,-37.3559034822247));
#26799=CARTESIAN_POINT('Ctrl Pts',(0.79351151155194,4.00718909973495,-37.3617089205516));
#26800=CARTESIAN_POINT('Ctrl Pts',(0.910768609656701,3.98396961723948,-37.3675162533769));
#26801=CARTESIAN_POINT('Ctrl Pts',(1.02695947832406,3.95560833219552,-37.3733235862022));
#26802=CARTESIAN_POINT('Ctrl Pts',(1.14160892428342,3.92223839968919,-37.3791309190275));
#26803=CARTESIAN_POINT('Ctrl Pts',(1.25638478021734,3.88883167422426,-37.3849446548911));
#26804=CARTESIAN_POINT('Ctrl Pts',(1.36961542909423,3.85040539238144,-37.3907583907547));
#26805=CARTESIAN_POINT('Ctrl Pts',(1.48084222697353,3.80714214323711,-37.3965721266184));
#26806=CARTESIAN_POINT('Ctrl Pts',(1.59214222262247,3.76385042277648,-37.4023896884709));
#26807=CARTESIAN_POINT('Ctrl Pts',(1.70143536841723,3.7157155596164,-37.4082072503235));
#26808=CARTESIAN_POINT('Ctrl Pts',(1.80828584066702,3.66296701028595,-37.414024812176));
#26809=CARTESIAN_POINT('Ctrl Pts',(1.91528776358037,3.61014369476467,-37.4198506198845));
#26810=CARTESIAN_POINT('Ctrl Pts',(2.01983974643858,3.55269383693167,-37.4256764275931));
#26811=CARTESIAN_POINT('Ctrl Pts',(2.12153314572536,3.49089130618366,-37.4315022353016));
#26812=CARTESIAN_POINT('Ctrl Pts',(2.14563035596093,3.4762466135392,-37.432882715393));
#26813=CARTESIAN_POINT('Ctrl Pts',(2.16956719796205,3.46135770180052,-37.4342631954844));
#26814=CARTESIAN_POINT('Ctrl Pts',(2.19333850413813,3.44622854817627,-37.4356436755758));
#26815=CARTESIAN_POINT('Ctrl Pts',(2.29403836309909,3.38213852195406,-37.441491656729));
#26816=CARTESIAN_POINT('Ctrl Pts',(2.392088474289,3.31352817431584,-37.4473396378822));
#26817=CARTESIAN_POINT('Ctrl Pts',(2.48705727606859,3.24064362520075,-37.4531876190354));
#26818=CARTESIAN_POINT('Ctrl Pts',(2.4870572760686,3.24064362520075,-36.2030038303486));
#26819=CARTESIAN_POINT('Ctrl Pts',(2.58187463704937,3.16787530051023,-36.2088183190398));
#26820=CARTESIAN_POINT('Ctrl Pts',(2.67342647523315,3.09099531024705,-36.2146328077311));
#26821=CARTESIAN_POINT('Ctrl Pts',(2.76135293747853,3.01034133524401,-36.2204472964224));
#26822=CARTESIAN_POINT('Ctrl Pts',(2.85143172726396,2.92771305390383,-36.2264041163735));
#26823=CARTESIAN_POINT('Ctrl Pts',(2.93770502899664,2.84112395663559,-36.2323609363245));
#26824=CARTESIAN_POINT('Ctrl Pts',(3.01982847136758,2.75097455522906,-36.2383177562756));
#26825=CARTESIAN_POINT('Ctrl Pts',(3.10195191373852,2.66082515382254,-36.2442745762267));
#26826=CARTESIAN_POINT('Ctrl Pts',(3.17992525499167,2.56711583740487,-36.2502313961777));
#26827=CARTESIAN_POINT('Ctrl Pts',(3.25345117218819,2.47027943160026,-36.2561882161288));
#26828=CARTESIAN_POINT('Ctrl Pts',(3.32535558943459,2.37557860238101,-36.2620136676642));
#26829=CARTESIAN_POINT('Ctrl Pts',(3.39323680231942,2.27758420590494,-36.2678391191996));
#26830=CARTESIAN_POINT('Ctrl Pts',(3.45677914334209,2.17667244990034,-36.273664570735));
#26831=CARTESIAN_POINT('Ctrl Pts',(3.52024172793067,2.07588735529484,-36.2794827103389));
#26832=CARTESIAN_POINT('Ctrl Pts',(3.57937605736851,1.97219252677822,-36.2853008499429));
#26833=CARTESIAN_POINT('Ctrl Pts',(3.63390741223458,1.86599622703439,-36.2911189895468));
#26834=CARTESIAN_POINT('Ctrl Pts',(3.68838450623552,1.75990559682896,-36.2969313398707));
#26835=CARTESIAN_POINT('Ctrl Pts',(3.73826755215734,1.65131880808949,-36.3027436901945));
#26836=CARTESIAN_POINT('Ctrl Pts',(3.78332609109917,1.54067150567805,-36.3085560405183));
#26837=CARTESIAN_POINT('Ctrl Pts',(3.82990654245871,1.42628694263898,-36.3145647107483));
#26838=CARTESIAN_POINT('Ctrl Pts',(3.8713305729448,1.30970058469697,-36.3205733809782));
#26839=CARTESIAN_POINT('Ctrl Pts',(3.90739600376305,1.19141993846693,-36.3265820512081));
#26840=CARTESIAN_POINT('Ctrl Pts',(3.94224421918767,1.07713128734392,-36.3323879276343));
#26841=CARTESIAN_POINT('Ctrl Pts',(3.97208957743956,0.961261289019829,-36.3381938040605));
#26842=CARTESIAN_POINT('Ctrl Pts',(3.99679955667867,0.844285676612574,-36.3439996804867));
#26843=CARTESIAN_POINT('Ctrl Pts',(4.02150595544695,0.727327013947177,-36.3498047156426));
#26844=CARTESIAN_POINT('Ctrl Pts',(4.04107837076155,0.609263454906169,-36.3556097507985));
#26845=CARTESIAN_POINT('Ctrl Pts',(4.05543513104386,0.490582202994803,-36.3614147859544));
#26846=CARTESIAN_POINT('Ctrl Pts',(4.06979319265331,0.371890193563596,-36.367220347291));
#26847=CARTESIAN_POINT('Ctrl Pts',(4.07893461027165,0.252580785023341,-36.3730259086276));
#26848=CARTESIAN_POINT('Ctrl Pts',(4.08282951957093,0.133146964367187,-36.3788314699642));
#26849=CARTESIAN_POINT('Ctrl Pts',(4.08672569932034,0.0136741865233215,
-36.3846389249716));
#26850=CARTESIAN_POINT('Ctrl Pts',(4.08537195399314,-0.105922676559767,
-36.390446379979));
#26851=CARTESIAN_POINT('Ctrl Pts',(4.07879053171232,-0.225150612732684,
-36.3962538349864));
#26852=CARTESIAN_POINT('Ctrl Pts',(4.07220185512428,-0.344509966711937,
-36.4020676912033));
#26853=CARTESIAN_POINT('Ctrl Pts',(4.06037402255944,-0.463499174477577,
-36.4078815474203));
#26854=CARTESIAN_POINT('Ctrl Pts',(4.04338117799063,-0.581630165544313,
-36.4136954036372));
#26855=CARTESIAN_POINT('Ctrl Pts',(4.02637715346937,-0.699838877492785,
-36.4195130849133));
#26856=CARTESIAN_POINT('Ctrl Pts',(4.00420142488322,-0.817187848249899,
-36.4253307661893));
#26857=CARTESIAN_POINT('Ctrl Pts',(3.97697895021239,-0.933200637359189,
-36.4311484474654));
#26858=CARTESIAN_POINT('Ctrl Pts',(3.94971790150782,-1.04937781568341,-36.4369743723504));
#26859=CARTESIAN_POINT('Ctrl Pts',(3.91739594400822,-1.16421464215036,-36.4428002972354));
#26860=CARTESIAN_POINT('Ctrl Pts',(3.8801874447013,-1.27725110842873,-36.4486262221203));
#26861=CARTESIAN_POINT('Ctrl Pts',(3.87137824570172,-1.30401275547719,-36.4500055234258));
#26862=CARTESIAN_POINT('Ctrl Pts',(3.86229535711031,-1.33067358484663,-36.4513848247312));
#26863=CARTESIAN_POINT('Ctrl Pts',(3.85294147739799,-1.35722767866935,-36.4527641260367));
#26864=CARTESIAN_POINT('Ctrl Pts',(3.81343551102534,-1.46937848345629,-36.458589583779));
#26865=CARTESIAN_POINT('Ctrl Pts',(3.76896558452616,-1.57998236229261,-36.4644150415214));
#26866=CARTESIAN_POINT('Ctrl Pts',(3.71967212011802,-1.6885687190093,-36.4702404992638));
#26867=CARTESIAN_POINT('Ctrl Pts',(3.67044052693488,-1.79701878238592,-36.4760586451198));
#26868=CARTESIAN_POINT('Ctrl Pts',(3.61639760517508,-1.9034559921634,-36.4818767909759));
#26869=CARTESIAN_POINT('Ctrl Pts',(3.55773307516494,-2.00742630397168,-36.487694936832));
#26870=CARTESIAN_POINT('Ctrl Pts',(3.49912691825589,-2.11129316196348,-36.4935072934451));
#26871=CARTESIAN_POINT('Ctrl Pts',(3.43590850110133,-2.21269765195627,-36.4993196500582));
#26872=CARTESIAN_POINT('Ctrl Pts',(3.36831476321685,-2.31120761851795,-36.5051320066713));
#26873=CARTESIAN_POINT('Ctrl Pts',(3.29843805929445,-2.41304474104254,-36.5111406745577));
#26874=CARTESIAN_POINT('Ctrl Pts',(3.22388543561436,-2.51178795092408,-36.5171493424441));
#26875=CARTESIAN_POINT('Ctrl Pts',(3.14496939547503,-2.60698916405984,-36.5231580103305));
#26876=CARTESIAN_POINT('Ctrl Pts',(3.06871667421491,-2.69897745384287,-36.5289638930975));
#26877=CARTESIAN_POINT('Ctrl Pts',(2.98839058523314,-2.78765862612755,-36.5347697758645));
#26878=CARTESIAN_POINT('Ctrl Pts',(2.90431543353171,-2.87266024140508,-36.5405756586315));
#26879=CARTESIAN_POINT('Ctrl Pts',(2.82025246417479,-2.95764954009513,-36.5463807001361));
#26880=CARTESIAN_POINT('Ctrl Pts',(2.7324417993068,-3.03896005209655,-36.5521857416407));
#26881=CARTESIAN_POINT('Ctrl Pts',(2.64124530328099,-3.11625548501661,-36.5579907831453));
#26882=CARTESIAN_POINT('Ctrl Pts',(2.55004054100715,-3.19355792416221,-36.5637963508314));
#26883=CARTESIAN_POINT('Ctrl Pts',(2.45544964865562,-3.26684429681266,-36.5696019185176));
#26884=CARTESIAN_POINT('Ctrl Pts',(2.35786782809665,-3.33581838612758,-36.5754074862037));
#26885=CARTESIAN_POINT('Ctrl Pts',(2.26025417822233,-3.40481497346545,-36.5812149475545));
#26886=CARTESIAN_POINT('Ctrl Pts',(2.15964799291212,-3.46949624467323,-36.5870224089053));
#26887=CARTESIAN_POINT('Ctrl Pts',(2.05647317141115,-3.5296094819776,-36.5928298702561));
#26888=CARTESIAN_POINT('Ctrl Pts',(1.9531846273436,-3.58978897800219,-36.5986437327753));
#26889=CARTESIAN_POINT('Ctrl Pts',(1.84732214855163,-3.64539018445363,-36.6044575952946));
#26890=CARTESIAN_POINT('Ctrl Pts',(1.73933406526962,-3.69620643489953,-36.6102714578138));
#26891=CARTESIAN_POINT('Ctrl Pts',(1.63127493472827,-3.74705611825037,-36.6160891453754));
#26892=CARTESIAN_POINT('Ctrl Pts',(1.52108779013081,-3.79311441897661,-36.6219068329371));
#26893=CARTESIAN_POINT('Ctrl Pts',(1.40923921274804,-3.83422349912643,-36.6277245204987));
#26894=CARTESIAN_POINT('Ctrl Pts',(1.29723214835793,-3.87539082995086,-36.6335504515974));
#26895=CARTESIAN_POINT('Ctrl Pts',(1.1835593398292,-3.91159481993312,-36.639376382696));
#26896=CARTESIAN_POINT('Ctrl Pts',(1.06870083667109,-3.94272792894698,-36.6452023137947));
#26897=CARTESIAN_POINT('Ctrl Pts',(1.04150904165693,-3.95009843348239,-36.6465815545113));
#26898=CARTESIAN_POINT('Ctrl Pts',(1.01425082784076,-3.95718495949799,-36.6479607952279));
#26899=CARTESIAN_POINT('Ctrl Pts',(0.986932620584834,-3.96398650381476,
-36.6493400359445));
#26900=CARTESIAN_POINT('Ctrl Pts',(0.871549970582555,-3.99271387234318,
-36.6551654712441));
#26901=CARTESIAN_POINT('Ctrl Pts',(0.75472741436091,-4.01644522789889,-36.6609909065437));
#26902=CARTESIAN_POINT('Ctrl Pts',(0.636935158523994,-4.03503886026343,
-36.6668163418433));
#26903=CARTESIAN_POINT('Ctrl Pts',(0.519290752117458,-4.05360915443877,
-36.6726344652252));
#26904=CARTESIAN_POINT('Ctrl Pts',(0.400679466532992,-4.06705448897578,
-36.678452588607));
#26905=CARTESIAN_POINT('Ctrl Pts',(0.281584815870499,-4.07528342467995,
-36.6842707119888));
#26906=CARTESIAN_POINT('Ctrl Pts',(0.162608668781168,-4.08350417228937,
-36.6900830461231));
#26907=CARTESIAN_POINT('Ctrl Pts',(0.0431505182011207,-4.08651881918968,
-36.6958953802575));
#26908=CARTESIAN_POINT('Ctrl Pts',(-0.076298414708443,-4.0842873983001,
-36.7017077143918));
#26909=CARTESIAN_POINT('Ctrl Pts',(-0.199782364003948,-4.08198059942568,
-36.7077163907026));
#26910=CARTESIAN_POINT('Ctrl Pts',(-0.323256023145913,-4.07406696201024,
-36.7137250670135));
#26911=CARTESIAN_POINT('Ctrl Pts',(-0.446173281238826,-4.06056084834455,
-36.7197337433243));
#26912=CARTESIAN_POINT('Ctrl Pts',(-0.564941610016865,-4.04751061786228,
-36.7255396037436));
#26913=CARTESIAN_POINT('Ctrl Pts',(-0.683190055011587,-4.02923940164376,
-36.7313454641629));
#26914=CARTESIAN_POINT('Ctrl Pts',(-0.800429181120055,-4.00581304181954,
-36.7371513245822));
#26915=CARTESIAN_POINT('Ctrl Pts',(-0.917651321175641,-3.9823900760959,
-36.7429563438262));
#26916=CARTESIAN_POINT('Ctrl Pts',(-1.03386403316443,-3.95381353209138,
-36.7487613630702));
#26917=CARTESIAN_POINT('Ctrl Pts',(-1.14858739600384,-3.92020050427795,
-36.7545663823143));
#26918=CARTESIAN_POINT('Ctrl Pts',(-1.26332115985405,-3.88658442905154,
-36.760371927851));
#26919=CARTESIAN_POINT('Ctrl Pts',(-1.37656491451374,-3.84793107688222,
-36.7661774733877));
#26920=CARTESIAN_POINT('Ctrl Pts',(-1.48785385632197,-3.80440743115506,
-36.7719830189244));
#26921=CARTESIAN_POINT('Ctrl Pts',(-1.59917910117831,-3.76086958778185,
-36.7777904582612));
#26922=CARTESIAN_POINT('Ctrl Pts',(-1.70854788519361,-3.71245843974745,
-36.7835978975979));
#26923=CARTESIAN_POINT('Ctrl Pts',(-1.81551593411231,-3.65938886878455,
-36.7894053369346));
#26924=CARTESIAN_POINT('Ctrl Pts',(-1.92260189275794,-3.60626079980581,
-36.7952191777491));
#26925=CARTESIAN_POINT('Ctrl Pts',(-2.02728146845473,-3.548464239783,-36.8010330185636));
#26926=CARTESIAN_POINT('Ctrl Pts',(-2.12913539516145,-3.4862598108963,-36.8068468593781));
#26927=CARTESIAN_POINT('Ctrl Pts',(-2.23105633633623,-3.42401445480288,
-36.8126645253907));
#26928=CARTESIAN_POINT('Ctrl Pts',(-2.33014758821295,-3.35735568125718,
-36.8184821914033));
#26929=CARTESIAN_POINT('Ctrl Pts',(-2.42602061258807,-3.28658622088297,
-36.8242998574159));
#26930=CARTESIAN_POINT('Ctrl Pts',(-2.52202949385745,-3.21571647662643,
-36.8301257673537));
#26931=CARTESIAN_POINT('Ctrl Pts',(-2.61481072952792,-3.14072467505461,
-36.8359516772915));
#26932=CARTESIAN_POINT('Ctrl Pts',(-2.70401036796732,-3.06195247022635,
-36.8417775872292));
#26933=CARTESIAN_POINT('Ctrl Pts',(-2.72513096525623,-3.04330086978441,
-36.8431570401036));
#26934=CARTESIAN_POINT('Ctrl Pts',(-2.74605093321617,-3.02443747840542,
-36.8445364929779));
#26935=CARTESIAN_POINT('Ctrl Pts',(-2.76676589646178,-3.00536711138191,
-36.8459159458523));
#26936=CARTESIAN_POINT('Ctrl Pts',(-2.85296777305954,-2.92600894862088,
-36.8516563097158));
#26937=CARTESIAN_POINT('Ctrl Pts',(-2.9359102855324,-2.84279355617639,-36.8573966735792));
#26938=CARTESIAN_POINT('Ctrl Pts',(-3.0152216656466,-2.75602309624128,-36.8631370374427));
#26939=CARTESIAN_POINT('Ctrl Pts',(-3.0944324328739,-2.66936271163783,-36.8688701191912));
#26940=CARTESIAN_POINT('Ctrl Pts',(-3.17002094314047,-2.57915653263523,
-36.8746032009398));
#26941=CARTESIAN_POINT('Ctrl Pts',(-3.24164959019338,-2.48574595129894,
-36.8803362826884));
#26942=CARTESIAN_POINT('Ctrl Pts',(-3.31319919234215,-2.39243845204993,
-36.8860630377658));
#26943=CARTESIAN_POINT('Ctrl Pts',(-3.38079737053372,-2.29593391815368,
-36.8917897928432));
#26944=CARTESIAN_POINT('Ctrl Pts',(-3.44414503611396,-2.19660874308821,
-36.8975165479206));
#26945=CARTESIAN_POINT('Ctrl Pts',(-3.50745410289587,-2.09734408852285,
-36.9032398135898));
#26946=CARTESIAN_POINT('Ctrl Pts',(-3.56651757797437,-1.9952625620178,-36.908963079259));
#26947=CARTESIAN_POINT('Ctrl Pts',(-3.62107844800158,-1.89077123772773,
-36.9146863449282));
#26948=CARTESIAN_POINT('Ctrl Pts',(-3.67561984362926,-1.78631720950343,
-36.9204075677934));
#26949=CARTESIAN_POINT('Ctrl Pts',(-3.72566163443285,-1.67945546632966,
-36.9261287906586));
#26950=CARTESIAN_POINT('Ctrl Pts',(-3.77099212964895,-1.57061878192185,
-36.9318500135238));
#26951=CARTESIAN_POINT('Ctrl Pts',(-3.81631788456961,-1.46179347877154,
-36.93757063811));
#26952=CARTESIAN_POINT('Ctrl Pts',(-3.85693316314368,-1.35099403439447,
-36.9432912626961));
#26953=CARTESIAN_POINT('Ctrl Pts',(-3.89267423871781,-1.23867359349537,
-36.9490118872823));
#26954=CARTESIAN_POINT('Ctrl Pts',(-3.92843606666944,-1.12628793586306,
-36.9547358334405));
#26955=CARTESIAN_POINT('Ctrl Pts',(-3.95931790999905,-1.01237991932313,
-36.9604597795988));
#26956=CARTESIAN_POINT('Ctrl Pts',(-3.98520586797416,-0.897418068608123,
-36.9661837257571));
#26957=CARTESIAN_POINT('Ctrl Pts',(-4.01110192825184,-0.782420237623872,
-36.9719094633716));
#26958=CARTESIAN_POINT('Ctrl Pts',(-4.03200091337673,-0.666368329771364,
-36.9776352009861));
#26959=CARTESIAN_POINT('Ctrl Pts',(-4.04784031633376,-0.549739732476181,
-36.9833609386006));
#26960=CARTESIAN_POINT('Ctrl Pts',(-4.06369764127743,-0.43297917211602,
-36.9890931547796));
#26961=CARTESIAN_POINT('Ctrl Pts',(-4.07448391270157,-0.315641038569806,
-36.9948253709586));
#26962=CARTESIAN_POINT('Ctrl Pts',(-4.080188622196,-0.1982064764388,-37.0005575871376));
#26963=CARTESIAN_POINT('Ctrl Pts',(-4.08344869767159,-0.131096041391466,
-37.003833381883));
#26964=CARTESIAN_POINT('Ctrl Pts',(-4.08505020174386,-0.0639541194029987,
-37.0071091766283));
#26965=CARTESIAN_POINT('Ctrl Pts',(-4.08499880087778,0.00312998835824298,
-37.0103849713737));
#26966=CARTESIAN_POINT('Origin',(0.,0.,-25.2396150285955));
#26967=CARTESIAN_POINT('',(2.48705727606859,3.24064362520075,-34.9531798329663));
#26968=CARTESIAN_POINT('',(2.4870572760686,3.24064362520075,-35.057284109232));
#26969=CARTESIAN_POINT('',(2.4870572760686,3.24064362520075,-25.2396150285955));
#26970=CARTESIAN_POINT('',(-4.08499983154849,-0.00117313631325986,-35.8646150286259));
#26971=CARTESIAN_POINT('Ctrl Pts',(2.4870572760686,3.24064362520074,-35.057284109232));
#26972=CARTESIAN_POINT('Ctrl Pts',(2.54761296302863,3.19416968999538,-35.0610166734358));
#26973=CARTESIAN_POINT('Ctrl Pts',(2.60681072845989,3.14603993011952,-35.0647492376396));
#26974=CARTESIAN_POINT('Ctrl Pts',(2.66455867416279,3.09634495364193,-35.0684818018434));
#26975=CARTESIAN_POINT('Ctrl Pts',(2.75468648016539,3.0187854985867,-35.0743072527466));
#26976=CARTESIAN_POINT('Ctrl Pts',(2.84156927643091,2.93716357340725,-35.0801327036498));
#26977=CARTESIAN_POINT('Ctrl Pts',(2.92481966594463,2.85178100872132,-35.085958154553));
#26978=CARTESIAN_POINT('Ctrl Pts',(3.00796556229563,2.76650561343455,-35.091776293541));
#26979=CARTESIAN_POINT('Ctrl Pts',(3.08748783801294,2.67747925686239,-35.097594432529));
#26980=CARTESIAN_POINT('Ctrl Pts',(3.16303243065348,2.58504368292575,-35.1034125715171));
#26981=CARTESIAN_POINT('Ctrl Pts',(3.23850185363169,2.49270008580223,-35.1092249212417));
#26982=CARTESIAN_POINT('Ctrl Pts',(3.31000121079498,2.39695433415158,-35.1150372709663));
#26983=CARTESIAN_POINT('Ctrl Pts',(3.37721399111375,2.29818420894096,-35.1208496206909));
#26984=CARTESIAN_POINT('Ctrl Pts',(3.44669698281696,2.19607797619791,-35.1268582911518));
#26985=CARTESIAN_POINT('Ctrl Pts',(3.51159839093206,2.09073976606651,-35.1328669616126));
#26986=CARTESIAN_POINT('Ctrl Pts',(3.5716143222271,1.98262354804493,-35.1388756320735));
#26987=CARTESIAN_POINT('Ctrl Pts',(3.62960469625512,1.87815628766459,-35.1446815079454));
#26988=CARTESIAN_POINT('Ctrl Pts',(3.68303383120364,1.77109589607329,-35.1504873838173));
#26989=CARTESIAN_POINT('Ctrl Pts',(3.73167259726826,1.66187984728053,-35.1562932596892));
#26990=CARTESIAN_POINT('Ctrl Pts',(3.78030431573155,1.55267962354324,-35.1620982943083));
#26991=CARTESIAN_POINT('Ctrl Pts',(3.82414687977847,1.44132473641654,-35.1679033289274));
#26992=CARTESIAN_POINT('Ctrl Pts',(3.86301848424554,1.32827451619658,-35.1737083635465));
#26993=CARTESIAN_POINT('Ctrl Pts',(3.90189361223779,1.21521404851444,-35.1795139243642));
#26994=CARTESIAN_POINT('Ctrl Pts',(3.93579675208558,1.10045832805974,-35.185319485182));
#26995=CARTESIAN_POINT('Ctrl Pts',(3.9645955489872,0.984483180633828,-35.1911250459997));
#26996=CARTESIAN_POINT('Ctrl Pts',(3.99340373963669,0.868470203804875,-35.1969325005068));
#26997=CARTESIAN_POINT('Ctrl Pts',(4.01710417778607,0.751237404722748,-35.2027399550139));
#26998=CARTESIAN_POINT('Ctrl Pts',(4.03561546230076,0.633271537682692,-35.2085474095209));
#26999=CARTESIAN_POINT('Ctrl Pts',(4.05414715079073,0.515175643326956,-35.2143612652671));
#27000=CARTESIAN_POINT('Ctrl Pts',(4.06747820553746,0.396345471471962,-35.2201751210133));
#27001=CARTESIAN_POINT('Ctrl Pts',(4.07557900651325,0.277273802708554,-35.2259889767595));
#27002=CARTESIAN_POINT('Ctrl Pts',(4.08368513720139,0.158123793822433,-35.2318066575816));
#27003=CARTESIAN_POINT('Ctrl Pts',(4.08655415117709,0.0387323785405584,
-35.2376243384036));
#27004=CARTESIAN_POINT('Ctrl Pts',(4.08420855108277,-0.0804084029337425,
-35.2434420192257));
#27005=CARTESIAN_POINT('Ctrl Pts',(4.08185962728007,-0.199718006542317,
-35.2492679436843));
#27006=CARTESIAN_POINT('Ctrl Pts',(4.07428136757816,-0.318775861817394,
-35.2550938681429));
#27007=CARTESIAN_POINT('Ctrl Pts',(4.0615480281694,-0.437095658721621,-35.2609197926015));
#27008=CARTESIAN_POINT('Ctrl Pts',(4.05853336904505,-0.465108251795378,
-35.2622990989847));
#27009=CARTESIAN_POINT('Ctrl Pts',(4.055229981517,-0.493079524776221,-35.263678405368));
#27010=CARTESIAN_POINT('Ctrl Pts',(4.05163926609921,-0.521003126097207,
-35.2650577117513));
#27011=CARTESIAN_POINT('Ctrl Pts',(4.03647400820025,-0.638937455674511,
-35.2708831628355));
#27012=CARTESIAN_POINT('Ctrl Pts',(4.01613100473269,-0.756397754621066,
-35.2767086139198));
#27013=CARTESIAN_POINT('Ctrl Pts',(3.99064910219284,-0.872894462788894,
-35.2825340650041));
#27014=CARTESIAN_POINT('Ctrl Pts',(3.96519918371308,-0.989244948055602,
-35.2883522041705));
#27015=CARTESIAN_POINT('Ctrl Pts',(3.93462328211081,-1.10463385306709,-35.2941703433369));
#27016=CARTESIAN_POINT('Ctrl Pts',(3.8990119140391,-1.2185774879675,-35.2999884825034));
#27017=CARTESIAN_POINT('Ctrl Pts',(3.86343598061113,-1.33240774468762,-35.3058008324036));
#27018=CARTESIAN_POINT('Ctrl Pts',(3.82283466967113,-1.44479520503797,-35.3116131823039));
#27019=CARTESIAN_POINT('Ctrl Pts',(3.77734925186654,-1.55526770345922,-35.3174255322041));
#27020=CARTESIAN_POINT('Ctrl Pts',(3.7303274985294,-1.66947156970967,-35.3234342025981));
#27021=CARTESIAN_POINT('Ctrl Pts',(3.67808595754768,-1.7816283891354,-35.329442872992));
#27022=CARTESIAN_POINT('Ctrl Pts',(3.62083645882539,-1.89123460692766,-35.335451543386));
#27023=CARTESIAN_POINT('Ctrl Pts',(3.56551914715493,-1.9971415833371,-35.3412574194255));
#27024=CARTESIAN_POINT('Ctrl Pts',(3.50552666701297,-2.10066695656878,-35.3470632954651));
#27025=CARTESIAN_POINT('Ctrl Pts',(3.44109821563374,-2.20137867491313,-35.3528691715046));
#27026=CARTESIAN_POINT('Ctrl Pts',(3.37667909976621,-2.30207580039664,-35.3586742062881));
#27027=CARTESIAN_POINT('Ctrl Pts',(3.3078255107762,-2.39995973817966,-35.3644792410716));
#27028=CARTESIAN_POINT('Ctrl Pts',(3.23482093722727,-2.4946259246781,-35.3702842758551));
#27029=CARTESIAN_POINT('Ctrl Pts',(3.16180974620552,-2.58930069215833,-35.3760898368339));
#27030=CARTESIAN_POINT('Ctrl Pts',(3.08464707169867,-2.68075680532705,-35.3818953978126));
#27031=CARTESIAN_POINT('Ctrl Pts',(3.00365738718824,-2.76862191358616,-35.3877009587914));
#27032=CARTESIAN_POINT('Ctrl Pts',(2.92264128507332,-2.85651568210852,-35.3935084134559));
#27033=CARTESIAN_POINT('Ctrl Pts',(2.83779596670142,-2.94081581632806,-35.3993158681204));
#27034=CARTESIAN_POINT('Ctrl Pts',(2.74948306936067,-3.02118649727206,-35.405123322785));
#27035=CARTESIAN_POINT('Ctrl Pts',(2.66107282964314,-3.10164576633108,-35.4109371786826));
#27036=CARTESIAN_POINT('Ctrl Pts',(2.56918768375993,-3.17816666203462,-35.4167510345802));
#27037=CARTESIAN_POINT('Ctrl Pts',(2.47422279488574,-3.2504532855077,-35.4225648904778));
#27038=CARTESIAN_POINT('Ctrl Pts',(2.3791954263768,-3.32278746805114,-35.428382571448));
#27039=CARTESIAN_POINT('Ctrl Pts',(2.28108461392576,-3.39088159813571,-35.4342002524182));
#27040=CARTESIAN_POINT('Ctrl Pts',(2.18031358449793,-3.45448370574444,-35.4400179333884));
#27041=CARTESIAN_POINT('Ctrl Pts',(2.07939976292653,-3.51817593728394,-35.4458438579892));
#27042=CARTESIAN_POINT('Ctrl Pts',(1.97581855388177,-3.57736324060849,-35.4516697825899));
#27043=CARTESIAN_POINT('Ctrl Pts',(1.87001687863024,-3.63184001212031,-35.4574957071907));
#27044=CARTESIAN_POINT('Ctrl Pts',(1.844968020134,-3.64473754836146,-35.4588750120135));
#27045=CARTESIAN_POINT('Ctrl Pts',(1.81979478230675,-3.65737126489159,-35.4602543168362));
#27046=CARTESIAN_POINT('Ctrl Pts',(1.79450323923852,-3.66973883598853,-35.461633621659));
#27047=CARTESIAN_POINT('Ctrl Pts',(1.68768517348913,-3.721972897747,-35.4674590737816));
#27048=CARTESIAN_POINT('Ctrl Pts',(1.57841371056643,-3.76962278931479,-35.4732845259041));
#27049=CARTESIAN_POINT('Ctrl Pts',(1.4671190004969,-3.81245155226673,-35.4791099780267));
#27050=CARTESIAN_POINT('Ctrl Pts',(1.35596398381554,-3.85522655799154,-35.4849281182371));
#27051=CARTESIAN_POINT('Ctrl Pts',(1.24279114860668,-3.89319232601522,-35.4907462584475));
#27052=CARTESIAN_POINT('Ctrl Pts',(1.12805417629044,-3.92615827181657,-35.4965643986578));
#27053=CARTESIAN_POINT('Ctrl Pts',(1.01343137144864,-3.95909141529886,-35.5023767496064));
#27054=CARTESIAN_POINT('Ctrl Pts',(0.897247915708348,-3.98703452188866,
-35.508189100555));
#27055=CARTESIAN_POINT('Ctrl Pts',(0.779975796753611,-4.00984572726665,
-35.5140014515035));
#27056=CARTESIAN_POINT('Ctrl Pts',(0.658742672748291,-4.03342740818918,
-35.5200101215062));
#27057=CARTESIAN_POINT('Ctrl Pts',(0.536346456490509,-4.05152421987872,
-35.5260187915088));
#27058=CARTESIAN_POINT('Ctrl Pts',(0.413324171960105,-4.06403594089342,
-35.5320274615114));
#27059=CARTESIAN_POINT('Ctrl Pts',(0.294453895636837,-4.07612539070306,
-35.5378333386034));
#27060=CARTESIAN_POINT('Ctrl Pts',(0.174999567079131,-4.08300061619102,
-35.5436392156953));
#27061=CARTESIAN_POINT('Ctrl Pts',(0.0554535665679267,-4.08462359366869,
-35.5494450927872));
#27062=CARTESIAN_POINT('Ctrl Pts',(-0.0640751120410736,-4.08624633598117,
-35.5552501286227));
#27063=CARTESIAN_POINT('Ctrl Pts',(-0.183695028315242,-4.08261833826464,
-35.5610551644582));
#27064=CARTESIAN_POINT('Ctrl Pts',(-0.302912381463827,-4.07375368538108,
-35.5668602002938));
#27065=CARTESIAN_POINT('Ctrl Pts',(-0.422140540992919,-4.06488822896674,
-35.572665762323));
#27066=CARTESIAN_POINT('Ctrl Pts',(-0.540965657934851,-4.0507852038775,
-35.5784713243523));
#27067=CARTESIAN_POINT('Ctrl Pts',(-0.658898275603472,-4.03151064272523,
-35.5842768863816));
#27068=CARTESIAN_POINT('Ctrl Pts',(-0.776869361039087,-4.01222979451393,
-35.590084342094));
#27069=CARTESIAN_POINT('Ctrl Pts',(-0.893946965763019,-3.9877741211649,
-35.5958917978064));
#27070=CARTESIAN_POINT('Ctrl Pts',(-1.00965168584978,-3.9582607889401,-35.6016992535188));
#27071=CARTESIAN_POINT('Ctrl Pts',(-1.12548394058473,-3.9287149258692,-35.6075131104551));
#27072=CARTESIAN_POINT('Ctrl Pts',(-1.23993989458916,-3.8941003773362,-35.6133269673914));
#27073=CARTESIAN_POINT('Ctrl Pts',(-1.35255502787744,-3.85458427026359,
-35.6191408243277));
#27074=CARTESIAN_POINT('Ctrl Pts',(-1.46524425321756,-3.81504216464736,
-35.6249585063325));
#27075=CARTESIAN_POINT('Ctrl Pts',(-1.5760898680173,-3.77059222953675,-35.6307761883372));
#27076=CARTESIAN_POINT('Ctrl Pts',(-1.68464858914159,-3.72144919770555,
-35.6365938703419));
#27077=CARTESIAN_POINT('Ctrl Pts',(-1.79336113725128,-3.67223653052527,
-35.6424197959634));
#27078=CARTESIAN_POINT('Ctrl Pts',(-1.89977996141944,-3.61831767766219,
-35.6482457215848));
#27079=CARTESIAN_POINT('Ctrl Pts',(-2.00348745511604,-3.55995267063941,
-35.6540716472062));
#27080=CARTESIAN_POINT('Ctrl Pts',(-2.02804032700518,-3.54613468614128,
-35.6554509419931));
#27081=CARTESIAN_POINT('Ctrl Pts',(-2.05244135994231,-3.53206767651095,
-35.65683023678));
#27082=CARTESIAN_POINT('Ctrl Pts',(-2.07668526966656,-3.51775543361813,
-35.6582095315669));
#27083=CARTESIAN_POINT('Ctrl Pts',(-2.1790793810782,-3.45730770014667,-35.6640349807492));
#27084=CARTESIAN_POINT('Ctrl Pts',(-2.27899585314593,-3.39228885905836,
-35.6698604299315));
#27085=CARTESIAN_POINT('Ctrl Pts',(-2.37600012791215,-3.32292768385974,
-35.6756858791139));
#27086=CARTESIAN_POINT('Ctrl Pts',(-2.47288264606866,-3.2536535685516,-35.6815040163819));
#27087=CARTESIAN_POINT('Ctrl Pts',(-2.56685990835396,-3.18004819524483,
-35.6873221536499));
#27088=CARTESIAN_POINT('Ctrl Pts',(-2.65752312928818,-3.10238550430123,
-35.693140290918));
#27089=CARTESIAN_POINT('Ctrl Pts',(-2.74809613698508,-3.02480009058974,
-35.6989526389255));
#27090=CARTESIAN_POINT('Ctrl Pts',(-2.83536135550246,-2.94316565481485,
-35.7047649869331));
#27091=CARTESIAN_POINT('Ctrl Pts',(-2.91894060623687,-2.85779823242677,
-35.7105773349407));
#27092=CARTESIAN_POINT('Ctrl Pts',(-3.00534290497359,-2.76954736314105,
-35.7165860060463));
#27093=CARTESIAN_POINT('Ctrl Pts',(-3.08780546588963,-2.67730712428515,
-35.7225946771519));
#27094=CARTESIAN_POINT('Ctrl Pts',(-3.16594909253999,-2.58147077137147,
-35.7286033482575));
#27095=CARTESIAN_POINT('Ctrl Pts',(-3.24145531609227,-2.48886896367815,
-35.7344092224305));
#27096=CARTESIAN_POINT('Ctrl Pts',(-3.31292915685849,-2.39291020915543,
-35.7402150966034));
#27097=CARTESIAN_POINT('Ctrl Pts',(-3.38006791958474,-2.29398471202275,
-35.7460209707764));
#27098=CARTESIAN_POINT('Ctrl Pts',(-3.44719695422765,-2.19507354871812,
-35.7518260037061));
#27099=CARTESIAN_POINT('Ctrl Pts',(-3.5099919309662,-2.09319683522284,-35.7576310366359));
#27100=CARTESIAN_POINT('Ctrl Pts',(-3.56819288252017,-1.98877463608433,
-35.7634360695656));
#27101=CARTESIAN_POINT('Ctrl Pts',(-3.62639910982831,-1.88434297136432,
-35.7692416287054));
#27102=CARTESIAN_POINT('Ctrl Pts',(-3.68001028532705,-1.77736571864468,
-35.7750471878452));
#27103=CARTESIAN_POINT('Ctrl Pts',(-3.72881220759218,-1.6682879009666,-35.7808527469851));
#27104=CARTESIAN_POINT('Ctrl Pts',(-3.77763004844898,-1.55917450343512,
-35.7866601998274));
#27105=CARTESIAN_POINT('Ctrl Pts',(-3.82163534966172,-1.44795955050639,
-35.7924676526698));
#27106=CARTESIAN_POINT('Ctrl Pts',(-3.86066213725814,-1.33510780910808,
-35.7982751055122));
#27107=CARTESIAN_POINT('Ctrl Pts',(-3.89973194214464,-1.22213167683893,
-35.8040889596215));
#27108=CARTESIAN_POINT('Ctrl Pts',(-3.93381214655235,-1.10751554075407,
-35.8099028137307));
#27109=CARTESIAN_POINT('Ctrl Pts',(-3.96278668303157,-0.991739232251915,
-35.81571666784));
#27110=CARTESIAN_POINT('Ctrl Pts',(-3.99178028263405,-0.875886751416868,
-35.8215343470396));
#27111=CARTESIAN_POINT('Ctrl Pts',(-4.01566144296388,-0.758872976833628,
-35.8273520262391));
#27112=CARTESIAN_POINT('Ctrl Pts',(-4.03436553274525,-0.64118620399781,
-35.8331697054386));
#27113=CARTESIAN_POINT('Ctrl Pts',(-4.05309612627992,-0.523332668639482,
-35.8389956283077));
#27114=CARTESIAN_POINT('Ctrl Pts',(-4.06663496159447,-0.404804635581587,
-35.8448215511767));
#27115=CARTESIAN_POINT('Ctrl Pts',(-4.07496936030051,-0.286093887757309,
-35.8506474740457));
#27116=CARTESIAN_POINT('Ctrl Pts',(-4.07694257960332,-0.257988400208571,
-35.8520267965221));
#27117=CARTESIAN_POINT('Ctrl Pts',(-4.07862430221465,-0.229872661637646,
-35.8534061189984));
#27118=CARTESIAN_POINT('Ctrl Pts',(-4.08001478647782,-0.201753171281986,
-35.8547854414747));
#27119=CARTESIAN_POINT('Ctrl Pts',(-4.08331782992595,-0.134956371890456,
-35.858061970515));
#27120=CARTESIAN_POINT('Ctrl Pts',(-4.08498061775683,-0.0680778031167455,
-35.8613384995552));
#27121=CARTESIAN_POINT('Ctrl Pts',(-4.08499983154831,-0.00117313693436384,
-35.8646150285955));
#27122=CARTESIAN_POINT('Ctrl Pts',(-4.08499983154849,-0.00117313631325986,
-35.8646150286259));
#27123=CARTESIAN_POINT('Ctrl Pts',(-4.08503373102818,0.116868874034736,
-35.8703959120372));
#27124=CARTESIAN_POINT('Ctrl Pts',(-4.07994688931445,0.235111042198397,
-35.8761767954485));
#27125=CARTESIAN_POINT('Ctrl Pts',(-4.06971340855855,0.353069075676062,
-35.8819576788598));
#27126=CARTESIAN_POINT('Ctrl Pts',(-4.05949248493801,0.470882367102661,
-35.8877314687574));
#27127=CARTESIAN_POINT('Ctrl Pts',(-4.04413751518853,0.588411807383864,
-35.8935052586551));
#27128=CARTESIAN_POINT('Ctrl Pts',(-4.02367460274052,0.705172100455546,
-35.8992790485527));
#27129=CARTESIAN_POINT('Ctrl Pts',(-4.00323126266263,0.82182071462144,-35.9050473159348));
#27130=CARTESIAN_POINT('Ctrl Pts',(-3.97768976799366,0.937701238296356,
-35.9108155833168));
#27131=CARTESIAN_POINT('Ctrl Pts',(-3.94712805194677,1.0523331894105,-35.9165838506989));
#27132=CARTESIAN_POINT('Ctrl Pts',(-3.91658616023214,1.16689078272738,-35.9223483764046));
#27133=CARTESIAN_POINT('Ctrl Pts',(-3.88103063010538,1.28020101451192,-35.9281129021103));
#27134=CARTESIAN_POINT('Ctrl Pts',(-3.84059040645634,1.39179392506057,-35.9338774278161));
#27135=CARTESIAN_POINT('Ctrl Pts',(-3.80016369775302,1.50334954174702,-35.9396400270426));
#27136=CARTESIAN_POINT('Ctrl Pts',(-3.75485568164683,1.6131885883631,-35.945402626269));
#27137=CARTESIAN_POINT('Ctrl Pts',(-3.70484486777294,1.72085720085558,-35.9511652254955));
#27138=CARTESIAN_POINT('Ctrl Pts',(-3.65483852056453,1.82851619703436,-35.9569273100413));
#27139=CARTESIAN_POINT('Ctrl Pts',(-3.60013038570784,1.93400476833678,-35.962689394587));
#27140=CARTESIAN_POINT('Ctrl Pts',(-3.54094643027633,2.03689061510757,-35.9684514791327));
#27141=CARTESIAN_POINT('Ctrl Pts',(-3.48175326739319,2.13979246818365,-35.9742144601058));
#27142=CARTESIAN_POINT('Ctrl Pts',(-3.41808310698881,2.24009043237277,-35.9799774410789));
#27143=CARTESIAN_POINT('Ctrl Pts',(-3.3502066488331,2.33737896159662,-35.9857404220519));
#27144=CARTESIAN_POINT('Ctrl Pts',(-3.28226204563824,2.43476516431158,-35.9915091888095));
#27145=CARTESIAN_POINT('Ctrl Pts',(-3.21010294911753,2.52913555748799,-35.9972779555672));
#27146=CARTESIAN_POINT('Ctrl Pts',(-3.13404206357346,2.62011552107006,-36.0030467223248));
#27147=CARTESIAN_POINT('Ctrl Pts',(-3.05794147341163,2.71114297719249,-36.008818500442));
#27148=CARTESIAN_POINT('Ctrl Pts',(-2.97793531758722,2.79877617279207,-36.0145902785593));
#27149=CARTESIAN_POINT('Ctrl Pts',(-2.89437384388307,2.88267671649902,-36.0203620566765));
#27150=CARTESIAN_POINT('Ctrl Pts',(-2.81068169672052,2.96670846390213,-36.0261428607022));
#27151=CARTESIAN_POINT('Ctrl Pts',(-2.72342343142299,3.04699561907668,-36.0319236647278));
#27152=CARTESIAN_POINT('Ctrl Pts',(-2.63298340357745,3.12323924739775,-36.0377044687535));
#27153=CARTESIAN_POINT('Ctrl Pts',(-2.56176327342611,3.18327993139126,-36.0422567629632));
#27154=CARTESIAN_POINT('Ctrl Pts',(-2.48857073233364,3.24081387347772,-36.0468090571729));
#27155=CARTESIAN_POINT('Ctrl Pts',(-2.41360551266508,3.29571440346896,-36.0513613513826));
#27156=CARTESIAN_POINT('Ctrl Pts',(-2.31767438385452,3.36596924748385,-36.0571868091634));
#27157=CARTESIAN_POINT('Ctrl Pts',(-2.21851980173033,3.43214448006078,-36.0630122669443));
#27158=CARTESIAN_POINT('Ctrl Pts',(-2.11652338183446,3.49393099161217,-36.0688377247252));
#27159=CARTESIAN_POINT('Ctrl Pts',(-2.01465498384444,3.5556399511576,-36.07465587062));
#27160=CARTESIAN_POINT('Ctrl Pts',(-1.90995218878251,3.6129709367171,-36.0804740165147));
#27161=CARTESIAN_POINT('Ctrl Pts',(-1.802827953626,3.66565633545,-36.0862921624095));
#27162=CARTESIAN_POINT('Ctrl Pts',(-1.6958103105392,3.71828931051157,-36.0921045190614));
#27163=CARTESIAN_POINT('Ctrl Pts',(-1.58637638474194,3.7662857157977,-36.0979168757133));
#27164=CARTESIAN_POINT('Ctrl Pts',(-1.47496574524972,3.80942266627634,-36.1037292323652));
#27165=CARTESIAN_POINT('Ctrl Pts',(-1.35979223299051,3.85401655890115,-36.1097379002371));
#27166=CARTESIAN_POINT('Ctrl Pts',(-1.24250649722304,3.89341670215756,-36.115746568109));
#27167=CARTESIAN_POINT('Ctrl Pts',(-1.12361946629171,3.92742973138544,-36.1217552359808));
#27168=CARTESIAN_POINT('Ctrl Pts',(-1.00874472476286,3.96029486318795,-36.1275611187866));
#27169=CARTESIAN_POINT('Ctrl Pts',(-0.892375451068235,3.98813050942876,
-36.1333670015924));
#27170=CARTESIAN_POINT('Ctrl Pts',(-0.774989601447213,4.01081240120361,
-36.1391728843982));
#27171=CARTESIAN_POINT('Ctrl Pts',(-0.657620760834644,4.03349100641122,
-36.1449779259415));
#27172=CARTESIAN_POINT('Ctrl Pts',(-0.539236037740283,4.05101726491168,
-36.1507829674848));
#27173=CARTESIAN_POINT('Ctrl Pts',(-0.420323977030102,4.06331794895915,
-36.1565880090282));
#27174=CARTESIAN_POINT('Ctrl Pts',(-0.301401137875816,4.07561974796699,
-36.1623935767529));
#27175=CARTESIAN_POINT('Ctrl Pts',(-0.181951271937012,4.08269498879295,
-36.1681991444776));
#27176=CARTESIAN_POINT('Ctrl Pts',(-0.0624678101101076,4.08452234327345,
-36.1740047122023));
#27177=CARTESIAN_POINT('Ctrl Pts',(0.0570546249246556,4.08635029380185,
-36.1798121735916));
#27178=CARTESIAN_POINT('Ctrl Pts',(0.176610269889323,4.08292694740399,-36.1856196349809));
#27179=CARTESIAN_POINT('Ctrl Pts',(0.295706570594373,4.07428308099809,-36.1914270963702));
#27180=CARTESIAN_POINT('Ctrl Pts',(0.414934143016387,4.0656296870487,-36.1972409589275));
#27181=CARTESIAN_POINT('Ctrl Pts',(0.533700953405311,4.0517443169522,-36.2030548214848));
#27182=CARTESIAN_POINT('Ctrl Pts',(0.651520286599236,4.03270955018455,-36.2088686840421));
#27183=CARTESIAN_POINT('Ctrl Pts',(0.769417135199933,4.01366226010982,-36.2146863716415));
#27184=CARTESIAN_POINT('Ctrl Pts',(0.886364866532126,3.98945890871128,-36.220504059241));
#27185=CARTESIAN_POINT('Ctrl Pts',(1.00188927308175,3.96023268059892,-36.2263217468405));
#27186=CARTESIAN_POINT('Ctrl Pts',(1.11757737519665,3.93096503955855,-36.2321476779765));
#27187=CARTESIAN_POINT('Ctrl Pts',(1.23183773787284,3.89666043349518,-36.2379736091124));
#27188=CARTESIAN_POINT('Ctrl Pts',(1.34421343830507,3.85750116426166,-36.2437995402484));
#27189=CARTESIAN_POINT('Ctrl Pts',(1.3708174431377,3.84823053561219,-36.2451787805957));
#27190=CARTESIAN_POINT('Ctrl Pts',(1.39731591818232,3.83868802715506,-36.2465580209431));
#27191=CARTESIAN_POINT('Ctrl Pts',(1.42370299393941,3.82887643898937,-36.2479372612904));
#27192=CARTESIAN_POINT('Ctrl Pts',(1.53513902979679,3.78744083237973,-36.2537619717743));
#27193=CARTESIAN_POINT('Ctrl Pts',(1.64494289311034,3.7410700433615,-36.2595866822581));
#27194=CARTESIAN_POINT('Ctrl Pts',(1.75264666459632,3.68991255574972,-36.265411392742));
#27195=CARTESIAN_POINT('Ctrl Pts',(1.86023165407244,3.63881148760323,-36.271229679395));
#27196=CARTESIAN_POINT('Ctrl Pts',(1.96572079000933,3.58293438695173,-36.2770479660479));
#27197=CARTESIAN_POINT('Ctrl Pts',(2.06866334150336,3.52247881179151,-36.2828662527009));
#27198=CARTESIAN_POINT('Ctrl Pts',(2.17149549035802,3.46208807332871,-36.2886782994249));
#27199=CARTESIAN_POINT('Ctrl Pts',(2.2717861402928,3.39712883799668,-36.2944903461489));
#27200=CARTESIAN_POINT('Ctrl Pts',(2.36910736359178,3.3278454440937,-36.300302392873));
#27201=CARTESIAN_POINT('Ctrl Pts',(2.40893026840626,3.29949534832737,-36.3026806262698));
#27202=CARTESIAN_POINT('Ctrl Pts',(2.44825626195152,3.27042176671815,-36.3050588596666));
#27203=CARTESIAN_POINT('Ctrl Pts',(2.4870572760686,3.24064362520075,-36.3074370930634));
#27204=CARTESIAN_POINT('',(-4.08499997274305,-0.000471899681166237,-35.7603849713613));
#27205=CARTESIAN_POINT('Ctrl Pts',(-4.08499997274315,-0.000471898789758368,
-35.7603849714045));
#27206=CARTESIAN_POINT('Ctrl Pts',(-4.08501433561535,0.123860550885335,
-35.7664085457386));
#27207=CARTESIAN_POINT('Ctrl Pts',(-4.07934803225326,0.248109173627762,
-35.7724321200727));
#27208=CARTESIAN_POINT('Ctrl Pts',(-4.06804995739247,0.371745267836846,
-35.7784556944068));
#27209=CARTESIAN_POINT('Ctrl Pts',(-4.0567401997084,0.495509208485071,-35.7844854974441));
#27210=CARTESIAN_POINT('Ctrl Pts',(-4.03978709161203,0.618658998081323,
-35.7905153004814));
#27211=CARTESIAN_POINT('Ctrl Pts',(-4.01729103004486,0.740673868798626,
-35.7965451035186));
#27212=CARTESIAN_POINT('Ctrl Pts',(-3.99474910373659,0.862937502191047,
-35.8025872000569));
#27213=CARTESIAN_POINT('Ctrl Pts',(-3.96664170401674,0.984061236009943,
-35.8086292965951));
#27214=CARTESIAN_POINT('Ctrl Pts',(-3.93312004227064,1.10353601349887,-35.8146713931334));
#27215=CARTESIAN_POINT('Ctrl Pts',(-3.89956210969393,1.22314006409633,-35.8207200272909));
#27216=CARTESIAN_POINT('Ctrl Pts',(-3.86057834267863,1.34109125660982,-35.8267686614483));
#27217=CARTESIAN_POINT('Ctrl Pts',(-3.8163687679715,1.45689890756076,-35.8328172956058));
#27218=CARTESIAN_POINT('Ctrl Pts',(-3.77206545519309,1.57295210681002,-35.8388787547521));
#27219=CARTESIAN_POINT('Ctrl Pts',(-3.72251432922099,1.68685234722564,-35.8449402138983));
#27220=CARTESIAN_POINT('Ctrl Pts',(-3.66796273133031,1.79813080769222,-35.8510016730446));
#27221=CARTESIAN_POINT('Ctrl Pts',(-3.63185957703299,1.87177674261505,-35.8550132474675));
#27222=CARTESIAN_POINT('Ctrl Pts',(-3.59356715360858,1.94427485830153,-35.8590248218903));
#27223=CARTESIAN_POINT('Ctrl Pts',(-3.55316758175896,2.01549625053911,-35.8630363963132));
#27224=CARTESIAN_POINT('Ctrl Pts',(-3.49450089718306,2.11892118209559,-35.8688618484292));
#27225=CARTESIAN_POINT('Ctrl Pts',(-3.43122090777399,2.2199479492658,-35.8746873005453));
#27226=CARTESIAN_POINT('Ctrl Pts',(-3.36354883275847,2.31813809977946,-35.8805127526613));
#27227=CARTESIAN_POINT('Ctrl Pts',(-3.29596169746274,2.41620500530811,-35.8863308928651));
#27228=CARTESIAN_POINT('Ctrl Pts',(-3.22399367114155,2.51144204289252,-35.892149033069));
#27229=CARTESIAN_POINT('Ctrl Pts',(-3.14791157911544,2.60343574725226,-35.8979671732728));
#27230=CARTESIAN_POINT('Ctrl Pts',(-3.07190519154733,2.69533791451908,-35.9037795242149));
#27231=CARTESIAN_POINT('Ctrl Pts',(-2.99179314080898,2.78400285624025,-35.9095918751569));
#27232=CARTESIAN_POINT('Ctrl Pts',(-2.90788487067213,2.86904698095311,-35.9154042260989));
#27233=CARTESIAN_POINT('Ctrl Pts',(-2.82114249895735,2.95696357208256,-35.921412896104));
#27234=CARTESIAN_POINT('Ctrl Pts',(-2.73034317695568,3.04101005616904,-35.9274215661091));
#27235=CARTESIAN_POINT('Ctrl Pts',(-2.63587353853775,3.1208004884703,-35.9334302361142));
#27236=CARTESIAN_POINT('Ctrl Pts',(-2.54459225524385,3.19789798960409,-35.9392361131996));
#27237=CARTESIAN_POINT('Ctrl Pts',(-2.44988474113596,3.27102180295613,-35.9450419902849));
#27238=CARTESIAN_POINT('Ctrl Pts',(-2.35213590391129,3.33986252554375,-35.9508478673703));
#27239=CARTESIAN_POINT('Ctrl Pts',(-2.25440123023684,3.40869327329115,-35.9566529031993));
#27240=CARTESIAN_POINT('Ctrl Pts',(-2.15362644335434,3.47324192964129,-35.9624579390283));
#27241=CARTESIAN_POINT('Ctrl Pts',(-2.05022704626308,3.53324129642618,-35.9682629748573));
#27242=CARTESIAN_POINT('Ctrl Pts',(-1.94681827659931,3.59324610181547,-35.9740685368801));
#27243=CARTESIAN_POINT('Ctrl Pts',(-1.84078477663318,3.64870059296511,-35.9798740989029));
#27244=CARTESIAN_POINT('Ctrl Pts',(-1.73256779614466,3.69938289877683,-35.9856796609256));
#27245=CARTESIAN_POINT('Ctrl Pts',(-1.62431551697691,3.75008173636061,-35.9914871166316));
#27246=CARTESIAN_POINT('Ctrl Pts',(-1.51387871013573,3.7960051198592,-35.9972945723375));
#27247=CARTESIAN_POINT('Ctrl Pts',(-1.40171920096156,3.8369790567132,-36.0031020280434));
#27248=CARTESIAN_POINT('Ctrl Pts',(-1.28943606481925,3.87799815677826,-36.0089158849733));
#27249=CARTESIAN_POINT('Ctrl Pts',(-1.17542681963514,3.91405678070922,-36.0147297419032));
#27250=CARTESIAN_POINT('Ctrl Pts',(-1.0601692166547,3.94503057428682,-36.0205435988331));
#27251=CARTESIAN_POINT('Ctrl Pts',(-0.944835783080895,3.97602474622632,
-36.0263612808315));
#27252=CARTESIAN_POINT('Ctrl Pts',(-0.82825275337201,4.00192733692282,-36.0321789628299));
#27253=CARTESIAN_POINT('Ctrl Pts',(-0.710907231777638,4.02266527414428,
-36.0379966448282));
#27254=CARTESIAN_POINT('Ctrl Pts',(-0.593395432357713,4.04343259688519,
-36.0438225704434));
#27255=CARTESIAN_POINT('Ctrl Pts',(-0.475119387659319,4.05902060671436,
-36.0496484960586));
#27256=CARTESIAN_POINT('Ctrl Pts',(-0.356570587963855,4.06940811615143,
-36.0554744216737));
#27257=CARTESIAN_POINT('Ctrl Pts',(-0.328504018016518,4.07186737141966,
-36.0568537165228));
#27258=CARTESIAN_POINT('Ctrl Pts',(-0.300422154589264,4.07403536270349,
-36.0582330113719));
#27259=CARTESIAN_POINT('Ctrl Pts',(-0.272331500023082,4.07591223581853,
-36.059612306221));
#27260=CARTESIAN_POINT('Ctrl Pts',(-0.150652121165061,4.08404222632104,
-36.0655869530596));
#27261=CARTESIAN_POINT('Ctrl Pts',(-0.0284087048904191,4.08673200763319,
-36.0715615998983));
#27262=CARTESIAN_POINT('Ctrl Pts',(0.0938723505112838,4.08392127517286,
-36.0775362467369));
#27263=CARTESIAN_POINT('Ctrl Pts',(0.212929860204959,4.08118463861012,-36.083353391278));
#27264=CARTESIAN_POINT('Ctrl Pts',(0.332022605367885,4.07323384029929,-36.0891705358191));
#27265=CARTESIAN_POINT('Ctrl Pts',(0.450658698680455,4.06006548436151,-36.0949876803602));
#27266=CARTESIAN_POINT('Ctrl Pts',(0.569186150230049,4.04690918743009,-36.1007994978139));
#27267=CARTESIAN_POINT('Ctrl Pts',(0.687257378507995,4.02854487922045,-36.1066113152676));
#27268=CARTESIAN_POINT('Ctrl Pts',(0.804382026689269,4.00502116787655,-36.1124231327213));
#27269=CARTESIAN_POINT('Ctrl Pts',(0.921427010307248,3.98151345663358,-36.1182309971565));
#27270=CARTESIAN_POINT('Ctrl Pts',(1.03752629592987,3.95285340288052,-36.1240388615917));
#27271=CARTESIAN_POINT('Ctrl Pts',(1.1521968018633,3.91914117247338,-36.1298467260269));
#27272=CARTESIAN_POINT('Ctrl Pts',(1.2725646562154,3.88375396626459,-36.135943151387));
#27273=CARTESIAN_POINT('Ctrl Pts',(1.39135763936013,3.84279971606564,-36.1420395767472));
#27274=CARTESIAN_POINT('Ctrl Pts',(1.50803172254238,3.79645430945848,-36.1481360021073));
#27275=CARTESIAN_POINT('Ctrl Pts',(1.61912987400424,3.75232378053234,-36.1539410752612));
#27276=CARTESIAN_POINT('Ctrl Pts',(1.72830655847884,3.70330564643782,-36.1597461484151));
#27277=CARTESIAN_POINT('Ctrl Pts',(1.8351108847196,3.64960176468387,-36.165551221569));
#27278=CARTESIAN_POINT('Ctrl Pts',(1.94191608605904,3.59589744290847,-36.1713563422866));
#27279=CARTESIAN_POINT('Ctrl Pts',(2.04634852902581,3.5375074861917,-36.1771614630042));
#27280=CARTESIAN_POINT('Ctrl Pts',(2.14798132902517,3.47468001550636,-36.1829665837219));
#27281=CARTESIAN_POINT('Ctrl Pts',(2.24966183811596,3.41182305196494,-36.1887744295148));
#27282=CARTESIAN_POINT('Ctrl Pts',(2.34853973848285,3.34452463795732,-36.1945822753078));
#27283=CARTESIAN_POINT('Ctrl Pts',(2.44421682960853,3.27307639535933,-36.2003901211007));
#27284=CARTESIAN_POINT('Ctrl Pts',(2.45856937424092,3.26235842642101,-36.2012613575167));
#27285=CARTESIAN_POINT('Ctrl Pts',(2.47284994982935,3.25154714875453,-36.2021325939326));
#27286=CARTESIAN_POINT('Ctrl Pts',(2.4870572760686,3.24064362520075,-36.2030038303486));
#27287=CARTESIAN_POINT('Ctrl Pts',(2.48705727606859,3.24064362520075,-34.9531798329663));
#27288=CARTESIAN_POINT('Ctrl Pts',(2.58185257295869,3.16789223376906,-34.9589854944241));
#27289=CARTESIAN_POINT('Ctrl Pts',(2.67349144398005,3.09094849285946,-34.9647911558819));
#27290=CARTESIAN_POINT('Ctrl Pts',(2.76159033964477,3.01012355161391,-34.9705968173397));
#27291=CARTESIAN_POINT('Ctrl Pts',(2.84967960198705,2.92930744830796,-34.9764018439676));
#27292=CARTESIAN_POINT('Ctrl Pts',(2.93422935823234,2.84461126453053,-34.9822068705956));
#27293=CARTESIAN_POINT('Ctrl Pts',(3.0148909053675,2.75638492027735,-34.9880118972235));
#27294=CARTESIAN_POINT('Ctrl Pts',(3.09556263158334,2.66814744230421,-34.9938176564165));
#27295=CARTESIAN_POINT('Ctrl Pts',(3.17234489771808,2.57637921918024,-34.9996234156096));
#27296=CARTESIAN_POINT('Ctrl Pts',(3.24492791543381,2.48146485440322,-35.0054291748026));
#27297=CARTESIAN_POINT('Ctrl Pts',(3.31921376641181,2.38432375198843,-35.0113711399592));
#27298=CARTESIAN_POINT('Ctrl Pts',(3.38910060130646,2.28388740056329,-35.0173131051158));
#27299=CARTESIAN_POINT('Ctrl Pts',(3.45430273132409,2.18060029358132,-35.0232550702724));
#27300=CARTESIAN_POINT('Ctrl Pts',(3.51810542786156,2.07953003803565,-35.029069503016));
#27301=CARTESIAN_POINT('Ctrl Pts',(3.57742233900376,1.97573055458253,-35.0348839357595));
#27302=CARTESIAN_POINT('Ctrl Pts',(3.63203245277187,1.8696430841238,-35.0406983685031));
#27303=CARTESIAN_POINT('Ctrl Pts',(3.68843927480726,1.76006526687625,-35.0467040998662));
#27304=CARTESIAN_POINT('Ctrl Pts',(3.73982405310811,1.64804675411381,-35.0527098312293));
#27305=CARTESIAN_POINT('Ctrl Pts',(3.7859976477236,1.53409478567375,-35.0587155625925));
#27306=CARTESIAN_POINT('Ctrl Pts',(3.83217124233908,1.42014281723368,-35.0647212939556));
#27307=CARTESIAN_POINT('Ctrl Pts',(3.87313355733504,1.3042578606197,-35.0707270253187));
#27308=CARTESIAN_POINT('Ctrl Pts',(3.9087526211886,1.18696164485262,-35.0767327566819));
#27309=CARTESIAN_POINT('Ctrl Pts',(3.94330247076365,1.07318643090717,-35.0825582077953));
#27310=CARTESIAN_POINT('Ctrl Pts',(3.97293584875576,0.957719453854558,-35.0883836589087));
#27311=CARTESIAN_POINT('Ctrl Pts',(3.99748734984815,0.84102311966082,-35.0942091100221));
#27312=CARTESIAN_POINT('Ctrl Pts',(4.02200803469859,0.724473258892695,-35.1000272492196));
#27313=CARTESIAN_POINT('Ctrl Pts',(4.04145944653533,0.60669750594145,-35.1058453884172));
#27314=CARTESIAN_POINT('Ctrl Pts',(4.05572571045719,0.488174109858925,-35.1116635276147));
#27315=CARTESIAN_POINT('Ctrl Pts',(4.06997777891732,0.369768648951444,-35.1174758775479));
#27316=CARTESIAN_POINT('Ctrl Pts',(4.07905491520925,0.250617427705652,-35.1232882274811));
#27317=CARTESIAN_POINT('Ctrl Pts',(4.08289225877019,0.13120900607235,-35.1291005774144));
#27318=CARTESIAN_POINT('Ctrl Pts',(4.08685921410945,0.00776739386600114,
-35.1351092477967));
#27319=CARTESIAN_POINT('Ctrl Pts',(4.08522605676269,-0.115948666280446,
-35.141117918179));
#27320=CARTESIAN_POINT('Ctrl Pts',(4.07797939808869,-0.239393042430706,
-35.1471265885613));
#27321=CARTESIAN_POINT('Ctrl Pts',(4.07097731617103,-0.358671136371906,
-35.1529324646382));
#27322=CARTESIAN_POINT('Ctrl Pts',(4.05873455894428,-0.477695149436253,
-35.1587383407151));
#27323=CARTESIAN_POINT('Ctrl Pts',(4.04129202904109,-0.595972932278733,
-35.1645442167921));
#27324=CARTESIAN_POINT('Ctrl Pts',(4.02385202650952,-0.714233577016134,
-35.1703492516145));
#27325=CARTESIAN_POINT('Ctrl Pts',(4.0012138092065,-0.831747803024423,-35.176154286437));
#27326=CARTESIAN_POINT('Ctrl Pts',(3.97346994912334,-0.948030359964137,
-35.1819593212594));
#27327=CARTESIAN_POINT('Ctrl Pts',(3.94572357420098,-1.06432345732371,-35.1877648822786));
#27328=CARTESIAN_POINT('Ctrl Pts',(3.91287073103484,-1.17938426674482,-35.1935704432978));
#27329=CARTESIAN_POINT('Ctrl Pts',(3.87505458387088,-1.29274010227163,-35.199376004317));
#27330=CARTESIAN_POINT('Ctrl Pts',(3.83722610164495,-1.4061329127777,-35.2051834590235));
#27331=CARTESIAN_POINT('Ctrl Pts',(3.79443122469791,-1.51781925650291,-35.2109909137299));
#27332=CARTESIAN_POINT('Ctrl Pts',(3.74686199638506,-1.62734451793263,-35.2167983684364));
#27333=CARTESIAN_POINT('Ctrl Pts',(3.69924033515195,-1.73699050297933,-35.2226122243778));
#27334=CARTESIAN_POINT('Ctrl Pts',(3.64683398098893,-1.84447027662019,-35.2284260803192));
#27335=CARTESIAN_POINT('Ctrl Pts',(3.58988192869939,-1.94935187639316,-35.2342399362607));
#27336=CARTESIAN_POINT('Ctrl Pts',(3.53289240630361,-2.05430248025867,-35.2400576172759));
#27337=CARTESIAN_POINT('Ctrl Pts',(3.47135143935218,-2.15665115703625,-35.2458752982911));
#27338=CARTESIAN_POINT('Ctrl Pts',(3.40554163728126,-2.25599449395242,-35.2516929793063));
#27339=CARTESIAN_POINT('Ctrl Pts',(3.33963858297056,-2.3554786,-35.2575189039534));
#27340=CARTESIAN_POINT('Ctrl Pts',(3.26945485984531,-2.45194853794407,-35.2633448286005));
#27341=CARTESIAN_POINT('Ctrl Pts',(3.19531370704236,-2.54503346020975,-35.2691707532476));
#27342=CARTESIAN_POINT('Ctrl Pts',(3.17776057548174,-2.56707158377632,-35.2705500576949));
#27343=CARTESIAN_POINT('Ctrl Pts',(3.15998578540621,-2.58892013290523,-35.2719293621423));
#27344=CARTESIAN_POINT('Ctrl Pts',(3.14199392218859,-2.61057449480568,-35.2733086665896));
#27345=CARTESIAN_POINT('Ctrl Pts',(3.06600582348427,-2.70203104766893,-35.2791341178629));
#27346=CARTESIAN_POINT('Ctrl Pts',(2.98589970471296,-2.7903133811064,-35.2849595691361));
#27347=CARTESIAN_POINT('Ctrl Pts',(2.90197064707861,-2.87502893263601,-35.2907850204093));
#27348=CARTESIAN_POINT('Ctrl Pts',(2.81814693444228,-2.95963815198628,-35.2966031597673));
#27349=CARTESIAN_POINT('Ctrl Pts',(2.73051011176688,-3.04068920674115,-35.3024212991253));
#27350=CARTESIAN_POINT('Ctrl Pts',(2.63939574446582,-3.11782217326385,-35.3082394384834));
#27351=CARTESIAN_POINT('Ctrl Pts',(2.54837203932978,-3.19487838963236,-35.3140517885776));
#27352=CARTESIAN_POINT('Ctrl Pts',(2.45387798317224,-3.26802401166205,-35.3198641386717));
#27353=CARTESIAN_POINT('Ctrl Pts',(2.35628582291631,-3.33693603785323,-35.3256764887659));
#27354=CARTESIAN_POINT('Ctrl Pts',(2.25539735138565,-3.40817566380552,-35.3316851590881));
#27355=CARTESIAN_POINT('Ctrl Pts',(2.15119809820872,-3.47489032488061,-35.3376938294102));
#27356=CARTESIAN_POINT('Ctrl Pts',(2.04413670567813,-3.53676831705151,-35.3437024997324));
#27357=CARTESIAN_POINT('Ctrl Pts',(1.94068866117255,-3.59655791194382,-35.3495083759704));
#27358=CARTESIAN_POINT('Ctrl Pts',(1.83456893706537,-3.65183182685612,-35.3553142522085));
#27359=CARTESIAN_POINT('Ctrl Pts',(1.72621097659092,-3.70235339538205,-35.3611201284465));
#27360=CARTESIAN_POINT('Ctrl Pts',(1.61786871687178,-3.75286764347871,-35.3669251634299));
#27361=CARTESIAN_POINT('Ctrl Pts',(1.50728923546747,-3.79863074227898,-35.3727301984132));
#27362=CARTESIAN_POINT('Ctrl Pts',(1.39492864762283,-3.83945296468666,-35.3785352333966));
#27363=CARTESIAN_POINT('Ctrl Pts',(1.28255787487331,-3.88027888741719,-35.3843407945762));
#27364=CARTESIAN_POINT('Ctrl Pts',(1.16840605819321,-3.91616290395843,-35.3901463557559));
#27365=CARTESIAN_POINT('Ctrl Pts',(1.05294666164762,-3.94696444469989,-35.3959519169356));
#27366=CARTESIAN_POINT('Ctrl Pts',(0.937449603985241,-3.9777760324402,-35.4017593718019));
#27367=CARTESIAN_POINT('Ctrl Pts',(0.82064451223023,-4.00350174218263,-35.4075668266683));
#27368=CARTESIAN_POINT('Ctrl Pts',(0.703016659107214,-4.02405176122496,
-35.4133742815346));
#27369=CARTESIAN_POINT('Ctrl Pts',(0.585259151366584,-4.04462443140637,
-35.4191881376343));
#27370=CARTESIAN_POINT('Ctrl Pts',(0.466677474225332,-4.06000995344015,
-35.425001993734));
#27371=CARTESIAN_POINT('Ctrl Pts',(0.347763821923251,-4.07017018368536,
-35.4308158498337));
#27372=CARTESIAN_POINT('Ctrl Pts',(0.228771933525952,-4.08033709858557,
-35.4366335310064));
#27373=CARTESIAN_POINT('Ctrl Pts',(0.109448041697635,-4.08527185822192,
-35.4424512121792));
#27374=CARTESIAN_POINT('Ctrl Pts',(-0.009715497563873,-4.0849884466308,
-35.4482688933519));
#27375=CARTESIAN_POINT('Ctrl Pts',(-0.129047891055146,-4.08470463344665,
-35.4540948181541));
#27376=CARTESIAN_POINT('Ctrl Pts',(-0.248219072395885,-4.07918791013412,
-35.4599207429563));
#27377=CARTESIAN_POINT('Ctrl Pts',(-0.366741519249476,-4.06850410569519,
-35.4657466677586));
#27378=CARTESIAN_POINT('Ctrl Pts',(-0.394802018096425,-4.06597468709054,
-35.4671259706716));
#27379=CARTESIAN_POINT('Ctrl Pts',(-0.422826199933721,-4.06315586969311,
-35.4685052735845));
#27380=CARTESIAN_POINT('Ctrl Pts',(-0.450807689956826,-4.06004894387688,
-35.4698845764975));
#27381=CARTESIAN_POINT('Ctrl Pts',(-0.56898680408474,-4.0469269214142,-35.4757100274021));
#27382=CARTESIAN_POINT('Ctrl Pts',(-0.686781564327053,-4.02861972549075,
-35.4815354783067));
#27383=CARTESIAN_POINT('Ctrl Pts',(-0.803701811597009,-4.00515772448922,
-35.4873609292113));
#27384=CARTESIAN_POINT('Ctrl Pts',(-0.920475304401193,-3.98172517222308,
-35.4931790682007));
#27385=CARTESIAN_POINT('Ctrl Pts',(-1.03637607093199,-3.95315076368354,
-35.4989972071901));
#27386=CARTESIAN_POINT('Ctrl Pts',(-1.1509189273156,-3.91951663126293,-35.5048153461795));
#27387=CARTESIAN_POINT('Ctrl Pts',(-1.26534780932296,-3.88591596604738,
-35.5106276959055));
#27388=CARTESIAN_POINT('Ctrl Pts',(-1.37842107995376,-3.84726570720263,
-35.5164400456315));
#27389=CARTESIAN_POINT('Ctrl Pts',(-1.48966419956015,-3.80369893295314,
-35.5222523953575));
#27390=CARTESIAN_POINT('Ctrl Pts',(-1.6046647205544,-3.75866062627441,-35.5282610658178));
#27391=CARTESIAN_POINT('Ctrl Pts',(-1.7177088345245,-3.70836788741373,-35.5342697362782));
#27392=CARTESIAN_POINT('Ctrl Pts',(-1.82828939612217,-3.65302380009044,
-35.5402784067385));
#27393=CARTESIAN_POINT('Ctrl Pts',(-1.93513782771306,-3.59954759375829,
-35.5460842826118));
#27394=CARTESIAN_POINT('Ctrl Pts',(-2.03968592103842,-3.54135570345619,
-35.551890158485));
#27395=CARTESIAN_POINT('Ctrl Pts',(-2.14149754958436,-3.47867981353906,
-35.5576960343583));
#27396=CARTESIAN_POINT('Ctrl Pts',(-2.24329442595143,-3.41601300515763,
-35.5635010689787));
#27397=CARTESIAN_POINT('Ctrl Pts',(-2.34235527872662,-3.34886370313172,
-35.5693061035992));
#27398=CARTESIAN_POINT('Ctrl Pts',(-2.4382706989037,-3.27750835221936,-35.5751111382196));
#27399=CARTESIAN_POINT('Ctrl Pts',(-2.53419481335538,-3.20614653328534,
-35.5809166990387));
#27400=CARTESIAN_POINT('Ctrl Pts',(-2.62697260094794,-3.13057815098081,
-35.5867222598578));
#27401=CARTESIAN_POINT('Ctrl Pts',(-2.71622615155643,-3.05112118631839,
-35.5925278206769));
#27402=CARTESIAN_POINT('Ctrl Pts',(-2.80550881537117,-2.97163830395315,
-35.5983352751853));
#27403=CARTESIAN_POINT('Ctrl Pts',(-2.89126465137951,-2.88826458779838,
-35.6041427296937));
#27404=CARTESIAN_POINT('Ctrl Pts',(-2.97315163245833,-2.8013558093199,-35.609950184202));
#27405=CARTESIAN_POINT('Ctrl Pts',(-3.05512887307286,-2.7143512360534,-35.6157640399495));
#27406=CARTESIAN_POINT('Ctrl Pts',(-3.13322846680991,-2.62380411998626,
-35.621577895697));
#27407=CARTESIAN_POINT('Ctrl Pts',(-3.2071477204704,-2.53010444430295,-35.6273917514445));
#27408=CARTESIAN_POINT('Ctrl Pts',(-3.28111560739103,-2.43634312134267,
-35.6332094322679));
#27409=CARTESIAN_POINT('Ctrl Pts',(-3.35089743891608,-2.33942543833364,
-35.6390271130913));
#27410=CARTESIAN_POINT('Ctrl Pts',(-3.41623395845745,-2.23977019827529,
-35.6448447939148));
#27411=CARTESIAN_POINT('Ctrl Pts',(-3.48166305965255,-2.13997374703839,
-35.6506707183746));
#27412=CARTESIAN_POINT('Ctrl Pts',(-3.54263406914116,-2.0374323459784,-35.6564966428345));
#27413=CARTESIAN_POINT('Ctrl Pts',(-3.59893367975997,-1.93258929125911,
-35.6623225672943));
#27414=CARTESIAN_POINT('Ctrl Pts',(-3.61226279381032,-1.90776736054981,
-35.6637018736646));
#27415=CARTESIAN_POINT('Ctrl Pts',(-3.62533027957415,-1.88281650320364,
-35.665081180035));
#27416=CARTESIAN_POINT('Ctrl Pts',(-3.63813370655198,-1.85774275217274,
-35.6664604864053));
#27417=CARTESIAN_POINT('Ctrl Pts',(-3.6955115031636,-1.74537622800449,-35.6726417658799));
#27418=CARTESIAN_POINT('Ctrl Pts',(-3.74774736328879,-1.63021694586954,
-35.6788230453544));
#27419=CARTESIAN_POINT('Ctrl Pts',(-3.79457835110188,-1.51274589318529,
-35.685004324829));
#27420=CARTESIAN_POINT('Ctrl Pts',(-3.84217030669429,-1.39336602562715,
-35.6912860453734));
#27421=CARTESIAN_POINT('Ctrl Pts',(-3.88417997960303,-1.27159886783622,
-35.6975677659177));
#27422=CARTESIAN_POINT('Ctrl Pts',(-3.92037933535891,-1.14797685816867,
-35.7038494864621));
#27423=CARTESIAN_POINT('Ctrl Pts',(-3.9558410409636,-1.02687394841927,-35.7100032016314));
#27424=CARTESIAN_POINT('Ctrl Pts',(-3.98572681192188,-0.903991386433874,
-35.7161569168008));
#27425=CARTESIAN_POINT('Ctrl Pts',(-4.00986993742051,-0.779851322350109,
-35.7223106319701));
#27426=CARTESIAN_POINT('Ctrl Pts',(-4.0347663761004,-0.651837843177621,
-35.728656355202));
#27427=CARTESIAN_POINT('Ctrl Pts',(-4.05355578670384,-0.522487414956089,
-35.7350020784338));
#27428=CARTESIAN_POINT('Ctrl Pts',(-4.06611043343708,-0.392391313734325,
-35.7413478016657));
#27429=CARTESIAN_POINT('Ctrl Pts',(-4.07866508017031,-0.262295212512561,
-35.7476935248976));
#27430=CARTESIAN_POINT('Ctrl Pts',(-4.08498484169645,-0.131453816830751,
-35.7540392481294));
#27431=CARTESIAN_POINT('Ctrl Pts',(-4.08499997274305,-0.000471899681166737,
-35.7603849713613));
#27432=CARTESIAN_POINT('Origin',(0.,0.,-25.2396150285955));
#27433=CARTESIAN_POINT('',(2.4870572760686,3.24064362520074,-33.7031235592767));
#27434=CARTESIAN_POINT('',(2.48364276907221,3.23615213332545,-33.8072572988311));
#27435=CARTESIAN_POINT('',(2.4870572760686,3.24064362520075,-25.2396150285955));
#27436=CARTESIAN_POINT('',(-4.08499870649295,0.00325083849409857,-34.6146150643215));
#27437=CARTESIAN_POINT('Ctrl Pts',(2.48364276907218,3.23615213332547,-33.8072572988311));
#27438=CARTESIAN_POINT('Ctrl Pts',(2.93053432606008,2.89620766874513,-33.8345136466862));
#27439=CARTESIAN_POINT('Ctrl Pts',(4.22102243221385,1.44257110886102,-33.9272952978439));
#27440=CARTESIAN_POINT('Ctrl Pts',(4.26353275186578,-2.23312212597346,-34.0856022523043));
#27441=CARTESIAN_POINT('Ctrl Pts',(0.481516845971146,-4.78880856471269,
-34.2821781622121));
#27442=CARTESIAN_POINT('Ctrl Pts',(-3.29963218394254,-3.21756865493895,
-34.4585157543092));
#27443=CARTESIAN_POINT('Ctrl Pts',(-4.07505368127094,-0.928043141231352,
-34.5693280431036));
#27444=CARTESIAN_POINT('Ctrl Pts',(-4.08219506199217,0.0032478726848344,
-34.6146150285955));
#27445=CARTESIAN_POINT('Ctrl Pts',(-4.08499870649295,0.00325083849409857,
-34.6146150643215));
#27446=CARTESIAN_POINT('Ctrl Pts',(-4.0848857285227,0.145218784049321,-34.6215140152461));
#27447=CARTESIAN_POINT('Ctrl Pts',(-4.07736808054459,0.286878155519986,
-34.6284129661707));
#27448=CARTESIAN_POINT('Ctrl Pts',(-4.06256514836033,0.427538788097697,
-34.6353119170953));
#27449=CARTESIAN_POINT('Ctrl Pts',(-4.04759363057255,0.569801357193021,
-34.6422894378459));
#27450=CARTESIAN_POINT('Ctrl Pts',(-4.02517001513738,0.711042259284884,
-34.6492669585965));
#27451=CARTESIAN_POINT('Ctrl Pts',(-3.9954672708171,0.850568214683206,-34.6562444793471));
#27452=CARTESIAN_POINT('Ctrl Pts',(-3.968385454481,0.977782597888755,-34.662606313574));
#27453=CARTESIAN_POINT('Ctrl Pts',(-3.93525307540227,1.10357157241974,-34.6689681478009));
#27454=CARTESIAN_POINT('Ctrl Pts',(-3.89623577907751,1.22742484651251,-34.6753299820277));
#27455=CARTESIAN_POINT('Ctrl Pts',(-3.86050813447011,1.34083572263829,-34.6811554331409));
#27456=CARTESIAN_POINT('Ctrl Pts',(-3.81976751612471,1.45286679822255,-34.6869808842541));
#27457=CARTESIAN_POINT('Ctrl Pts',(-3.7741385054851,1.56304303888752,-34.6928063353673));
#27458=CARTESIAN_POINT('Ctrl Pts',(-3.72856676688873,1.67308098993515,-34.6986244745646));
#27459=CARTESIAN_POINT('Ctrl Pts',(-3.67811899487606,1.78126836305931,-34.7044426137619));
#27460=CARTESIAN_POINT('Ctrl Pts',(-3.62296959571413,1.88714501523625,-34.7102607529592));
#27461=CARTESIAN_POINT('Ctrl Pts',(-3.5678750722497,1.99291631621757,-34.7160731028923));
#27462=CARTESIAN_POINT('Ctrl Pts',(-3.50808841614009,2.09638111060591,-34.7218854528253));
#27463=CARTESIAN_POINT('Ctrl Pts',(-3.44383195947611,2.19709955051903,-34.7276978027583));
#27464=CARTESIAN_POINT('Ctrl Pts',(-3.37740514889466,2.30121990009191,-34.7337064731407));
#27465=CARTESIAN_POINT('Ctrl Pts',(-3.30620141507986,2.40240467677481,-34.7397151435231));
#27466=CARTESIAN_POINT('Ctrl Pts',(-3.23051807941002,2.50019558007068,-34.7457238139055));
#27467=CARTESIAN_POINT('Ctrl Pts',(-3.15738907748324,2.59468601303393,-34.7515296899822));
#27468=CARTESIAN_POINT('Ctrl Pts',(-3.08007823973709,2.68600761593496,-34.7573355660589));
#27469=CARTESIAN_POINT('Ctrl Pts',(-2.99889721484469,2.77377729726032,-34.7631414421356));
#27470=CARTESIAN_POINT('Ctrl Pts',(-2.91772795284556,2.86153426101534,-34.7689464769578));
#27471=CARTESIAN_POINT('Ctrl Pts',(-2.83268989593037,2.94574002727901,-34.7747515117801));
#27472=CARTESIAN_POINT('Ctrl Pts',(-2.74413344169413,3.02604637343448,-34.7805565466023));
#27473=CARTESIAN_POINT('Ctrl Pts',(-2.65556896026765,3.10635999895002,-34.7863621076213));
#27474=CARTESIAN_POINT('Ctrl Pts',(-2.56348574968054,3.18277322748858,-34.7921676686403));
#27475=CARTESIAN_POINT('Ctrl Pts',(-2.46826886854475,3.25497677296979,-34.7979732296592));
#27476=CARTESIAN_POINT('Ctrl Pts',(-2.37302092908558,3.32720387016827,-34.8037806843654));
#27477=CARTESIAN_POINT('Ctrl Pts',(-2.27463761115528,3.39521830701507,-34.8095881390717));
#27478=CARTESIAN_POINT('Ctrl Pts',(-2.17353411149157,3.45875331097529,-34.8153955937779));
#27479=CARTESIAN_POINT('Ctrl Pts',(-2.07231917105122,3.52235834604432,-34.8212094497191));
#27480=CARTESIAN_POINT('Ctrl Pts',(-1.96837840977851,3.58147387567573,-34.8270233056603));
#27481=CARTESIAN_POINT('Ctrl Pts',(-1.8621529840195,3.63587833461287,-34.8328371616016));
#27482=CARTESIAN_POINT('Ctrl Pts',(-1.75585767003262,3.69031858753432,-34.8386548426166));
#27483=CARTESIAN_POINT('Ctrl Pts',(-1.64727506808491,3.74004142740467,-34.8444725236316));
#27484=CARTESIAN_POINT('Ctrl Pts',(-1.53686621063264,3.78487347881216,-34.8502902046465));
#27485=CARTESIAN_POINT('Ctrl Pts',(-1.42630090424893,3.82976905706613,-34.8561161292934));
#27486=CARTESIAN_POINT('Ctrl Pts',(-1.31390456045862,3.86975987876471,-34.8619420539403));
#27487=CARTESIAN_POINT('Ctrl Pts',(-1.20015335692215,3.9047223870422,-34.8677679785872));
#27488=CARTESIAN_POINT('Ctrl Pts',(-1.17322243167338,3.91299986163286,-34.8691472830367));
#27489=CARTESIAN_POINT('Ctrl Pts',(-1.14621560689718,3.92099571550889,-34.8705265874861));
#27490=CARTESIAN_POINT('Ctrl Pts',(-1.11913927164857,3.92870873069688,-34.8719058919356));
#27491=CARTESIAN_POINT('Ctrl Pts',(-1.00477888093834,3.9612856441659,-34.8777315620014));
#27492=CARTESIAN_POINT('Ctrl Pts',(-0.888811943804751,3.98891717273778,
-34.8835572320672));
#27493=CARTESIAN_POINT('Ctrl Pts',(-0.771703712261843,4.01144592142052,
-34.889382902133));
#27494=CARTESIAN_POINT('Ctrl Pts',(-0.654743540980267,4.03394618694393,
-34.895201206788));
#27495=CARTESIAN_POINT('Ctrl Pts',(-0.536645342689016,4.05135642868629,
-34.901019511443));
#27496=CARTESIAN_POINT('Ctrl Pts',(-0.417889341804417,4.06356905909156,
-34.906837816098));
#27497=CARTESIAN_POINT('Ctrl Pts',(-0.299252591448985,4.07576942601013,
-34.9126502782196));
#27498=CARTESIAN_POINT('Ctrl Pts',(-0.179959756285397,4.08278252384552,
-34.9184627403411));
#27499=CARTESIAN_POINT('Ctrl Pts',(-0.060500474495871,4.084551957386,-34.9242752024627));
#27500=CARTESIAN_POINT('Ctrl Pts',(0.0588684033324125,4.08632005186098,
-34.9300832658503));
#27501=CARTESIAN_POINT('Ctrl Pts',(0.178403070480959,4.08285237366982,-34.9358913292378));
#27502=CARTESIAN_POINT('Ctrl Pts',(0.297610172620584,4.07414447278846,-34.9416993926254));
#27503=CARTESIAN_POINT('Ctrl Pts',(0.416769399934111,4.06544006909169,-34.9475051234337));
#27504=CARTESIAN_POINT('Ctrl Pts',(0.535600917600651,4.05149965774601,-34.9533108542419));
#27505=CARTESIAN_POINT('Ctrl Pts',(0.65361324170988,4.03237085723294,-34.9591165850501));
#27506=CARTESIAN_POINT('Ctrl Pts',(0.771605967742213,4.01324523340252,-34.964921351712));
#27507=CARTESIAN_POINT('Ctrl Pts',(0.888779368345493,3.98893300005499,-34.9707261183738));
#27508=CARTESIAN_POINT('Ctrl Pts',(1.00464957269879,3.959533335644,-34.9765308850356));
#27509=CARTESIAN_POINT('Ctrl Pts',(1.12052782646279,3.93013162886177,-34.9823360549499));
#27510=CARTESIAN_POINT('Ctrl Pts',(1.23510230882257,3.89564188957588,-34.9881412248643));
#27511=CARTESIAN_POINT('Ctrl Pts',(1.34790241018648,3.85621369903348,-34.9939463947786));
#27512=CARTESIAN_POINT('Ctrl Pts',(1.46079370495804,3.81675363271252,-34.9997562578911));
#27513=CARTESIAN_POINT('Ctrl Pts',(1.57190736800501,3.77234727584653,-35.0055661210036));
#27514=CARTESIAN_POINT('Ctrl Pts',(1.68079085356918,3.72319313312621,-35.011375984116));
#27515=CARTESIAN_POINT('Ctrl Pts',(1.78972161361045,3.6740176489106,-35.0171883697253));
#27516=CARTESIAN_POINT('Ctrl Pts',(1.89641990205823,3.62009045420047,-35.0230007553346));
#27517=CARTESIAN_POINT('Ctrl Pts',(2.00045733956525,3.56165627659092,-35.0288131409438));
#27518=CARTESIAN_POINT('Ctrl Pts',(2.10463072800272,3.50314574011473,-35.0346331218884));
#27519=CARTESIAN_POINT('Ctrl Pts',(2.20613597300339,3.44011667098013,-35.0404531028331));
#27520=CARTESIAN_POINT('Ctrl Pts',(2.30457302903138,3.37285756501236,-35.0462730837777));
#27521=CARTESIAN_POINT('Ctrl Pts',(2.36665186513484,3.33044094687771,-35.0499434255958));
#27522=CARTESIAN_POINT('Ctrl Pts',(2.42751106117837,3.28634283317704,-35.0536137674139));
#27523=CARTESIAN_POINT('Ctrl Pts',(2.4870572760686,3.24064362520074,-35.057284109232));
#27524=CARTESIAN_POINT('',(-4.08499921798789,-0.00252765470411389,-34.5103849714454));
#27525=CARTESIAN_POINT('Ctrl Pts',(-4.08499921798789,-0.00252765470410572,
-34.5103849714454));
#27526=CARTESIAN_POINT('Ctrl Pts',(-4.08507189103842,0.114920885278749,
-34.5161279682783));
#27527=CARTESIAN_POINT('Ctrl Pts',(-4.0800751941379,0.232562318317247,-34.5218709651111));
#27528=CARTESIAN_POINT('Ctrl Pts',(-4.0699856738512,0.349916582410724,-34.527613961944));
#27529=CARTESIAN_POINT('Ctrl Pts',(-4.05990723653758,0.467141937089886,
-34.5333506503025));
#27530=CARTESIAN_POINT('Ctrl Pts',(-4.04474713355492,0.584080334458861,
-34.5390873386611));
#27531=CARTESIAN_POINT('Ctrl Pts',(-4.02453394165429,0.700251063885355,
-34.5448240270196));
#27532=CARTESIAN_POINT('Ctrl Pts',(-4.00416272258904,0.817330018547843,
-34.5506055649299));
#27533=CARTESIAN_POINT('Ctrl Pts',(-3.97865904795262,0.933628817439481,
-34.5563871028402));
#27534=CARTESIAN_POINT('Ctrl Pts',(-3.94810563132553,1.04865958437217,-34.5621686407504));
#27535=CARTESIAN_POINT('Ctrl Pts',(-3.91782816729369,1.1626514154943,-34.5678979609199));
#27536=CARTESIAN_POINT('Ctrl Pts',(-3.88259192065302,1.27539761376406,-34.5736272810893));
#27537=CARTESIAN_POINT('Ctrl Pts',(-3.84252864447435,1.38643377641851,-34.5793566012588));
#27538=CARTESIAN_POINT('Ctrl Pts',(-3.80247324529,1.49744810782735,-34.5850847949646));
#27539=CARTESIAN_POINT('Ctrl Pts',(-3.75759284556215,1.60675267684264,-34.5908129886704));
#27540=CARTESIAN_POINT('Ctrl Pts',(-3.70806856918763,1.71389978884496,-34.5965411823763));
#27541=CARTESIAN_POINT('Ctrl Pts',(-3.65854159187046,1.82105274440979,-34.6022696884849));
#27542=CARTESIAN_POINT('Ctrl Pts',(-3.60437041159065,1.92604762802633,-34.6079981945936));
#27543=CARTESIAN_POINT('Ctrl Pts',(-3.5457833064289,2.02845895789146,-34.6137267007022));
#27544=CARTESIAN_POINT('Ctrl Pts',(-3.48624833339938,2.13252717810146,-34.6195478870492));
#27545=CARTESIAN_POINT('Ctrl Pts',(-3.42215350945476,2.233927120391,-34.6253690733962));
#27546=CARTESIAN_POINT('Ctrl Pts',(-3.35378495433835,2.33224172847792,-34.6311902597432));
#27547=CARTESIAN_POINT('Ctrl Pts',(-3.28641177720436,2.42912497391467,-34.6369266954221));
#27548=CARTESIAN_POINT('Ctrl Pts',(-3.2148887863614,2.52301182450451,-34.6426631311011));
#27549=CARTESIAN_POINT('Ctrl Pts',(-3.13953055420171,2.61353647367583,-34.64839956678));
#27550=CARTESIAN_POINT('Ctrl Pts',(-3.06250229707934,2.70606725302725,-34.654263128461));
#27551=CARTESIAN_POINT('Ctrl Pts',(-2.98146712601755,2.79508471007264,-34.6601266901421));
#27552=CARTESIAN_POINT('Ctrl Pts',(-2.89679987682826,2.88023878760213,-34.6659902518231));
#27553=CARTESIAN_POINT('Ctrl Pts',(-2.81213262763897,2.96539286513162,-34.6718538135041));
#27554=CARTESIAN_POINT('Ctrl Pts',(-2.72383368600946,3.04668330119613,-34.6777173751852));
#27555=CARTESIAN_POINT('Ctrl Pts',(-2.63231171170454,3.123805380049,-34.6835809368662));
#27556=CARTESIAN_POINT('Ctrl Pts',(-2.54138458930515,3.20042619987734,-34.6894063880184));
#27557=CARTESIAN_POINT('Ctrl Pts',(-2.44696383970992,3.27319626328287,-34.6952318391706));
#27558=CARTESIAN_POINT('Ctrl Pts',(-2.34940915475552,3.3417812052184,-34.7010572903228));
#27559=CARTESIAN_POINT('Ctrl Pts',(-2.25197691724743,3.4102800615805,-34.7068754295595));
#27560=CARTESIAN_POINT('Ctrl Pts',(-2.15141889928821,3.47460401221233,-34.7126935687962));
#27561=CARTESIAN_POINT('Ctrl Pts',(-2.04812888576518,3.53445795947473,-34.7185117080329));
#27562=CARTESIAN_POINT('Ctrl Pts',(-1.94494164963081,3.594252349843,-34.7243240580055));
#27563=CARTESIAN_POINT('Ctrl Pts',(-1.83902817706856,3.64958538199854,-34.7301364079782));
#27564=CARTESIAN_POINT('Ctrl Pts',(-1.7308118474824,3.70020477117342,-34.7359487579509));
#27565=CARTESIAN_POINT('Ctrl Pts',(-1.61894035730438,3.752533902281,-34.7419574283185));
#27566=CARTESIAN_POINT('Ctrl Pts',(-1.50460805523535,3.7998250786186,-34.7479660986861));
#27567=CARTESIAN_POINT('Ctrl Pts',(-1.3883115259683,3.84185060964941,-34.7539747690538));
#27568=CARTESIAN_POINT('Ctrl Pts',(-1.27594003603281,3.8824577676362,-34.7597806451706));
#27569=CARTESIAN_POINT('Ctrl Pts',(-1.16173518016177,3.91814882911819,-34.7655865212874));
#27570=CARTESIAN_POINT('Ctrl Pts',(-1.04616534780103,3.94876728423699,-34.7713923974042));
#27571=CARTESIAN_POINT('Ctrl Pts',(-0.930612261169279,3.97938130283164,
-34.7771974322667));
#27572=CARTESIAN_POINT('Ctrl Pts',(-0.813694985692373,4.00492407234662,
-34.7830024671291));
#27573=CARTESIAN_POINT('Ctrl Pts',(-0.695895948715241,4.02528928507775,
-34.7888075019916));
#27574=CARTESIAN_POINT('Ctrl Pts',(-0.578086233855809,4.04565634381161,
-34.7946130630509));
#27575=CARTESIAN_POINT('Ctrl Pts',(-0.459395000651461,4.06084484313215,
-34.8004186241101));
#27576=CARTESIAN_POINT('Ctrl Pts',(-0.340313083382252,4.07079992203975,
-34.8062241851694));
#27577=CARTESIAN_POINT('Ctrl Pts',(-0.221192323371624,4.08075824814529,
-34.8120316399159));
#27578=CARTESIAN_POINT('Ctrl Pts',(-0.101681032236312,4.08547972485986,
-34.8178390946624));
#27579=CARTESIAN_POINT('Ctrl Pts',(0.0177272842119958,4.08496153511811,
-34.8236465494089));
#27580=CARTESIAN_POINT('Ctrl Pts',(0.137267217815624,4.08444277420458,-34.8294604053903));
#27581=CARTESIAN_POINT('Ctrl Pts',(0.256703541938331,4.07867282065794,-34.8352742613716));
#27582=CARTESIAN_POINT('Ctrl Pts',(0.375545050646511,4.06770093725373,-34.8410881173529));
#27583=CARTESIAN_POINT('Ctrl Pts',(0.494464748001043,4.05672183518729,-34.846905798408));
#27584=CARTESIAN_POINT('Ctrl Pts',(0.612788447254424,4.0405340423935,-34.852723479463));
#27585=CARTESIAN_POINT('Ctrl Pts',(0.730033977028201,4.01923816069468,-34.858541160518));
#27586=CARTESIAN_POINT('Ctrl Pts',(0.84744564326344,3.997912102814,-34.8643670852046));
#27587=CARTESIAN_POINT('Ctrl Pts',(0.963775694404563,3.9714635997781,-34.8701930098911));
#27588=CARTESIAN_POINT('Ctrl Pts',(1.07855586087678,3.94004343313222,-34.8760189345777));
#27589=CARTESIAN_POINT('Ctrl Pts',(1.10573038831509,3.93260462025298,-34.8773982386431));
#27590=CARTESIAN_POINT('Ctrl Pts',(1.13281812654346,3.92488735000989,-34.8787775427086));
#27591=CARTESIAN_POINT('Ctrl Pts',(1.15981302825806,3.9168940168816,-34.880156846774));
#27592=CARTESIAN_POINT('Ctrl Pts',(1.27890982403516,3.88162882594951,-34.8862420956234));
#27593=CARTESIAN_POINT('Ctrl Pts',(1.39659581265874,3.84086790255425,-34.8923273444727));
#27594=CARTESIAN_POINT('Ctrl Pts',(1.51232740443447,3.79474515900561,-34.8984125933221));
#27595=CARTESIAN_POINT('Ctrl Pts',(1.62296374346671,3.75065303675922,-34.9042299301829));
#27596=CARTESIAN_POINT('Ctrl Pts',(1.73181365772583,3.70166130574987,-34.9100472670436));
#27597=CARTESIAN_POINT('Ctrl Pts',(1.83841493028788,3.64793853348636,-34.9158646039044));
#27598=CARTESIAN_POINT('Ctrl Pts',(1.94492283349963,3.5942628156362,-34.9216768455074));
#27599=CARTESIAN_POINT('Ctrl Pts',(2.04918564850979,3.53586447764656,-34.9274890871104));
#27600=CARTESIAN_POINT('Ctrl Pts',(2.15076070959423,3.47296031795149,-34.9333013287134));
#27601=CARTESIAN_POINT('Ctrl Pts',(2.25225919348319,3.41010358155189,-34.9391091884814));
#27602=CARTESIAN_POINT('Ctrl Pts',(2.35107361069731,3.34274799860495,-34.9449170482494));
#27603=CARTESIAN_POINT('Ctrl Pts',(2.44678622254801,3.27115609244641,-34.9507249080173));
#27604=CARTESIAN_POINT('Ctrl Pts',(2.46027181438137,3.2610690286169,-34.9515432163337));
#27605=CARTESIAN_POINT('Ctrl Pts',(2.47369587352053,3.25089793800677,-34.95236152465));
#27606=CARTESIAN_POINT('Ctrl Pts',(2.48705727606859,3.24064362520075,-34.9531798329663));
#27607=CARTESIAN_POINT('Ctrl Pts',(2.4870572760686,3.24064362520074,-33.7031235592767));
#27608=CARTESIAN_POINT('Ctrl Pts',(2.58140861963151,3.16823294921954,-33.7089479065311));
#27609=CARTESIAN_POINT('Ctrl Pts',(2.6727421027167,3.09158538855808,-33.7147722537854));
#27610=CARTESIAN_POINT('Ctrl Pts',(2.76065463340963,3.01098173276324,-33.7205966010398));
#27611=CARTESIAN_POINT('Ctrl Pts',(2.84845998739043,2.93047634321948,-33.7264138476637));
#27612=CARTESIAN_POINT('Ctrl Pts',(2.93285238629096,2.84602472527932,-33.7322310942876));
#27613=CARTESIAN_POINT('Ctrl Pts',(3.01345992186858,2.75794929237139,-33.7380483409115));
#27614=CARTESIAN_POINT('Ctrl Pts',(3.09399015369909,2.6699583250279,-33.7438600087151));
#27615=CARTESIAN_POINT('Ctrl Pts',(3.1707424694783,2.57835075612183,-33.7496716765187));
#27616=CARTESIAN_POINT('Ctrl Pts',(3.24338055930375,2.48348697349724,-33.7554833443222));
#27617=CARTESIAN_POINT('Ctrl Pts',(3.31722369002888,2.38704943338212,-33.7613914256936));
#27618=CARTESIAN_POINT('Ctrl Pts',(3.38681454731882,2.28724696092719,-33.7672995070649));
#27619=CARTESIAN_POINT('Ctrl Pts',(3.45184110457183,2.18449490472931,-33.7732075884363));
#27620=CARTESIAN_POINT('Ctrl Pts',(3.51574082737825,2.08352342190441,-33.7790132896436));
#27621=CARTESIAN_POINT('Ctrl Pts',(3.5752329498575,1.97970412336723,-33.7848189908508));
#27622=CARTESIAN_POINT('Ctrl Pts',(3.63006449254069,1.87346117653803,-33.7906246920581));
#27623=CARTESIAN_POINT('Ctrl Pts',(3.68488965641702,1.76723058944204,-33.7964297178613));
#27624=CARTESIAN_POINT('Ctrl Pts',(3.73505513173854,1.65857727733264,-33.8022347436645));
#27625=CARTESIAN_POINT('Ctrl Pts',(3.78035399916738,1.54794981862435,-33.8080397694677));
#27626=CARTESIAN_POINT('Ctrl Pts',(3.82565826654194,1.43730917233973,-33.813845487271));
#27627=CARTESIAN_POINT('Ctrl Pts',(3.86609461788279,1.32469428912235,-33.8196512050744));
#27628=CARTESIAN_POINT('Ctrl Pts',(3.90150460760563,1.21057292090646,-33.8254569228778));
#27629=CARTESIAN_POINT('Ctrl Pts',(3.93800825802992,1.09292683956332,-33.8314419540742));
#27630=CARTESIAN_POINT('Ctrl Pts',(3.96916987962091,0.973680146299653,-33.8374269852706));
#27631=CARTESIAN_POINT('Ctrl Pts',(3.99487195022529,0.85335988967327,-33.8434120164671));
#27632=CARTESIAN_POINT('Ctrl Pts',(4.01984107880477,0.736470787442399,-33.8492263734423));
#27633=CARTESIAN_POINT('Ctrl Pts',(4.0396578047206,0.618568938570236,-33.8550407304175));
#27634=CARTESIAN_POINT('Ctrl Pts',(4.0542669145193,0.500144764877267,-33.8608550873927));
#27635=CARTESIAN_POINT('Ctrl Pts',(4.06951927647338,0.376506269023205,-33.8669254556997));
#27636=CARTESIAN_POINT('Ctrl Pts',(4.07909491797284,0.252298906764303,-33.8729958240067));
#27637=CARTESIAN_POINT('Ctrl Pts',(4.08299155861645,0.128081740567421,-33.8790661923138));
#27638=CARTESIAN_POINT('Ctrl Pts',(4.08688819926007,0.00386457437053903,
-33.8851365606208));
#27639=CARTESIAN_POINT('Ctrl Pts',(4.08510591468131,-0.120361897969216,
-33.8912069289278));
#27640=CARTESIAN_POINT('Ctrl Pts',(4.07770364345426,-0.244045069935603,
-33.8972772972349));
#27641=CARTESIAN_POINT('Ctrl Pts',(4.0706000268172,-0.362738077953689,-33.9031027483669));
#27642=CARTESIAN_POINT('Ctrl Pts',(4.05829840808877,-0.481310545933248,
-33.9089281994989));
#27643=CARTESIAN_POINT('Ctrl Pts',(4.04080422479748,-0.59927140500681,-33.9147536506308));
#27644=CARTESIAN_POINT('Ctrl Pts',(4.02333199963246,-0.717084203471046,
-33.9205717898473));
#27645=CARTESIAN_POINT('Ctrl Pts',(4.0006802327364,-0.834286519845738,-33.9263899290637));
#27646=CARTESIAN_POINT('Ctrl Pts',(3.97290631151279,-0.950389625333658,
-33.9322080682801));
#27647=CARTESIAN_POINT('Ctrl Pts',(3.94516002636953,-1.06637720393122,-33.9380204182324));
#27648=CARTESIAN_POINT('Ctrl Pts',(3.91230182081931,-1.18126735300376,-33.9438327681848));
#27649=CARTESIAN_POINT('Ctrl Pts',(3.8744405029074,-1.29457938707159,-33.9496451181372));
#27650=CARTESIAN_POINT('Ctrl Pts',(3.83530036489639,-1.41171869696148,-33.9556537885124));
#27651=CARTESIAN_POINT('Ctrl Pts',(3.79081322265837,-1.52717095930536,-33.9616624588877));
#27652=CARTESIAN_POINT('Ctrl Pts',(3.74115614356725,-1.64041936999324,-33.9676711292629));
#27653=CARTESIAN_POINT('Ctrl Pts',(3.69317500455989,-1.74984561565717,-33.9734770053595));
#27654=CARTESIAN_POINT('Ctrl Pts',(3.6403674480488,-1.85721396695235,-33.9792828814561));
#27655=CARTESIAN_POINT('Ctrl Pts',(3.58294271170609,-1.96207709446703,-33.9850887575528));
#27656=CARTESIAN_POINT('Ctrl Pts',(3.52552629603823,-2.06692502762399,-33.9908937923951));
#27657=CARTESIAN_POINT('Ctrl Pts',(3.46349422697335,-2.16926810114257,-33.9966988272374));
#27658=CARTESIAN_POINT('Ctrl Pts',(3.39710180162501,-2.26868339558346,-34.0025038620797));
#27659=CARTESIAN_POINT('Ctrl Pts',(3.33070335814077,-2.36810770151549,-34.0083094231189));
#27660=CARTESIAN_POINT('Ctrl Pts',(3.25994399914227,-2.46460336139142,-34.0141149841581));
#27661=CARTESIAN_POINT('Ctrl Pts',(3.18512210400834,-2.5577768046797,-34.0199205451973));
#27662=CARTESIAN_POINT('Ctrl Pts',(3.11027580308902,-2.65098063975445,-34.0257279999239));
#27663=CARTESIAN_POINT('Ctrl Pts',(3.03136458594073,-2.74085978509838,-34.0315354546505));
#27664=CARTESIAN_POINT('Ctrl Pts',(2.94872639587784,-2.82705458777387,-34.037342909377));
#27665=CARTESIAN_POINT('Ctrl Pts',(2.86599711832371,-2.91334439819732,-34.0431567653387));
#27666=CARTESIAN_POINT('Ctrl Pts',(2.77953295055453,-2.99594146523343,-34.0489706213003));
#27667=CARTESIAN_POINT('Ctrl Pts',(2.68970800095107,-3.07452368174646,-34.054784477262));
#27668=CARTESIAN_POINT('Ctrl Pts',(2.59982395338143,-3.15315759936475,-34.0606021582975));
#27669=CARTESIAN_POINT('Ctrl Pts',(2.50657503821053,-3.22777115151494,-34.0664198393329));
#27670=CARTESIAN_POINT('Ctrl Pts',(2.41036635228617,-3.29808414807243,-34.0722375203684));
#27671=CARTESIAN_POINT('Ctrl Pts',(2.31402133902063,-3.368496777878,-34.0780634450357));
#27672=CARTESIAN_POINT('Ctrl Pts',(2.21470852277989,-3.43459646429006,-34.0838893697031));
#27673=CARTESIAN_POINT('Ctrl Pts',(2.11285979541865,-3.49614766348669,-34.0897152943704));
#27674=CARTESIAN_POINT('Ctrl Pts',(2.08874681914687,-3.51072008519663,-34.0910945986278));
#27675=CARTESIAN_POINT('Ctrl Pts',(2.06449179678867,-3.5250377642382,-34.0924739028853));
#27676=CARTESIAN_POINT('Ctrl Pts',(2.04010063005674,-3.5390979668896,-34.0938532071427));
#27677=CARTESIAN_POINT('Ctrl Pts',(1.93708525171181,-3.59848082100475,-34.0996786582781));
#27678=CARTESIAN_POINT('Ctrl Pts',(1.83131017195687,-3.65345711139818,-34.1055041094136));
#27679=CARTESIAN_POINT('Ctrl Pts',(1.72318841613334,-3.70376115354431,-34.111329560549));
#27680=CARTESIAN_POINT('Ctrl Pts',(1.61520237119852,-3.75400205570337,-34.1171476997689));
#27681=CARTESIAN_POINT('Ctrl Pts',(1.50487587551227,-3.79958220349568,-34.1229658389887));
#27682=CARTESIAN_POINT('Ctrl Pts',(1.39264858741361,-3.84028057724626,-34.1287839782086));
#27683=CARTESIAN_POINT('Ctrl Pts',(1.28053296962322,-3.8809384546076,-34.1345963281644));
#27684=CARTESIAN_POINT('Ctrl Pts',(1.16652070352613,-3.91672408330216,-34.1404086781203));
#27685=CARTESIAN_POINT('Ctrl Pts',(1.05107302712988,-3.94746380498163,-34.1462210280761));
#27686=CARTESIAN_POINT('Ctrl Pts',(0.931725940637991,-3.97924180464811,
-34.15222969845));
#27687=CARTESIAN_POINT('Ctrl Pts',(0.81084516407094,-4.00562681086514,-34.158238368824));
#27688=CARTESIAN_POINT('Ctrl Pts',(0.68895965546336,-4.0264822852142,-34.1642470391979));
#27689=CARTESIAN_POINT('Ctrl Pts',(0.571187816215797,-4.0466338815814,-34.170052915298));
#27690=CARTESIAN_POINT('Ctrl Pts',(0.452478404756792,-4.06162309540167,
-34.1758587913981));
#27691=CARTESIAN_POINT('Ctrl Pts',(0.333320071698919,-4.07137848029419,
-34.1816646674982));
#27692=CARTESIAN_POINT('Ctrl Pts',(0.214179004332095,-4.0811324516602,-34.1874697023439));
#27693=CARTESIAN_POINT('Ctrl Pts',(0.0945895512791576,-4.08565406902207,
-34.1932747371897));
#27694=CARTESIAN_POINT('Ctrl Pts',(-0.0249546731795135,-4.08492377704732,
-34.1990797720354));
#27695=CARTESIAN_POINT('Ctrl Pts',(-0.144509733714166,-4.08419341887531,
-34.204885333078));
#27696=CARTESIAN_POINT('Ctrl Pts',(-0.264019149476858,-4.07821020733982,
-34.2106908941207));
#27697=CARTESIAN_POINT('Ctrl Pts',(-0.382990104713468,-4.06700671006227,
-34.2164964551633));
#27698=CARTESIAN_POINT('Ctrl Pts',(-0.501999866499577,-4.05579955837118,
-34.2223039098933));
#27699=CARTESIAN_POINT('Ctrl Pts',(-0.620470412446873,-4.03936877268701,
-34.2281113646233));
#27700=CARTESIAN_POINT('Ctrl Pts',(-0.737915476155763,-4.01779861989745,
-34.2339188193533));
#27701=CARTESIAN_POINT('Ctrl Pts',(-0.855489993040401,-3.99620469152556,
-34.2397326753183));
#27702=CARTESIAN_POINT('Ctrl Pts',(-0.972036369967927,-3.96946016251569,
-34.2455465312833));
#27703=CARTESIAN_POINT('Ctrl Pts',(-1.08707978970347,-3.93770015755622,
-34.2513603872483));
#27704=CARTESIAN_POINT('Ctrl Pts',(-1.20219889923479,-3.90591925693584,
-34.2571780682872));
#27705=CARTESIAN_POINT('Ctrl Pts',(-1.31581269501042,-3.86911643407099,
-34.262995749326));
#27706=CARTESIAN_POINT('Ctrl Pts',(-1.4274643074096,-3.82747575447208,-34.2688134303648));
#27707=CARTESIAN_POINT('Ctrl Pts',(-1.5392741297167,-3.78577607018938,-34.2746393550354));
#27708=CARTESIAN_POINT('Ctrl Pts',(-1.64911584502968,-3.73922500567654,
-34.280465279706));
#27709=CARTESIAN_POINT('Ctrl Pts',(-1.75655511782045,-3.68805356767751,
-34.2862912043767));
#27710=CARTESIAN_POINT('Ctrl Pts',(-1.78199167102502,-3.67593858428822,
-34.2876705086013));
#27711=CARTESIAN_POINT('Ctrl Pts',(-1.80729368388432,-3.66356481564983,
-34.2890498128259));
#27712=CARTESIAN_POINT('Ctrl Pts',(-1.83245562620588,-3.65093568527116,
-34.2904291170505));
#27713=CARTESIAN_POINT('Ctrl Pts',(-1.93872635511457,-3.59759692176587,
-34.2962545681808));
#27714=CARTESIAN_POINT('Ctrl Pts',(-2.04283629197228,-3.53952902162373,
-34.302080019311));
#27715=CARTESIAN_POINT('Ctrl Pts',(-2.14433631617764,-3.47693065261902,
-34.3079054704413));
#27716=CARTESIAN_POINT('Ctrl Pts',(-2.24570894087504,-3.41441085503803,
-34.313723609656));
#27717=CARTESIAN_POINT('Ctrl Pts',(-2.3444778244325,-3.34737211145425,-34.3195417488707));
#27718=CARTESIAN_POINT('Ctrl Pts',(-2.44021648497874,-3.27605990580728,
-34.3253598880854));
#27719=CARTESIAN_POINT('Ctrl Pts',(-2.53585988201199,-3.20481865844602,
-34.3311722380361));
#27720=CARTESIAN_POINT('Ctrl Pts',(-2.62847872912805,-3.12931265088252,
-34.3369845879868));
#27721=CARTESIAN_POINT('Ctrl Pts',(-2.71767421543167,-3.04983144760131,
-34.3427969379375));
#27722=CARTESIAN_POINT('Ctrl Pts',(-2.8098824067416,-2.96766565310414,-34.3488056083133));
#27723=CARTESIAN_POINT('Ctrl Pts',(-2.89843150791676,-2.88125160684509,
-34.3548142786892));
#27724=CARTESIAN_POINT('Ctrl Pts',(-2.9829164376061,-2.79095584455565,-34.3608229490651));
#27725=CARTESIAN_POINT('Ctrl Pts',(-3.06454997763867,-2.7037075891244,-34.3666288251601));
#27726=CARTESIAN_POINT('Ctrl Pts',(-3.14238895228346,-2.61283572932098,
-34.3724347012551));
#27727=CARTESIAN_POINT('Ctrl Pts',(-3.21610481112445,-2.51870896370782,
-34.3782405773501));
#27728=CARTESIAN_POINT('Ctrl Pts',(-3.28980998875537,-2.42459583678481,
-34.3840456121908));
#27729=CARTESIAN_POINT('Ctrl Pts',(-3.35939298721425,-2.32722906314811,
-34.3898506470315));
#27730=CARTESIAN_POINT('Ctrl Pts',(-3.42456585272475,-2.22701004046942,
-34.3956556818722));
#27731=CARTESIAN_POINT('Ctrl Pts',(-3.48974462582455,-2.12678193344525,
-34.4014612429098));
#27732=CARTESIAN_POINT('Ctrl Pts',(-3.55051224871766,-2.0237014054016,-34.4072668039475));
#27733=CARTESIAN_POINT('Ctrl Pts',(-3.60662472871704,-1.9181978694094,-34.4130723649851));
#27734=CARTESIAN_POINT('Ctrl Pts',(-3.6627555117701,-1.81265991973804,-34.4188798197101));
#27735=CARTESIAN_POINT('Ctrl Pts',(-3.71422794057079,-1.70469775031853,
-34.4246872744352));
#27736=CARTESIAN_POINT('Ctrl Pts',(-3.76084479430878,-1.59476375464222,
-34.4304947291602));
#27737=CARTESIAN_POINT('Ctrl Pts',(-3.80751303121828,-1.48470858482176,
-34.4363085851204));
#27738=CARTESIAN_POINT('Ctrl Pts',(-3.84931485079231,-1.37267762631494,
-34.4421224410805));
#27739=CARTESIAN_POINT('Ctrl Pts',(-3.88610179775092,-1.25914169874445,
-34.4479362970407));
#27740=CARTESIAN_POINT('Ctrl Pts',(-3.92291294771529,-1.14553107319179,
-34.4537539780747));
#27741=CARTESIAN_POINT('Ctrl Pts',(-3.95470254576335,-1.03041389900235,
-34.4595716591087));
#27742=CARTESIAN_POINT('Ctrl Pts',(-3.98137287746323,-0.914272940975595,
-34.4653893401428));
#27743=CARTESIAN_POINT('Ctrl Pts',(-4.00808100092164,-0.797967411653265,
-34.4712152648087));
#27744=CARTESIAN_POINT('Ctrl Pts',(-4.02965530652827,-0.680635602909504,
-34.4770411894746));
#27745=CARTESIAN_POINT('Ctrl Pts',(-4.04604967492253,-0.562767294766934,
-34.4828671141405));
#27746=CARTESIAN_POINT('Ctrl Pts',(-4.04993108837527,-0.534861636807215,
-34.4842464184131));
#27747=CARTESIAN_POINT('Ctrl Pts',(-4.05352238634429,-0.506925913458926,
-34.4856257226857));
#27748=CARTESIAN_POINT('Ctrl Pts',(-4.05682338424715,-0.478966626212638,
-34.4870050269583));
#27749=CARTESIAN_POINT('Ctrl Pts',(-4.07547461035645,-0.320991673294925,
-34.4947983417737));
#27750=CARTESIAN_POINT('Ctrl Pts',(-4.08490059976322,-0.161906717262808,
-34.5025916565891));
#27751=CARTESIAN_POINT('Ctrl Pts',(-4.08499921798737,-0.00252765554147077,
-34.5103849714045));
#27752=CARTESIAN_POINT('Origin',(0.,0.,-25.2396150285955));
#27753=CARTESIAN_POINT('',(2.48705727606859,3.24064362520075,-32.4530286559313));
#27754=CARTESIAN_POINT('',(2.48705727606861,3.24064362520074,-32.5574517732253));
#27755=CARTESIAN_POINT('',(2.4870572760686,3.24064362520075,-25.2396150285955));
#27756=CARTESIAN_POINT('',(-4.08393919123128,-0.00301203127919971,-33.3646149993214));
#27757=CARTESIAN_POINT('Ctrl Pts',(2.48705727606861,3.24064362520074,-32.5574517732253));
#27758=CARTESIAN_POINT('Ctrl Pts',(2.58172320530517,3.16799151798577,-32.5632616020185));
#27759=CARTESIAN_POINT('Ctrl Pts',(2.67328514414928,3.09112485577708,-32.5690714308118));
#27760=CARTESIAN_POINT('Ctrl Pts',(2.76135115698028,3.01034296847447,-32.5748812596051));
#27761=CARTESIAN_POINT('Ctrl Pts',(2.84937101736654,2.92960341625062,-32.5806880436619));
#27762=CARTESIAN_POINT('Ctrl Pts',(2.9338982955662,2.84495299497576,-32.5864948277187));
#27763=CARTESIAN_POINT('Ctrl Pts',(3.01457442907343,2.75673103722082,-32.5923016117755));
#27764=CARTESIAN_POINT('Ctrl Pts',(3.09522959340846,2.66853200993298,-32.5981068865451));
#27765=CARTESIAN_POINT('Ctrl Pts',(3.17203532837339,2.57676359299807,-32.6039121613148));
#27766=CARTESIAN_POINT('Ctrl Pts',(3.24467064842198,2.48180123766366,-32.6097174360844));
#27767=CARTESIAN_POINT('Ctrl Pts',(3.31730419799415,2.38684119702424,-32.6155225693512));
#27768=CARTESIAN_POINT('Ctrl Pts',(3.38576728708351,2.28868769701797,-32.621327702618));
#27769=CARTESIAN_POINT('Ctrl Pts',(3.4497802746404,2.18774794176615,-32.6271328358848));
#27770=CARTESIAN_POINT('Ctrl Pts',(3.51380677956652,2.08678687146571,-32.6329391949986));
#27771=CARTESIAN_POINT('Ctrl Pts',(3.57338109574889,1.98303872041235,-32.6387455541124));
#27772=CARTESIAN_POINT('Ctrl Pts',(3.62826817427027,1.87693768025938,-32.6445519132262));
#27773=CARTESIAN_POINT('Ctrl Pts',(3.68321269754718,1.77072559487543,-32.650364349269));
#27774=CARTESIAN_POINT('Ctrl Pts',(3.73345999844513,1.66215606547514,-32.6561767853119));
#27775=CARTESIAN_POINT('Ctrl Pts',(3.77882198208528,1.55168599520299,-32.6619892213547));
#27776=CARTESIAN_POINT('Ctrl Pts',(3.82420913072869,1.44115464058092,-32.6678048819032));
#27777=CARTESIAN_POINT('Ctrl Pts',(3.86470542475532,1.32872102830188,-32.6736205424516));
#27778=CARTESIAN_POINT('Ctrl Pts',(3.90017230377922,1.21485842830903,-32.6794362030001));
#27779=CARTESIAN_POINT('Ctrl Pts',(3.93569417491232,1.10081928206499,-32.6852608808472));
#27780=CARTESIAN_POINT('Ctrl Pts',(3.9661709492188,0.985347116488283,-32.6910855586943));
#27781=CARTESIAN_POINT('Ctrl Pts',(3.99151484202714,0.868927077421931,-32.6969102365414));
#27782=CARTESIAN_POINT('Ctrl Pts',(4.00987752083801,0.784576034719471,-32.7011304520108));
#27783=CARTESIAN_POINT('Ctrl Pts',(4.02554672280569,0.699727619360669,-32.7053506674801));
#27784=CARTESIAN_POINT('Ctrl Pts',(4.03850610398736,0.614567692005377,-32.7095708829494));
#27785=CARTESIAN_POINT('Ctrl Pts',(4.05639482136825,0.497015638301612,-32.7153963340847));
#27786=CARTESIAN_POINT('Ctrl Pts',(4.06917537424636,0.378493836629278,-32.72122178522));
#27787=CARTESIAN_POINT('Ctrl Pts',(4.07675032949716,0.259483623654406,-32.7270472363553));
#27788=CARTESIAN_POINT('Ctrl Pts',(4.08431577691211,0.140622788402665,-32.7328653755751));
#27789=CARTESIAN_POINT('Ctrl Pts',(4.08668859704055,0.0212751648462426,
-32.7386835147948));
#27790=CARTESIAN_POINT('Ctrl Pts',(4.08382264634036,-0.0980693287305154,
-32.7445016540146));
#27791=CARTESIAN_POINT('Ctrl Pts',(4.08095954736724,-0.217295070116563,
-32.7503140039703));
#27792=CARTESIAN_POINT('Ctrl Pts',(4.07286805768413,-0.336517282128182,
-32.7561263539261));
#27793=CARTESIAN_POINT('Ctrl Pts',(4.0595539991492,-0.455243152602845,-32.7619387038819));
#27794=CARTESIAN_POINT('Ctrl Pts',(4.04579023927839,-0.57797915886101,-32.7679473742558));
#27795=CARTESIAN_POINT('Ctrl Pts',(4.02644483800421,-0.700184257555691,
-32.7739560446298));
#27796=CARTESIAN_POINT('Ctrl Pts',(4.00158280818318,-0.821316034941986,
-32.7799647150038));
#27797=CARTESIAN_POINT('Ctrl Pts',(3.97755987869073,-0.938359581602993,
-32.7857705911039));
#27798=CARTESIAN_POINT('Ctrl Pts',(3.9483867759184,-1.05440065611912,-32.7915764672039));
#27799=CARTESIAN_POINT('Ctrl Pts',(3.91417450767327,-1.16895805035113,-32.797382343304));
#27800=CARTESIAN_POINT('Ctrl Pts',(3.87996719668473,-1.28349884555519,-32.8031873781498));
#27801=CARTESIAN_POINT('Ctrl Pts',(3.84072228906231,-1.39655599716866,-32.8089924129956));
#27802=CARTESIAN_POINT('Ctrl Pts',(3.79660094001163,-1.50766252931577,-32.8147974478414));
#27803=CARTESIAN_POINT('Ctrl Pts',(3.7524755915848,-1.61877913270556,-32.8206030088841));
#27804=CARTESIAN_POINT('Ctrl Pts',(3.70347307347273,-1.72794438585373,-32.8264085699268));
#27805=CARTESIAN_POINT('Ctrl Pts',(3.6498028104171,-1.8347109976973,-32.8322141309695));
#27806=CARTESIAN_POINT('Ctrl Pts',(3.59611504092265,-1.94151243521623,-32.8380215856996));
#27807=CARTESIAN_POINT('Ctrl Pts',(3.53775668159944,-2.04591331103718,-32.8438290404296));
#27808=CARTESIAN_POINT('Ctrl Pts',(3.47498294221769,-2.14749122263541,-32.8496364951597));
#27809=CARTESIAN_POINT('Ctrl Pts',(3.4121400108264,-2.2491810979289,-32.8554503511249));
#27810=CARTESIAN_POINT('Ctrl Pts',(3.34487219957761,-2.34804145083341,-32.86126420709));
#27811=CARTESIAN_POINT('Ctrl Pts',(3.27347793879498,-2.44367902643177,-32.8670780630552));
#27812=CARTESIAN_POINT('Ctrl Pts',(3.20203670603364,-2.53937952426109,-32.8728957440942));
#27813=CARTESIAN_POINT('Ctrl Pts',(3.12646387447464,-2.63185270681192,-32.8787134251331));
#27814=CARTESIAN_POINT('Ctrl Pts',(3.04709694760438,-2.72073982436765,-32.8845311061721));
#27815=CARTESIAN_POINT('Ctrl Pts',(2.96761755810181,-2.80975289462953,-32.8903570308429));
#27816=CARTESIAN_POINT('Ctrl Pts',(2.88433362686235,-2.89516946694921,-32.8961829555137));
#27817=CARTESIAN_POINT('Ctrl Pts',(2.79761820097002,-2.97666884311998,-32.9020088801845));
#27818=CARTESIAN_POINT('Ctrl Pts',(2.7770880774276,-2.99596405206578,-32.9033881844088));
#27819=CARTESIAN_POINT('Ctrl Pts',(2.75636575017673,-3.01503987859658,-32.904767488633));
#27820=CARTESIAN_POINT('Ctrl Pts',(2.73545641829513,-3.03389241463965,-32.9061467928573));
#27821=CARTESIAN_POINT('Ctrl Pts',(2.64714646539456,-3.11351555034991,-32.9119722439893));
#27822=CARTESIAN_POINT('Ctrl Pts',(2.5552158770103,-3.18940709734534,-32.9177976951212));
#27823=CARTESIAN_POINT('Ctrl Pts',(2.46001294474537,-3.26122083148094,-32.9236231462532));
#27824=CARTESIAN_POINT('Ctrl Pts',(2.36492950808498,-3.33294442736795,-32.9294412854696));
#27825=CARTESIAN_POINT('Ctrl Pts',(2.26658222001921,-3.40060014728236,-32.935259424686));
#27826=CARTESIAN_POINT('Ctrl Pts',(2.16535476120644,-3.46387987062493,-32.9410775639024));
#27827=CARTESIAN_POINT('Ctrl Pts',(2.06422802746459,-3.52709662829894,-32.9468899138548));
#27828=CARTESIAN_POINT('Ctrl Pts',(1.96022716842146,-3.58594583682477,-32.9527022638071));
#27829=CARTESIAN_POINT('Ctrl Pts',(1.85376687652398,-3.6401611732865,-32.9585146137595));
#27830=CARTESIAN_POINT('Ctrl Pts',(1.74371073618401,-3.69620771018643,-32.9645232841347));
#27831=CARTESIAN_POINT('Ctrl Pts',(1.63102643496968,-3.74730153529941,-32.97053195451));
#27832=CARTESIAN_POINT('Ctrl Pts',(1.5162026532571,-3.79319845437279,-32.9765406248852));
#27833=CARTESIAN_POINT('Ctrl Pts',(1.40525420577434,-3.83754633979761,-32.9823465009818));
#27834=CARTESIAN_POINT('Ctrl Pts',(1.2923087726332,-3.87704228917243,-32.9881523770784));
#27835=CARTESIAN_POINT('Ctrl Pts',(1.17782923873314,-3.91151419329974,-32.9939582531751));
#27836=CARTESIAN_POINT('Ctrl Pts',(1.0633662925797,-3.94598110254987,-32.9997632880174));
#27837=CARTESIAN_POINT('Ctrl Pts',(0.947370078327658,-3.97542529669491,
-33.0055683228597));
#27838=CARTESIAN_POINT('Ctrl Pts',(0.830319192253988,-3.99972437037537,
-33.011373357702));
#27839=CARTESIAN_POINT('Ctrl Pts',(0.713257696112499,-4.02402564664335,
-33.0171789187412));
#27840=CARTESIAN_POINT('Ctrl Pts',(0.595141737588523,-4.04318079223594,
-33.0229844797804));
#27841=CARTESIAN_POINT('Ctrl Pts',(0.4764600382136,-4.05711853807422,-33.0287900408196));
#27842=CARTESIAN_POINT('Ctrl Pts',(0.357739626639744,-4.07106083019716,
-33.0345974955461));
#27843=CARTESIAN_POINT('Ctrl Pts',(0.238453512227109,-4.07978229038899,
-33.0404049502727));
#27844=CARTESIAN_POINT('Ctrl Pts',(0.119094829578062,-4.0832635748342,-33.0462124049992));
#27845=CARTESIAN_POINT('Ctrl Pts',(-0.00039541552347408,-4.08674869650607,
-33.0520262609609));
#27846=CARTESIAN_POINT('Ctrl Pts',(-0.119957980454486,-4.08498210146,-33.0578401169225));
#27847=CARTESIAN_POINT('Ctrl Pts',(-0.239100284959963,-4.07799657353118,
-33.0636539728842));
#27848=CARTESIAN_POINT('Ctrl Pts',(-0.358320976015313,-4.07100644965774,
-33.0694716539196));
#27849=CARTESIAN_POINT('Ctrl Pts',(-0.47712045105476,-4.05879059621428,
-33.0752893349551));
#27850=CARTESIAN_POINT('Ctrl Pts',(-0.595013439880053,-4.04143340986365,
-33.0811070159906));
#27851=CARTESIAN_POINT('Ctrl Pts',(-0.713073482620973,-4.02405162844614,
-33.0869329406579));
#27852=CARTESIAN_POINT('Ctrl Pts',(-0.830224076280858,-4.00151405052528,
-33.0927588653252));
#27853=CARTESIAN_POINT('Ctrl Pts',(-0.945992164063851,-3.97395568993035,
-33.0985847899925));
#27854=CARTESIAN_POINT('Ctrl Pts',(-0.973400588560486,-3.96743116957174,
-33.09996409425));
#27855=CARTESIAN_POINT('Ctrl Pts',(-1.00073159851543,-3.96062544127137,
-33.1013433985076));
#27856=CARTESIAN_POINT('Ctrl Pts',(-1.02797906981974,-3.95354069563126,
-33.1027227027651));
#27857=CARTESIAN_POINT('Ctrl Pts',(-1.14305796681636,-3.92361847992695,
-33.1085481538981));
#27858=CARTESIAN_POINT('Ctrl Pts',(-1.25701341679574,-3.88861968836278,
-33.1143736050311));
#27859=CARTESIAN_POINT('Ctrl Pts',(-1.36936467170234,-3.84864461803029,
-33.1201990561641));
#27860=CARTESIAN_POINT('Ctrl Pts',(-1.4815749069912,-3.80871972309764,-33.1260171953815));
#27861=CARTESIAN_POINT('Ctrl Pts',(-1.59218457109093,-3.76383110851015,
-33.1318353345989));
#27862=CARTESIAN_POINT('Ctrl Pts',(-1.70072525783867,-3.71412958812015,
-33.1376534738164));
#27863=CARTESIAN_POINT('Ctrl Pts',(-1.80915794258291,-3.66447752258382,
-33.1434658237698));
#27864=CARTESIAN_POINT('Ctrl Pts',(-1.91552537673333,-3.61002224751509,
-33.1492781737232));
#27865=CARTESIAN_POINT('Ctrl Pts',(-2.01937698927143,-3.55096347139774,
-33.1550905236766));
#27866=CARTESIAN_POINT('Ctrl Pts',(-2.1267363383542,-3.48990990076341,-33.1610991940514));
#27867=CARTESIAN_POINT('Ctrl Pts',(-2.23140648815104,-3.42393649366664,
-33.1671078644263));
#27868=CARTESIAN_POINT('Ctrl Pts',(-2.33291463067306,-3.35331691404072,
-33.1731165348011));
#27869=CARTESIAN_POINT('Ctrl Pts',(-2.43099684547556,-3.28508076464384,
-33.1789224108987));
#27870=CARTESIAN_POINT('Ctrl Pts',(-2.5261266845148,-3.21250725285454,-33.1847282869964));
#27871=CARTESIAN_POINT('Ctrl Pts',(-2.61790572415689,-3.1358881707463,-33.190534163094));
#27872=CARTESIAN_POINT('Ctrl Pts',(-2.70967146528695,-3.05928019051699,
-33.1963391979373));
#27873=CARTESIAN_POINT('Ctrl Pts',(-2.79808705946827,-2.9786280671734,-33.2021442327806));
#27874=CARTESIAN_POINT('Ctrl Pts',(-2.88278693919141,-2.89426406245654,
-33.2079492676239));
#27875=CARTESIAN_POINT('Ctrl Pts',(-2.96749449652806,-2.80989241057152,
-33.2137548286642));
#27876=CARTESIAN_POINT('Ctrl Pts',(-3.04848538064976,-2.7218084962934,-33.2195603897044));
#27877=CARTESIAN_POINT('Ctrl Pts',(-3.12543115015846,-2.6303811749667,-33.2253659507446));
#27878=CARTESIAN_POINT('Ctrl Pts',(-3.20240201822857,-2.53892403141254,
-33.2311734054721));
#27879=CARTESIAN_POINT('Ctrl Pts',(-3.27532488496593,-2.44412162389534,
-33.2369808601997));
#27880=CARTESIAN_POINT('Ctrl Pts',(-3.34391223716288,-2.34637506595863,
-33.2427883149273));
#27881=CARTESIAN_POINT('Ctrl Pts',(-3.41257518939194,-2.24852076741549,
-33.2486021708899));
#27882=CARTESIAN_POINT('Ctrl Pts',(-3.47689285389555,-2.14771617511677,
-33.2544160268525));
#27883=CARTESIAN_POINT('Ctrl Pts',(-3.53662154811065,-2.04439062447456,
-33.2602298828152));
#27884=CARTESIAN_POINT('Ctrl Pts',(-3.59638953925116,-1.94099709350043,
-33.2660475638516));
#27885=CARTESIAN_POINT('Ctrl Pts',(-3.65156235915723,-1.83507966201013,
-33.271865244888));
#27886=CARTESIAN_POINT('Ctrl Pts',(-3.70194344356619,-1.72708996309899,
-33.2776829259245));
#27887=CARTESIAN_POINT('Ctrl Pts',(-3.75239591777952,-1.61894724319656,
-33.2835088505928));
#27888=CARTESIAN_POINT('Ctrl Pts',(-3.79804294926478,-1.5087267708014,-33.289334775261));
#27889=CARTESIAN_POINT('Ctrl Pts',(-3.83873695890835,-1.39689783460032,
-33.2951606999293));
#27890=CARTESIAN_POINT('Ctrl Pts',(-3.84837138152122,-1.37042201564943,
-33.2965400041772));
#27891=CARTESIAN_POINT('Ctrl Pts',(-3.85772840126692,-1.34385609362042,
-33.2979193084251));
#27892=CARTESIAN_POINT('Ctrl Pts',(-3.86680647728966,-1.31720638746962,
-33.2992986126729));
#27893=CARTESIAN_POINT('Ctrl Pts',(-3.91171149104778,-1.18538270386582,
-33.306121388344));
#27894=CARTESIAN_POINT('Ctrl Pts',(-3.94990424892378,-1.05116500701228,
-33.3129441640151));
#27895=CARTESIAN_POINT('Ctrl Pts',(-3.98116232529437,-0.91518934634136,
-33.3197669396861));
#27896=CARTESIAN_POINT('Ctrl Pts',(-4.01227614441052,-0.779841218703709,
-33.3265582279785));
#27897=CARTESIAN_POINT('Ctrl Pts',(-4.03651905423974,-0.642751411539236,
-33.333349516271));
#27898=CARTESIAN_POINT('Ctrl Pts',(-4.05371878773402,-0.504568122231469,
-33.3401408045634));
#27899=CARTESIAN_POINT('Ctrl Pts',(-4.0707767280463,-0.367524004545033,
-33.3468761060362));
#27900=CARTESIAN_POINT('Ctrl Pts',(-4.08090705786169,-0.229404471212952,
-33.353611407509));
#27901=CARTESIAN_POINT('Ctrl Pts',(-4.08398938536452,-0.0908608839378785,
-33.3603467089818));
#27902=CARTESIAN_POINT('Ctrl Pts',(-4.08464049359338,-0.0615950549015332,
-33.3617694683119));
#27903=CARTESIAN_POINT('Ctrl Pts',(-4.08497727930409,-0.0323103685043114,
-33.3631922276419));
#27904=CARTESIAN_POINT('Ctrl Pts',(-4.08499888879145,-0.00301306698060582,
-33.3646149869719));
#27905=CARTESIAN_POINT('Ctrl Pts',(-4.08142719209529,-0.00300957616263146,
-33.3646150285955));
#27906=CARTESIAN_POINT('Ctrl Pts',(-4.07512000112023,0.897168111157932,
-33.4083681932572));
#27907=CARTESIAN_POINT('Ctrl Pts',(-3.3405993134047,3.15482004326997,-33.5176466612216));
#27908=CARTESIAN_POINT('Ctrl Pts',(-0.208040431483893,4.54234690697773,
-33.6651940846335));
#27909=CARTESIAN_POINT('Ctrl Pts',(1.8561899212011,3.7134471707538,-33.7689883433836));
#27910=CARTESIAN_POINT('Ctrl Pts',(2.48364276907218,3.23615213332547,-33.8072572988311));
#27911=CARTESIAN_POINT('',(-4.0849984546357,0.00355325540345546,-33.2603849714311));
#27912=CARTESIAN_POINT('Ctrl Pts',(-4.0849984546357,0.00355325540344558,
-33.2603849714311));
#27913=CARTESIAN_POINT('Ctrl Pts',(-4.08485806388176,0.16495342166653,-33.2682457374445));
#27914=CARTESIAN_POINT('Ctrl Pts',(-4.07514796326737,0.325942653816538,
-33.2761065034578));
#27915=CARTESIAN_POINT('Ctrl Pts',(-4.0560388768652,0.485565267866275,-33.2839672694712));
#27916=CARTESIAN_POINT('Ctrl Pts',(-4.03692979046304,0.645187881916002,
-33.2918280354846));
#27917=CARTESIAN_POINT('Ctrl Pts',(-4.0084218836177,0.803444375325491,-33.299688801498));
#27918=CARTESIAN_POINT('Ctrl Pts',(-3.9707387557445,0.959405406295278,-33.3075495675114));
#27919=CARTESIAN_POINT('Ctrl Pts',(-3.94281256896416,1.07498490107533,-33.3133750186434));
#27920=CARTESIAN_POINT('Ctrl Pts',(-3.90979112428803,1.18952897197209,-33.3192004697754));
#27921=CARTESIAN_POINT('Ctrl Pts',(-3.87176638399298,1.3025552071916,-33.3250259209074));
#27922=CARTESIAN_POINT('Ctrl Pts',(-3.83378937110738,1.41543957558005,-33.3308440601238));
#27923=CARTESIAN_POINT('Ctrl Pts',(-3.79082168255022,1.52680951428498,-33.3366621993402));
#27924=CARTESIAN_POINT('Ctrl Pts',(-3.74300600338184,1.63619407731708,-33.3424803385566));
#27925=CARTESIAN_POINT('Ctrl Pts',(-3.6952379025852,1.74546979865763,-33.348292688509));
#27926=CARTESIAN_POINT('Ctrl Pts',(-3.64263157049037,1.85276370272238,-33.3541050384614));
#27927=CARTESIAN_POINT('Ctrl Pts',(-3.58537888812054,1.9576218298281,-33.3599173884137));
#27928=CARTESIAN_POINT('Ctrl Pts',(-3.52619241461574,2.06602168997119,-33.365926058789));
#27929=CARTESIAN_POINT('Ctrl Pts',(-3.46204030233133,2.17181789592515,-33.3719347291642));
#27930=CARTESIAN_POINT('Ctrl Pts',(-3.39318799183319,2.27453297449807,-33.3779433995394));
#27931=CARTESIAN_POINT('Ctrl Pts',(-3.32665946576081,2.3737813909045,-33.3837492756361));
#27932=CARTESIAN_POINT('Ctrl Pts',(-3.25574313323563,2.47015293580079,-33.3895551517327));
#27933=CARTESIAN_POINT('Ctrl Pts',(-3.18072384753942,2.56324419548626,-33.3953610278293));
#27934=CARTESIAN_POINT('Ctrl Pts',(-3.10571543191632,2.65632196652293,-33.4011660626716));
#27935=CARTESIAN_POINT('Ctrl Pts',(-3.02660550140437,2.74612008000037,-33.4069710975139));
#27936=CARTESIAN_POINT('Ctrl Pts',(-2.94371994149808,2.83226727305644,-33.4127761323563));
#27937=CARTESIAN_POINT('Ctrl Pts',(-2.86082686843711,2.91842227491765,-33.4185816933955));
#27938=CARTESIAN_POINT('Ctrl Pts',(-2.77415776842686,3.00092540433822,-33.4243872544347));
#27939=CARTESIAN_POINT('Ctrl Pts',(-2.68407575758724,3.07944188572093,-33.4301928154739));
#27940=CARTESIAN_POINT('Ctrl Pts',(-2.59396436334027,3.15798397800791,-33.4360002702005));
#27941=CARTESIAN_POINT('Ctrl Pts',(-2.50043815167015,3.23253656810522,-33.441807724927));
#27942=CARTESIAN_POINT('Ctrl Pts',(-2.4038932003654,3.30280524421847,-33.4476151796536));
#27943=CARTESIAN_POINT('Ctrl Pts',(-2.30724183291824,3.37315137359408,-33.4534290356153));
#27944=CARTESIAN_POINT('Ctrl Pts',(-2.20756541428628,3.43920392358034,-33.4592428915769));
#27945=CARTESIAN_POINT('Ctrl Pts',(-2.10528899843033,3.50071181805761,-33.4650567475385));
#27946=CARTESIAN_POINT('Ctrl Pts',(-2.002945292493,3.56226018003846,-33.470874428574));
#27947=CARTESIAN_POINT('Ctrl Pts',(-1.89799854028645,3.61925773741008,-33.4766921096095));
#27948=CARTESIAN_POINT('Ctrl Pts',(-1.79089690554167,3.67150013941458,-33.482509790645));
#27949=CARTESIAN_POINT('Ctrl Pts',(-1.68364350818876,3.72381656870356,-33.4883357153123));
#27950=CARTESIAN_POINT('Ctrl Pts',(-1.57422950683071,3.77136423237152,-33.4941616399796));
#27951=CARTESIAN_POINT('Ctrl Pts',(-1.46312156587967,3.81398745192716,-33.4999875646469));
#27952=CARTESIAN_POINT('Ctrl Pts',(-1.43681644442011,3.82407862054941,-33.5013668689043));
#27953=CARTESIAN_POINT('Ctrl Pts',(-1.41041643265913,3.83389398716217,-33.5027461731618));
#27954=CARTESIAN_POINT('Ctrl Pts',(-1.38392782194091,3.8434319017849,-33.5041254774192));
#27955=CARTESIAN_POINT('Ctrl Pts',(-1.2720539503939,3.88371500483929,-33.5099509285522));
#27956=CARTESIAN_POINT('Ctrl Pts',(-1.15824082603233,3.91917389249815,-33.5157763796852));
#27957=CARTESIAN_POINT('Ctrl Pts',(-1.04294185843482,3.94961989056219,-33.5216018308182));
#27958=CARTESIAN_POINT('Ctrl Pts',(-0.927787610327543,3.98002767380601,
-33.5274199700356));
#27959=CARTESIAN_POINT('Ctrl Pts',(-0.811151619532936,4.00543497911748,
-33.533238109253));
#27960=CARTESIAN_POINT('Ctrl Pts',(-0.693505633569845,4.02570179424742,
-33.5390562484704));
#27961=CARTESIAN_POINT('Ctrl Pts',(-0.575976709720327,4.04594844314563,
-33.5448685984238));
#27962=CARTESIAN_POINT('Ctrl Pts',(-0.457440189850825,4.06106470881374,
-33.5506809483772));
#27963=CARTESIAN_POINT('Ctrl Pts',(-0.338380709729531,4.07096100390104,
-33.5564932983306));
#27964=CARTESIAN_POINT('Ctrl Pts',(-0.215299825614357,4.08119156048979,
-33.5625019687055));
#27965=CARTESIAN_POINT('Ctrl Pts',(-0.091660457871997,4.08584316738755,
-33.5685106390803));
#27966=CARTESIAN_POINT('Ctrl Pts',(0.0319926461436455,4.08487471908169,
-33.5745193094552));
#27967=CARTESIAN_POINT('Ctrl Pts',(0.15147242390054,4.08393895617243,-33.5803251855528));
#27968=CARTESIAN_POINT('Ctrl Pts',(0.270964585161165,4.07775637691233,-33.5861310616504));
#27969=CARTESIAN_POINT('Ctrl Pts',(0.389975538435989,4.06634283840179,-33.591936937748));
#27970=CARTESIAN_POINT('Ctrl Pts',(0.508969247374796,4.05493095367932,-33.5977419725913));
#27971=CARTESIAN_POINT('Ctrl Pts',(0.627481480948872,4.03828965602805,-33.6035470074346));
#27972=CARTESIAN_POINT('Ctrl Pts',(0.745022913854255,4.01648675559028,-33.609352042278));
#27973=CARTESIAN_POINT('Ctrl Pts',(0.862575001292974,3.99468187883042,-33.6151576033182));
#27974=CARTESIAN_POINT('Ctrl Pts',(0.979155711911009,3.96771454345726,-33.6209631643584));
#27975=CARTESIAN_POINT('Ctrl Pts',(1.09428569935645,3.93570372464493,-33.6267687253986));
#27976=CARTESIAN_POINT('Ctrl Pts',(1.20945324048528,3.90368246438132,-33.6325761801261));
#27977=CARTESIAN_POINT('Ctrl Pts',(1.32316872443695,3.86661455812985,-33.6383836348537));
#27978=CARTESIAN_POINT('Ctrl Pts',(1.43496836976327,3.82466871477504,-33.6441910895812));
#27979=CARTESIAN_POINT('Ctrl Pts',(1.54689124563445,3.78267663684482,-33.6500049455439));
#27980=CARTESIAN_POINT('Ctrl Pts',(1.65689368556221,3.73579603311961,-33.6558188015065));
#27981=CARTESIAN_POINT('Ctrl Pts',(1.76453214759268,3.68424365373844,-33.6616326574691));
#27982=CARTESIAN_POINT('Ctrl Pts',(1.87224142752183,3.63265735682342,-33.6674503385056));
#27983=CARTESIAN_POINT('Ctrl Pts',(1.97758327299647,3.5763933546384,-33.673268019542));
#27984=CARTESIAN_POINT('Ctrl Pts',(2.08014044003778,3.51571340551522,-33.6790857005784));
#27985=CARTESIAN_POINT('Ctrl Pts',(2.18284293019341,3.4549474731357,-33.6849116252467));
#27986=CARTESIAN_POINT('Ctrl Pts',(2.28275252601363,3.38975332706837,-33.690737549915));
#27987=CARTESIAN_POINT('Ctrl Pts',(2.3794824434069,3.32043495667636,-33.6965634745832));
#27988=CARTESIAN_POINT('Ctrl Pts',(2.40238352667851,3.30402363518059,-33.6979427788312));
#27989=CARTESIAN_POINT('Ctrl Pts',(2.4251065366247,3.28738131410434,-33.6993220830791));
#27990=CARTESIAN_POINT('Ctrl Pts',(2.44764663355019,3.2705123386513,-33.700701387327));
#27991=CARTESIAN_POINT('Ctrl Pts',(2.4608407229129,3.2606379015395,-33.7015087779769));
#27992=CARTESIAN_POINT('Ctrl Pts',(2.47397797477153,3.25068143719705,-33.7023161686268));
#27993=CARTESIAN_POINT('Ctrl Pts',(2.4870572760686,3.24064362520074,-33.7031235592767));
#27994=CARTESIAN_POINT('Ctrl Pts',(2.48705727606859,3.24064362520075,-32.4530286559312));
#27995=CARTESIAN_POINT('Ctrl Pts',(2.58193246648303,3.16783091885943,-32.4588406338953));
#27996=CARTESIAN_POINT('Ctrl Pts',(2.67356128451973,3.09088376133001,-32.4646526118594));
#27997=CARTESIAN_POINT('Ctrl Pts',(2.76157813222159,3.01013475107602,-32.4704645898235));
#27998=CARTESIAN_POINT('Ctrl Pts',(2.84964039440292,2.92934407636387,-32.476279566622));
#27999=CARTESIAN_POINT('Ctrl Pts',(2.9340866845969,2.84474792911086,-32.4820945434205));
#28000=CARTESIAN_POINT('Ctrl Pts',(3.01458914627439,2.75671494339996,-32.487909520219));
#28001=CARTESIAN_POINT('Ctrl Pts',(3.09522071278122,2.66854077587476,-32.4937338227148));
#28002=CARTESIAN_POINT('Ctrl Pts',(3.17189555031696,2.57691906946114,-32.4995581252106));
#28003=CARTESIAN_POINT('Ctrl Pts',(3.24432651836811,2.48225108363627,-32.5053824277063));
#28004=CARTESIAN_POINT('Ctrl Pts',(3.31008596195785,2.39630284573328,-32.5106702610976));
#28005=CARTESIAN_POINT('Ctrl Pts',(3.37234774091624,2.30784423322459,-32.5159580944888));
#28006=CARTESIAN_POINT('Ctrl Pts',(3.43092935719941,2.21719389001215,-32.5212459278801));
#28007=CARTESIAN_POINT('Ctrl Pts',(3.49546700783304,2.11732706230663,-32.5270713790312));
#28008=CARTESIAN_POINT('Ctrl Pts',(3.55574392599387,2.01448031600678,-32.5328968301824));
#28009=CARTESIAN_POINT('Ctrl Pts',(3.6114737953513,1.90905265131449,-32.5387222813335));
#28010=CARTESIAN_POINT('Ctrl Pts',(3.66713371440342,1.80375731597123,-32.5445404205693));
#28011=CARTESIAN_POINT('Ctrl Pts',(3.71825774756252,1.69588786321235,-32.5503585598051));
#28012=CARTESIAN_POINT('Ctrl Pts',(3.76460283321834,1.5858721600824,-32.5561766990409));
#28013=CARTESIAN_POINT('Ctrl Pts',(3.81090180379914,1.47596592664773,-32.5619890490129));
#28014=CARTESIAN_POINT('Ctrl Pts',(3.85243112951132,1.36391806532641,-32.5678013989849));
#28015=CARTESIAN_POINT('Ctrl Pts',(3.88899395308434,1.2501804001317,-32.5736137489569));
#28016=CARTESIAN_POINT('Ctrl Pts',(3.92679173808193,1.13260108335458,-32.5796224193248));
#28017=CARTESIAN_POINT('Ctrl Pts',(3.95928137331307,1.01321618370378,-32.5856310896928));
#28018=CARTESIAN_POINT('Ctrl Pts',(3.98629963452622,0.892547042892467,-32.5916397600608));
#28019=CARTESIAN_POINT('Ctrl Pts',(4.01240602211043,0.775950518244885,-32.5974456361774));
#28020=CARTESIAN_POINT('Ctrl Pts',(4.03340430066207,0.658155470498375,-32.6032515122941));
#28021=CARTESIAN_POINT('Ctrl Pts',(4.04919830090484,0.539646291518178,-32.6090573884108));
#28022=CARTESIAN_POINT('Ctrl Pts',(4.06499001264393,0.42115428416572,-32.6148624232733));
#28023=CARTESIAN_POINT('Ctrl Pts',(4.07557889187928,0.301948755701678,-32.6206674581358));
#28024=CARTESIAN_POINT('Ctrl Pts',(4.08092034135956,0.182521690430972,-32.6264724929983));
#28025=CARTESIAN_POINT('Ctrl Pts',(4.08626227501516,0.0630837997020384,
-32.6322780540577));
#28026=CARTESIAN_POINT('Ctrl Pts',(4.08635581497202,-0.0565752601332626,
-32.6380836151172));
#28027=CARTESIAN_POINT('Ctrl Pts',(4.08120846023082,-0.175961655312674,
-32.6438891761767));
#28028=CARTESIAN_POINT('Ctrl Pts',(4.07605942649925,-0.29538699255423,-32.6496966309236));
#28029=CARTESIAN_POINT('Ctrl Pts',(4.06566611578164,-0.414539080835525,
-32.6555040856706));
#28030=CARTESIAN_POINT('Ctrl Pts',(4.0500879922333,-0.53292800186111,-32.6613115404175));
#28031=CARTESIAN_POINT('Ctrl Pts',(4.03449269778387,-0.65144741642437,-32.6671253963996));
#28032=CARTESIAN_POINT('Ctrl Pts',(4.01370123649887,-0.769201579913466,
-32.6729392523816));
#28033=CARTESIAN_POINT('Ctrl Pts',(3.9878244461349,-0.885709425719769,-32.6787531083636));
#28034=CARTESIAN_POINT('Ctrl Pts',(3.96193063081623,-1.00229392480375,-32.6845707894195));
#28035=CARTESIAN_POINT('Ctrl Pts',(3.93094492876804,-1.11763008004322,-32.6903884704754));
#28036=CARTESIAN_POINT('Ctrl Pts',(3.89502796685284,-1.23125226393062,-32.6962061515313));
#28037=CARTESIAN_POINT('Ctrl Pts',(3.8590601107404,-1.34503545001664,-32.7020320762189));
#28038=CARTESIAN_POINT('Ctrl Pts',(3.81814718789577,-1.45709943553806,-32.7078580009066));
#28039=CARTESIAN_POINT('Ctrl Pts',(3.77249785019351,-1.56699871419391,-32.7136839255942));
#28040=CARTESIAN_POINT('Ctrl Pts',(3.76169024103059,-1.5930176776835,-32.7150632296588));
#28041=CARTESIAN_POINT('Ctrl Pts',(3.75061734824109,-1.61891541630945,-32.7164425337233));
#28042=CARTESIAN_POINT('Ctrl Pts',(3.73928231007638,-1.64468623316116,-32.7178218377879));
#28043=CARTESIAN_POINT('Ctrl Pts',(3.69140910172012,-1.75352853847376,-32.7236472889164));
#28044=CARTESIAN_POINT('Ctrl Pts',(3.63870312742187,-1.86045299892141,-32.7294727400449));
#28045=CARTESIAN_POINT('Ctrl Pts',(3.58133999098287,-1.96500098447477,-32.7352981911735));
#28046=CARTESIAN_POINT('Ctrl Pts',(3.5240488548755,-2.06941774481803,-32.7411163303864));
#28047=CARTESIAN_POINT('Ctrl Pts',(3.46211237802662,-2.17146360865253,-32.7469344695993));
#28048=CARTESIAN_POINT('Ctrl Pts',(3.39575406965653,-2.27070017800922,-32.7527526088123));
#28049=CARTESIAN_POINT('Ctrl Pts',(3.32946179026127,-2.36983800330355,-32.7585649587611));
#28050=CARTESIAN_POINT('Ctrl Pts',(3.25875665807394,-2.46617175798871,-32.7643773087101));
#28051=CARTESIAN_POINT('Ctrl Pts',(3.18390761119513,-2.5592884408315,-32.7701896586589));
#28052=CARTESIAN_POINT('Ctrl Pts',(3.10653043076955,-2.65555027273732,-32.7761983290355));
#28053=CARTESIAN_POINT('Ctrl Pts',(3.02472466091164,-2.74837347420396,-32.782206999412));
#28054=CARTESIAN_POINT('Ctrl Pts',(2.938835793223,-2.83733487281134,-32.7882156697885));
#28055=CARTESIAN_POINT('Ctrl Pts',(2.85584569852113,-2.92329379966553,-32.7940215458817));
#28056=CARTESIAN_POINT('Ctrl Pts',(2.76904397598569,-3.00564707424169,-32.7998274219748));
#28057=CARTESIAN_POINT('Ctrl Pts',(2.678782163719,-3.08404784647401,-32.805633298068));
#28058=CARTESIAN_POINT('Ctrl Pts',(2.58853343012276,-3.1624372586656,-32.8114383329068));
#28059=CARTESIAN_POINT('Ctrl Pts',(2.49482591183162,-3.23687503999613,-32.8172433677456));
#28060=CARTESIAN_POINT('Ctrl Pts',(2.39804586548011,-3.30705322410356,-32.8230484025844));
#28061=CARTESIAN_POINT('Ctrl Pts',(2.30125704650927,-3.37723776950671,-32.8288539636202));
#28062=CARTESIAN_POINT('Ctrl Pts',(2.2013954760632,-3.44316171047454,-32.8346595246559));
#28063=CARTESIAN_POINT('Ctrl Pts',(2.09887762249836,-3.5045595623096,-32.8404650856916));
#28064=CARTESIAN_POINT('Ctrl Pts',(1.9963263291404,-3.56597744120718,-32.8462725404147));
#28065=CARTESIAN_POINT('Ctrl Pts',(1.89111737934565,-3.62286608529565,-32.8520799951377));
#28066=CARTESIAN_POINT('Ctrl Pts',(1.78369256745013,-3.67500555439351,-32.8578874498608));
#28067=CARTESIAN_POINT('Ctrl Pts',(1.67614934714406,-3.72720249393562,-32.863701305819));
#28068=CARTESIAN_POINT('Ctrl Pts',(1.5663857568185,-3.77463963142747,-32.8695151617772));
#28069=CARTESIAN_POINT('Ctrl Pts',(1.45486446961969,-3.81714479356472,-32.8753290177354));
#28070=CARTESIAN_POINT('Ctrl Pts',(1.34326980991886,-3.85967792085707,-32.8811466987674));
#28071=CARTESIAN_POINT('Ctrl Pts',(1.22991553661569,-3.89727248232742,-32.8869643797995));
#28072=CARTESIAN_POINT('Ctrl Pts',(1.11527882938665,-3.92980637343902,-32.8927820608315));
#28073=CARTESIAN_POINT('Ctrl Pts',(1.00047968237937,-3.96238636495062,-32.8986079854955));
#28074=CARTESIAN_POINT('Ctrl Pts',(0.884394870114934,-3.98989128010835,
-32.9044339101594));
#28075=CARTESIAN_POINT('Ctrl Pts',(0.76751119858735,-4.01225018662134,-32.9102598348234));
#28076=CARTESIAN_POINT('Ctrl Pts',(0.739838655778987,-4.01754372154836,
-32.9116391391142));
#28077=CARTESIAN_POINT('Ctrl Pts',(0.712121353475551,-4.02254904212186,
-32.913018443405));
#28078=CARTESIAN_POINT('Ctrl Pts',(0.6843657754055,-4.02726563383316,-32.9143977476958));
#28079=CARTESIAN_POINT('Ctrl Pts',(0.567140907239768,-4.04718602029217,
-32.9202231988263));
#28080=CARTESIAN_POINT('Ctrl Pts',(0.448858034774041,-4.06201578964598,
-32.9260486499569));
#28081=CARTESIAN_POINT('Ctrl Pts',(0.32999673641773,-4.0716491933802,-32.9318741010875));
#28082=CARTESIAN_POINT('Ctrl Pts',(0.211284628873984,-4.08127050558126,
-32.9376922403025));
#28083=CARTESIAN_POINT('Ctrl Pts',(0.0919959426583443,-4.08570839247379,
-32.9435103795174));
#28084=CARTESIAN_POINT('Ctrl Pts',(-0.0273802758723824,-4.08490823893183,
-32.9493285187323));
#28085=CARTESIAN_POINT('Ctrl Pts',(-0.146637710644032,-4.08410888157228,
-32.9551408686833));
#28086=CARTESIAN_POINT('Ctrl Pts',(-0.265982098758161,-4.07808185543052,
-32.9609532186342));
#28087=CARTESIAN_POINT('Ctrl Pts',(-0.384920601103282,-4.06682445291732,
-32.9667655685851));
#28088=CARTESIAN_POINT('Ctrl Pts',(-0.507876421316165,-4.05518681554856,
-32.9727742389609));
#28089=CARTESIAN_POINT('Ctrl Pts',(-0.630398008995281,-4.03795918482162,
-32.9787829093366));
#28090=CARTESIAN_POINT('Ctrl Pts',(-0.751941906517641,-4.01519717687969,
-32.9847915797124));
#28091=CARTESIAN_POINT('Ctrl Pts',(-0.869383664010096,-3.99320339297733,
-32.9905974558074));
#28092=CARTESIAN_POINT('Ctrl Pts',(-0.985912228050297,-3.96604285837032,
-32.9964033319025));
#28093=CARTESIAN_POINT('Ctrl Pts',(-1.10104454147099,-3.93381823648436,
-33.0022092079975));
#28094=CARTESIAN_POINT('Ctrl Pts',(-1.21616017255858,-3.9015982838512,-33.0080142428382));
#28095=CARTESIAN_POINT('Ctrl Pts',(-1.3298795625645,-3.86431581317818,-33.0138192776789));
#28096=CARTESIAN_POINT('Ctrl Pts',(-1.44173301660593,-3.8221238740821,-33.0196243125196));
#28097=CARTESIAN_POINT('Ctrl Pts',(-1.5535966095935,-3.77992811050155,-33.0254298735572));
#28098=CARTESIAN_POINT('Ctrl Pts',(-1.66359354855399,-3.73282213770339,
-33.0312354345947));
#28099=CARTESIAN_POINT('Ctrl Pts',(-1.77127298511989,-3.68100760827582,
-33.0370409956323));
#28100=CARTESIAN_POINT('Ctrl Pts',(-1.87898754511049,-3.62917617772227,
-33.0428484503571));
#28101=CARTESIAN_POINT('Ctrl Pts',(-1.98438273183416,-3.572633312846,-33.048655905082));
#28102=CARTESIAN_POINT('Ctrl Pts',(-2.08703178938166,-3.51162687512645,
-33.0544633598069));
#28103=CARTESIAN_POINT('Ctrl Pts',(-2.18979399128881,-3.45055319339614,
-33.0602772157669));
#28104=CARTESIAN_POINT('Ctrl Pts',(-2.28980367123861,-3.38500632695112,
-33.0660910717268));
#28105=CARTESIAN_POINT('Ctrl Pts',(-2.38666246859223,-3.31527785577819,
-33.0719049276868));
#28106=CARTESIAN_POINT('Ctrl Pts',(-2.48358499164677,-3.24550350858965,
-33.0777226087205));
#28107=CARTESIAN_POINT('Ctrl Pts',(-2.57735218392528,-3.17154232964677,
-33.0835402897542));
#28108=CARTESIAN_POINT('Ctrl Pts',(-2.66759950862442,-3.09372556339226,
-33.089357970788));
#28109=CARTESIAN_POINT('Ctrl Pts',(-2.75797471343884,-3.01579853107643,
-33.0951838954536));
#28110=CARTESIAN_POINT('Ctrl Pts',(-2.84481980007433,-2.93400528603584,
-33.1010098201192));
#28111=CARTESIAN_POINT('Ctrl Pts',(-2.92780766242373,-2.84871326950482,
-33.1068357447847));
#28112=CARTESIAN_POINT('Ctrl Pts',(-2.94745527541399,-2.82852014144347,
-33.1082150490577));
#28113=CARTESIAN_POINT('Ctrl Pts',(-2.96688686509319,-2.80813104182631,
-33.1095943533306));
#28114=CARTESIAN_POINT('Ctrl Pts',(-2.98609843399859,-2.78755110132015,
-33.1109736576035));
#28115=CARTESIAN_POINT('Ctrl Pts',(-3.06626583517473,-2.70167366180113,
-33.1167293165784));
#28116=CARTESIAN_POINT('Ctrl Pts',(-3.14286955276453,-2.61218061687391,
-33.1224849755533));
#28117=CARTESIAN_POINT('Ctrl Pts',(-3.21556074940212,-2.51940351410895,
-33.1282406345282));
#28118=CARTESIAN_POINT('Ctrl Pts',(-3.28813850960451,-2.42677119233938,
-33.1339873116529));
#28119=CARTESIAN_POINT('Ctrl Pts',(-3.35681564336712,-2.3308653382591,-33.1397339887777));
#28120=CARTESIAN_POINT('Ctrl Pts',(-3.42128067654142,-2.23205365802982,
-33.1454806659024));
#28121=CARTESIAN_POINT('Ctrl Pts',(-3.48568814733276,-2.13333020913306,
-33.1512222116805));
#28122=CARTESIAN_POINT('Ctrl Pts',(-3.54589076438995,-2.03170643895666,
-33.1569637574586));
#28123=CARTESIAN_POINT('Ctrl Pts',(-3.60161793196347,-1.92758223486293,
-33.1627053032367));
#28124=CARTESIAN_POINT('Ctrl Pts',(-3.65730926590799,-1.82352498461347,
-33.1684431570917));
#28125=CARTESIAN_POINT('Ctrl Pts',(-3.70853067401423,-1.71697086465564,
-33.1741810109466));
#28126=CARTESIAN_POINT('Ctrl Pts',(-3.75505586227218,-1.60834712398018,
-33.1799188648016));
#28127=CARTESIAN_POINT('Ctrl Pts',(-3.80156275802397,-1.49976609136288,
-33.1856544626801));
#28128=CARTESIAN_POINT('Ctrl Pts',(-3.84337694153011,-1.38911744095059,
-33.1913900605586));
#28129=CARTESIAN_POINT('Ctrl Pts',(-3.88031925962283,-1.27685059556712,
-33.1971256584372));
#28130=CARTESIAN_POINT('Ctrl Pts',(-3.91726724257214,-1.16456653481628,
-33.2028621358312));
#28131=CARTESIAN_POINT('Ctrl Pts',(-3.94934172727531,-1.05066417837745,
-33.2085986132252));
#28132=CARTESIAN_POINT('Ctrl Pts',(-3.97641280845001,-0.935610055949977,
-33.2143350906191));
#28133=CARTESIAN_POINT('Ctrl Pts',(-4.00348552924101,-0.82054896503038,
-33.2200719154548));
#28134=CARTESIAN_POINT('Ctrl Pts',(-4.02555415539019,-0.704336379157422,
-33.2258087402905));
#28135=CARTESIAN_POINT('Ctrl Pts',(-4.04253976856566,-0.587449759183785,
-33.2315455651261));
#28136=CARTESIAN_POINT('Ctrl Pts',(-4.05953874277468,-0.47047119516113,
-33.237286902599));
#28137=CARTESIAN_POINT('Ctrl Pts',(-4.07144666714239,-0.352817954335272,
-33.2430282400718));
#28138=CARTESIAN_POINT('Ctrl Pts',(-4.0782364528454,-0.234973263761964,
-33.2487695775446));
#28139=CARTESIAN_POINT('Ctrl Pts',(-4.08281529505991,-0.155502089331045,
-33.2526413754979));
#28140=CARTESIAN_POINT('Ctrl Pts',(-4.08506760369229,-0.0759439382077033,
-33.2565131734512));
#28141=CARTESIAN_POINT('Ctrl Pts',(-4.08499845463617,0.00355325485717703,
-33.2603849714045));
#28142=CARTESIAN_POINT('Origin',(0.,0.,-25.2396150285955));
#28143=CARTESIAN_POINT('',(2.48705727606859,3.24064362520075,-31.2032093449099));
#28144=CARTESIAN_POINT('',(2.4870572760686,3.24064362520075,-31.3072405360316));
#28145=CARTESIAN_POINT('',(2.4870572760686,3.24064362520075,-25.2396150285955));
#28146=CARTESIAN_POINT('',(-4.08499995078438,0.000634106917209552,-32.1146150285602));
#28147=CARTESIAN_POINT('Ctrl Pts',(2.4870572760686,3.24064362520075,-31.3072405360316));
#28148=CARTESIAN_POINT('Ctrl Pts',(2.58177343908692,3.16795296567738,-31.3130657305817));
#28149=CARTESIAN_POINT('Ctrl Pts',(2.6731893400469,3.09119144240212,-31.3188909251318));
#28150=CARTESIAN_POINT('Ctrl Pts',(2.76095535213861,3.01070598755461,-31.3247161196819));
#28151=CARTESIAN_POINT('Ctrl Pts',(2.80526826965443,2.97006901161277,-31.3276572509862));
#28152=CARTESIAN_POINT('Ctrl Pts',(2.84865135640308,2.92848328490921,-31.3305983822904));
#28153=CARTESIAN_POINT('Ctrl Pts',(2.89106349316248,2.88599668719546,-31.3335395135947));
#28154=CARTESIAN_POINT('Ctrl Pts',(2.97506852242191,2.80184417433516,-31.3393649645186));
#28155=CARTESIAN_POINT('Ctrl Pts',(3.05553064445705,2.71388619702605,-31.3451904154425));
#28156=CARTESIAN_POINT('Ctrl Pts',(3.13208639459978,2.62245301516785,-31.3510158663664));
#28157=CARTESIAN_POINT('Ctrl Pts',(3.20854605442018,2.53113459730713,-31.3568340053711));
#28158=CARTESIAN_POINT('Ctrl Pts',(3.28110883514576,2.43634996104282,-31.3626521443759));
#28159=CARTESIAN_POINT('Ctrl Pts',(3.34944752932834,2.338466644679,-31.3684702833806));
#28160=CARTESIAN_POINT('Ctrl Pts',(3.4177182239378,2.24068072589948,-31.374282633118));
#28161=CARTESIAN_POINT('Ctrl Pts',(3.48177296152747,2.13980259365382,-31.3800949828554));
#28162=CARTESIAN_POINT('Ctrl Pts',(3.54132470353108,2.03623288063043,-31.3859073325929));
#28163=CARTESIAN_POINT('Ctrl Pts',(3.60288789378296,1.92916494722211,-31.3919160030474));
#28164=CARTESIAN_POINT('Ctrl Pts',(3.65963822815731,1.8192207308402,-31.397924673502));
#28165=CARTESIAN_POINT('Ctrl Pts',(3.71130701083638,1.70687588046606,-31.4039333439566));
#28166=CARTESIAN_POINT('Ctrl Pts',(3.7612319553154,1.5983227052873,-31.4097392198314));
#28167=CARTESIAN_POINT('Ctrl Pts',(3.80641263717735,1.48752872590933,-31.4155450957062));
#28168=CARTESIAN_POINT('Ctrl Pts',(3.84665366265959,1.3749474897419,-31.421350971581));
#28169=CARTESIAN_POINT('Ctrl Pts',(3.88688885732084,1.26238256630575,-31.4271560061993));
#28170=CARTESIAN_POINT('Ctrl Pts',(3.92218568174725,1.1480312852159,-31.4329610408177));
#28171=CARTESIAN_POINT('Ctrl Pts',(3.95239758401236,1.03236540909374,-31.438766075436));
#28172=CARTESIAN_POINT('Ctrl Pts',(3.98261222482297,0.916689048485613,-31.4445716362493));
#28173=CARTESIAN_POINT('Ctrl Pts',(4.00774092393238,0.799698250713554,-31.4503771970627));
#28174=CARTESIAN_POINT('Ctrl Pts',(4.02768768552435,0.681877487438528,-31.456182757876));
#28175=CARTESIAN_POINT('Ctrl Pts',(4.04764095344671,0.564018292821727,-31.461990212375));
#28176=CARTESIAN_POINT('Ctrl Pts',(4.06240885417604,0.44532899636973,-31.467797666874));
#28177=CARTESIAN_POINT('Ctrl Pts',(4.07194702605262,0.326301114036093,-31.473605121373));
#28178=CARTESIAN_POINT('Ctrl Pts',(4.08149571132497,0.207142033895291,-31.4794189771057));
#28179=CARTESIAN_POINT('Ctrl Pts',(4.08580312905233,0.0876440298755329,
-31.4852328328385));
#28180=CARTESIAN_POINT('Ctrl Pts',(4.08487700611757,-0.0316992885084958,
-31.4910466885712));
#28181=CARTESIAN_POINT('Ctrl Pts',(4.0839502738647,-0.151121125675586,-31.4968643693767));
#28182=CARTESIAN_POINT('Ctrl Pts',(4.07778316450658,-0.270387668005049,
-31.5026820501822));
#28183=CARTESIAN_POINT('Ctrl Pts',(4.06643532238445,-0.389009985558321,
-31.5084997309877));
#28184=CARTESIAN_POINT('Ctrl Pts',(4.05507140041231,-0.507800390493599,
-31.5143256554252));
#28185=CARTESIAN_POINT('Ctrl Pts',(4.03851215027927,-0.625944346112009,
-31.5201515798628));
#28186=CARTESIAN_POINT('Ctrl Pts',(4.01686838841442,-0.742962549632821,
-31.5259775043003));
#28187=CARTESIAN_POINT('Ctrl Pts',(4.01174415798604,-0.770666986731162,
-31.527356810701));
#28188=CARTESIAN_POINT('Ctrl Pts',(4.006335150232,-0.79830838953125,-31.5287361171018));
#28189=CARTESIAN_POINT('Ctrl Pts',(4.00064324193696,-0.825880530551567,
-31.5301154235025));
#28190=CARTESIAN_POINT('Ctrl Pts',(3.97660367076272,-0.942330482329761,
-31.53594087477));
#28191=CARTESIAN_POINT('Ctrl Pts',(3.94743702183402,-1.05791623962973,-31.5417663260374));
#28192=CARTESIAN_POINT('Ctrl Pts',(3.91321904908743,-1.17215258130468,-31.5475917773049));
#28193=CARTESIAN_POINT('Ctrl Pts',(3.87904402560938,-1.28624553729893,-31.5534099166584));
#28194=CARTESIAN_POINT('Ctrl Pts',(3.83983040525071,-1.39899205908764,-31.559228056012));
#28195=CARTESIAN_POINT('Ctrl Pts',(3.79570502028427,-1.50991668610847,-31.5650461953655));
#28196=CARTESIAN_POINT('Ctrl Pts',(3.75162354169778,-1.62073093904817,-31.5708585454566));
#28197=CARTESIAN_POINT('Ctrl Pts',(3.70264017151582,-1.72972652676446,-31.5766708955476));
#28198=CARTESIAN_POINT('Ctrl Pts',(3.64893147927402,-1.83644331781929,-31.5824832456386));
#28199=CARTESIAN_POINT('Ctrl Pts',(3.59340870102602,-1.9467646173661,-31.5884919159625));
#28200=CARTESIAN_POINT('Ctrl Pts',(3.53283586916301,-2.0546500308498,-31.5945005862863));
#28201=CARTESIAN_POINT('Ctrl Pts',(3.46746228396593,-2.15961346293122,-31.6005092566101));
#28202=CARTESIAN_POINT('Ctrl Pts',(3.40429507317844,-2.2610343536362,-31.6063151328482));
#28203=CARTESIAN_POINT('Ctrl Pts',(3.33664616612951,-2.35972694152215,-31.6121210090864));
#28204=CARTESIAN_POINT('Ctrl Pts',(3.26478674532157,-2.45527849898389,-31.6179268853245));
#28205=CARTESIAN_POINT('Ctrl Pts',(3.19293773672137,-2.55081621132059,-31.6237319203091));
#28206=CARTESIAN_POINT('Ctrl Pts',(3.11687967285738,-2.64321347236129,-31.6295369552937));
#28207=CARTESIAN_POINT('Ctrl Pts',(3.03692582220991,-2.73208831306652,-31.6353419902784));
#28208=CARTESIAN_POINT('Ctrl Pts',(2.9569647241434,-2.82097120983418,-31.6411475514606));
#28209=CARTESIAN_POINT('Ctrl Pts',(2.87310741007591,-2.90633074809517,-31.6469531126428));
#28210=CARTESIAN_POINT('Ctrl Pts',(2.78570558024516,-2.98782017869064,-31.6527586738249));
#28211=CARTESIAN_POINT('Ctrl Pts',(2.69827524123529,-3.06933618992839,-31.658566128695));
#28212=CARTESIAN_POINT('Ctrl Pts',(2.60729838534707,-3.14697930480428,-31.664373583565));
#28213=CARTESIAN_POINT('Ctrl Pts',(2.51316100784573,-3.2204420113773,-31.6701810384351));
#28214=CARTESIAN_POINT('Ctrl Pts',(2.41891986793911,-3.29398569181356,-31.6759948945402));
#28215=CARTESIAN_POINT('Ctrl Pts',(2.3215115746994,-3.36333951534805,-31.6818087506454));
#28216=CARTESIAN_POINT('Ctrl Pts',(2.22135253469191,-3.42823831094308,-31.6876226067505));
#28217=CARTESIAN_POINT('Ctrl Pts',(2.12112759767327,-3.49317980499704,-31.6934402879297));
#28218=CARTESIAN_POINT('Ctrl Pts',(2.01814866060833,-3.55366022757815,-31.6992579691088));
#28219=CARTESIAN_POINT('Ctrl Pts',(1.91285679177796,-3.60946033281278,-31.705075650288));
#28220=CARTESIAN_POINT('Ctrl Pts',(1.80741572478954,-3.6653395065739,-31.7109015750982));
#28221=CARTESIAN_POINT('Ctrl Pts',(1.69965555194913,-3.71652495199247,-31.7167274999084));
#28222=CARTESIAN_POINT('Ctrl Pts',(1.59003746195505,-3.76284544853752,-31.7225534247185));
#28223=CARTESIAN_POINT('Ctrl Pts',(1.56408509318158,-3.77381194693366,-31.7239327276158));
#28224=CARTESIAN_POINT('Ctrl Pts',(1.53802865048042,-3.78450597661719,-31.725312030513));
#28225=CARTESIAN_POINT('Ctrl Pts',(1.51187436638704,-3.7949256778311,-31.7266913334103));
#28226=CARTESIAN_POINT('Ctrl Pts',(1.40141240502279,-3.83893302396254,-31.7325167845219));
#28227=CARTESIAN_POINT('Ctrl Pts',(1.28885070777441,-3.87818380994179,-31.7383422356336));
#28228=CARTESIAN_POINT('Ctrl Pts',(1.1746361108397,-3.91247428197444,-31.7441676867452));
#28229=CARTESIAN_POINT('Ctrl Pts',(1.06056487232927,-3.94672171372878,-31.7499858259413));
#28230=CARTESIAN_POINT('Ctrl Pts',(0.944845248067957,-3.97602109890178,
-31.7558039651373));
#28231=CARTESIAN_POINT('Ctrl Pts',(0.827944031676047,-4.00021670418141,
-31.7616221043334));
#28232=CARTESIAN_POINT('Ctrl Pts',(0.711159136324298,-4.02438823393762,
-31.7674344542655));
#28233=CARTESIAN_POINT('Ctrl Pts',(0.593195385143151,-4.04346600473028,
-31.7732468041975));
#28234=CARTESIAN_POINT('Ctrl Pts',(0.474534141585862,-4.05734424820835,
-31.7790591541296));
#28235=CARTESIAN_POINT('Ctrl Pts',(0.351864944429789,-4.07169124925397,
-31.7850678245124));
#28236=CARTESIAN_POINT('Ctrl Pts',(0.228450728635298,-4.08048113494708,
-31.7910764948953));
#28237=CARTESIAN_POINT('Ctrl Pts',(0.104834559263976,-4.08365457833837,
-31.7970851652781));
#28238=CARTESIAN_POINT('Ctrl Pts',(-0.014609529809033,-4.08672091712742,
-31.8028910413546));
#28239=CARTESIAN_POINT('Ctrl Pts',(-0.134241720055493,-4.08454379782612,
-31.8086969174311));
#28240=CARTESIAN_POINT('Ctrl Pts',(-0.253568165814577,-4.07712253743807,
-31.8145027935076));
#28241=CARTESIAN_POINT('Ctrl Pts',(-0.372877321525938,-4.06970235236862,
-31.8203078283299));
#28242=CARTESIAN_POINT('Ctrl Pts',(-0.491880413732094,-4.05703956271141,
-31.8261128631522));
#28243=CARTESIAN_POINT('Ctrl Pts',(-0.610086120570589,-4.03918555224777,
-31.8319178979745));
#28244=CARTESIAN_POINT('Ctrl Pts',(-0.728302542158392,-4.02132992340841,
-31.8377234589938));
#28245=CARTESIAN_POINT('Ctrl Pts',(-0.845721031212787,-3.99828219911942,
-31.8435290200131));
#28246=CARTESIAN_POINT('Ctrl Pts',(-0.961858525623113,-3.97014523370193,
-31.8493345810324));
#28247=CARTESIAN_POINT('Ctrl Pts',(-1.07803390235364,-3.94199909042557,
-31.8551420357393));
#28248=CARTESIAN_POINT('Ctrl Pts',(-1.19292705710286,-3.90876050056796,
-31.8609494904461));
#28249=CARTESIAN_POINT('Ctrl Pts',(-1.30606881826721,-3.87058254555436,
-31.8667569451529));
#28250=CARTESIAN_POINT('Ctrl Pts',(-1.41933528932348,-3.83236250909714,
-31.8725708010951));
#28251=CARTESIAN_POINT('Ctrl Pts',(-1.53084612668865,-3.78919237076018,
-31.8783846570374));
#28252=CARTESIAN_POINT('Ctrl Pts',(-1.64015077791753,-3.74127390412631,
-31.8841985129796));
#28253=CARTESIAN_POINT('Ctrl Pts',(-1.74952734327411,-3.69332391079444,
-31.8900161939959));
#28254=CARTESIAN_POINT('Ctrl Pts',(-1.85669446646886,-3.64061954711204,
-31.8958338750121));
#28255=CARTESIAN_POINT('Ctrl Pts',(-1.96122637087928,-3.58340845036784,
-31.9016515560283));
#28256=CARTESIAN_POINT('Ctrl Pts',(-2.06590639660719,-3.5261162857136,-31.9074774806768));
#28257=CARTESIAN_POINT('Ctrl Pts',(-2.16794340309138,-3.46430485296478,
-31.9133034053253));
#28258=CARTESIAN_POINT('Ctrl Pts',(-2.26694064212117,-3.3982650169019,-31.9191293299737));
#28259=CARTESIAN_POINT('Ctrl Pts',(-2.29037852372566,-3.38262989541779,
-31.9205086344219));
#28260=CARTESIAN_POINT('Ctrl Pts',(-2.31364616841575,-3.36675793990398,
-31.92188793887));
#28261=CARTESIAN_POINT('Ctrl Pts',(-2.33673859368093,-3.3506533310389,-31.9232672433182));
#28262=CARTESIAN_POINT('Ctrl Pts',(-2.43384640131928,-3.28293055000565,
-31.9290674669623));
#28263=CARTESIAN_POINT('Ctrl Pts',(-2.52816984019052,-3.21086960220254,
-31.9348676906065));
#28264=CARTESIAN_POINT('Ctrl Pts',(-2.61929494263886,-3.13472789943027,
-31.9406679142507));
#28265=CARTESIAN_POINT('Ctrl Pts',(-2.71030537162278,-3.05868201474334,
-31.9464608387894));
#28266=CARTESIAN_POINT('Ctrl Pts',(-2.7981251548425,-2.97856584921579,-31.952253763328));
#28267=CARTESIAN_POINT('Ctrl Pts',(-2.88236925872762,-2.89468002659051,
-31.9580466878667));
#28268=CARTESIAN_POINT('Ctrl Pts',(-2.96652979121779,-2.81087741993986,
-31.9638338657387));
#28269=CARTESIAN_POINT('Ctrl Pts',(-3.04712140956654,-2.72331288349971,
-31.9696210436106));
#28270=CARTESIAN_POINT('Ctrl Pts',(-3.12379265800122,-2.63232680908311,
-31.9754082214826));
#28271=CARTESIAN_POINT('Ctrl Pts',(-3.20063753764538,-2.541134685822,-31.9812085051108));
#28272=CARTESIAN_POINT('Ctrl Pts',(-3.27354395713333,-2.44650578476795,
-31.9870087887391));
#28273=CARTESIAN_POINT('Ctrl Pts',(-3.34219549847513,-2.34881975680821,
-31.9928090723673));
#28274=CARTESIAN_POINT('Ctrl Pts',(-3.41061798646001,-2.25145965470812,
-31.9985900035613));
#28275=CARTESIAN_POINT('Ctrl Pts',(-3.47481370569665,-2.15106313236277,
-32.0043709347554));
#28276=CARTESIAN_POINT('Ctrl Pts',(-3.53451060025972,-2.04803804082143,
-32.0101518659494));
#28277=CARTESIAN_POINT('Ctrl Pts',(-3.59419958651706,-1.94502659745942,
-32.0159320313185));
#28278=CARTESIAN_POINT('Ctrl Pts',(-3.64939072674739,-1.83938763382505,
-32.0217121966876));
#28279=CARTESIAN_POINT('Ctrl Pts',(-3.69985673480307,-1.73155569992199,
-32.0274923620567));
#28280=CARTESIAN_POINT('Ctrl Pts',(-3.75032822749171,-1.62371204687171,
-32.0332731556127));
#28281=CARTESIAN_POINT('Ctrl Pts',(-3.79607339270388,-1.51367532307134,
-32.0390539491687));
#28282=CARTESIAN_POINT('Ctrl Pts',(-3.83691241130101,-1.40190161851833,
-32.0448347427246));
#28283=CARTESIAN_POINT('Ctrl Pts',(-3.87799325316331,-1.28946605961315,
-32.0506497665443));
#28284=CARTESIAN_POINT('Ctrl Pts',(-3.91410950446023,-1.17527327558181,
-32.0564647903639));
#28285=CARTESIAN_POINT('Ctrl Pts',(-3.94512885569573,-1.05980343081013,
-32.0622798141835));
#28286=CARTESIAN_POINT('Ctrl Pts',(-3.97601037479555,-0.94484666754007,
-32.0680689993856));
#28287=CARTESIAN_POINT('Ctrl Pts',(-4.00184016039536,-0.828624585574513,
-32.0738581845877));
#28288=CARTESIAN_POINT('Ctrl Pts',(-4.02253913335644,-0.711620629700959,
-32.0796473697899));
#28289=CARTESIAN_POINT('Ctrl Pts',(-4.04337668355074,-0.593833345856952,
-32.0854753129182));
#28290=CARTESIAN_POINT('Ctrl Pts',(-4.05901441865793,-0.475254101590422,
-32.0913032560466));
#28291=CARTESIAN_POINT('Ctrl Pts',(-4.0694248419718,-0.356379650854012,
-32.097131199175));
#28292=CARTESIAN_POINT('Ctrl Pts',(-4.07983526528566,-0.237505200117603,
-32.1029591423034));
#28293=CARTESIAN_POINT('Ctrl Pts',(-4.08501841828653,-0.118335964697111,
-32.1087870854318));
#28294=CARTESIAN_POINT('Ctrl Pts',(-4.08499995078438,0.000634106917214494,
-32.1146150285602));
#28295=CARTESIAN_POINT('Ctrl Pts',(-4.08499995078427,0.000634107638191378,
-32.1146150285955));
#28296=CARTESIAN_POINT('Ctrl Pts',(-4.08499442850935,0.0362092867362075,
-32.1163577368056));
#28297=CARTESIAN_POINT('Ctrl Pts',(-4.08452419335079,0.0717803130156109,
-32.1181004450158));
#28298=CARTESIAN_POINT('Ctrl Pts',(-4.08358951442185,0.107339078177262,
-32.1198431532259));
#28299=CARTESIAN_POINT('Ctrl Pts',(-4.08046510930863,0.226203411426466,
-32.1256686043772));
#28300=CARTESIAN_POINT('Ctrl Pts',(-4.07214158107509,0.345121361988938,
-32.1314940555285));
#28301=CARTESIAN_POINT('Ctrl Pts',(-4.0586079174886,0.463601954373402,-32.1373195066798));
#28302=CARTESIAN_POINT('Ctrl Pts',(-4.04509124091304,0.581933833801863,
-32.1431376459158));
#28303=CARTESIAN_POINT('Ctrl Pts',(-4.02637748224907,0.699829045080311,
-32.1489557851517));
#28304=CARTESIAN_POINT('Ctrl Pts',(-4.00250762836785,0.816797211587529,
-32.1547739243877));
#28305=CARTESIAN_POINT('Ctrl Pts',(-3.97866152587439,0.933648990441425,
-32.1605862743599));
#28306=CARTESIAN_POINT('Ctrl Pts',(-3.94966961600344,1.04957516213541,-32.166398624332));
#28307=CARTESIAN_POINT('Ctrl Pts',(-3.91562454680484,1.16409166669097,-32.1722109743042));
#28308=CARTESIAN_POINT('Ctrl Pts',(-3.88042955692181,1.28247612923273,-32.1782196446721));
#28309=CARTESIAN_POINT('Ctrl Pts',(-3.83983406048606,1.39935357072967,-32.18422831504));
#28310=CARTESIAN_POINT('Ctrl Pts',(-3.79399771690724,1.51420154672442,-32.1902369854079));
#28311=CARTESIAN_POINT('Ctrl Pts',(-3.74970836232903,1.62517337244771,-32.1960428615247));
#28312=CARTESIAN_POINT('Ctrl Pts',(-3.70052637554683,1.73425010302123,-32.2018487376416));
#28313=CARTESIAN_POINT('Ctrl Pts',(-3.64664589504588,1.8409776522666,-32.2076546137584));
#28314=CARTESIAN_POINT('Ctrl Pts',(-3.5927732216664,1.94768973700732,-32.2134596486211));
#28315=CARTESIAN_POINT('Ctrl Pts',(-3.53420359234195,2.05205295323479,-32.2192646834837));
#28316=CARTESIAN_POINT('Ctrl Pts',(-3.47117799669026,2.15363606844179,-32.2250697183464));
#28317=CARTESIAN_POINT('Ctrl Pts',(-3.40814668808747,2.25522839164378,-32.230875279406));
#28318=CARTESIAN_POINT('Ctrl Pts',(-3.34065882520363,2.35403976606273,-32.2366808404657));
#28319=CARTESIAN_POINT('Ctrl Pts',(-3.26899943869611,2.44966684873771,-32.2424864015253));
#28320=CARTESIAN_POINT('Ctrl Pts',(-3.19731667796541,2.54532512354091,-32.2482938562724));
#28321=CARTESIAN_POINT('Ctrl Pts',(-3.12145993202294,2.6377967145576,-32.2541013110195));
#28322=CARTESIAN_POINT('Ctrl Pts',(-3.04175490922273,2.72671085233095,-32.2599087657666));
#28323=CARTESIAN_POINT('Ctrl Pts',(-2.9619620319989,2.81572299522433,-32.2657226217488));
#28324=CARTESIAN_POINT('Ctrl Pts',(-2.8783126837044,2.9011695540318,-32.271536477731));
#28325=CARTESIAN_POINT('Ctrl Pts',(-2.79116997494235,2.98271607280685,-32.2773503337132));
#28326=CARTESIAN_POINT('Ctrl Pts',(-2.70396993292371,3.06431624297226,-32.2831680147693));
#28327=CARTESIAN_POINT('Ctrl Pts',(-2.61327226225792,3.1420109980932,-32.2889856958253));
#28328=CARTESIAN_POINT('Ctrl Pts',(-2.51947244850089,3.2155067378634,-32.2948033768814));
#28329=CARTESIAN_POINT('Ctrl Pts',(-2.4255397207676,3.28910662081492,-32.3006293015692));
#28330=CARTESIAN_POINT('Ctrl Pts',(-2.32849640733948,3.35849537657707,-32.306455226257));
#28331=CARTESIAN_POINT('Ctrl Pts',(-2.22876626902628,3.42342312869016,-32.3122811509447));
#28332=CARTESIAN_POINT('Ctrl Pts',(-2.20515487815661,3.43879495669882,-32.3136604550078));
#28333=CARTESIAN_POINT('Ctrl Pts',(-2.18139298917573,3.45391694238073,-32.3150397590708));
#28334=CARTESIAN_POINT('Ctrl Pts',(-2.15748640892605,3.46878615589076,-32.3164190631338));
#28335=CARTESIAN_POINT('Ctrl Pts',(-2.05651765328459,3.53158585245109,-32.3222445142623));
#28336=CARTESIAN_POINT('Ctrl Pts',(-1.9526431612848,3.59007388439192,-32.3280699653908));
#28337=CARTESIAN_POINT('Ctrl Pts',(-1.84626682834135,3.64397088333131,-32.3338954165193));
#28338=CARTESIAN_POINT('Ctrl Pts',(-1.74002401548954,3.69780023252157,-32.3397135557322));
#28339=CARTESIAN_POINT('Ctrl Pts',(-1.63128596846802,3.74704982764663,-32.3455316949451));
#28340=CARTESIAN_POINT('Ctrl Pts',(-1.52048469664809,3.79148404813458,-32.351349834158));
#28341=CARTESIAN_POINT('Ctrl Pts',(-1.409793676198,3.83587405492718,-32.3571621841068));
#28342=CARTESIAN_POINT('Ctrl Pts',(-1.29704389175103,3.87545806832089,-32.3629745340557));
#28343=CARTESIAN_POINT('Ctrl Pts',(-1.18269050645048,3.91004707976156,-32.3687868840046));
#28344=CARTESIAN_POINT('Ctrl Pts',(-1.06447467210484,3.94580438450512,-32.3747955543811));
#28345=CARTESIAN_POINT('Ctrl Pts',(-0.944545387756902,3.97622308711449,
-32.3808042247577));
#28346=CARTESIAN_POINT('Ctrl Pts',(-0.823426741796678,4.00114901008374,
-32.3868128951342));
#28347=CARTESIAN_POINT('Ctrl Pts',(-0.706395883563465,4.02523367627382,
-32.3926187712273));
#28348=CARTESIAN_POINT('Ctrl Pts',(-0.588255082315933,4.04419025689563,
-32.3984246473204));
#28349=CARTESIAN_POINT('Ctrl Pts',(-0.469490321672897,4.05793097992751,
-32.4042305234135));
#28350=CARTESIAN_POINT('Ctrl Pts',(-0.350742769693217,4.07166971196918,
-32.4100355582522));
#28351=CARTESIAN_POINT('Ctrl Pts',(-0.231371843327783,4.08019404256848,
-32.415840593091));
#28352=CARTESIAN_POINT('Ctrl Pts',(-0.111870224996192,4.08346789539961,
-32.4216456279298));
#28353=CARTESIAN_POINT('Ctrl Pts',(0.00764222554980037,4.08674204498885,
-32.4274511889655));
#28354=CARTESIAN_POINT('Ctrl Pts',(0.127284983734767,4.08476475937415,-32.4332567500012));
#28355=CARTESIAN_POINT('Ctrl Pts',(0.246564419532909,4.07755208268642,-32.4390623110368));
#28356=CARTESIAN_POINT('Ctrl Pts',(0.365882762502919,4.0703370533312,-32.4448697657599));
#28357=CARTESIAN_POINT('Ctrl Pts',(0.484837140335601,4.0578832612336,-32.4506772204829));
#28358=CARTESIAN_POINT('Ctrl Pts',(0.602938737191007,4.04025864013611,-32.456484675206));
#28359=CARTESIAN_POINT('Ctrl Pts',(0.721170510883805,4.02261459239669,-32.4622985311642));
#28360=CARTESIAN_POINT('Ctrl Pts',(0.838547223601299,3.99978839941529,-32.4681123871223));
#28361=CARTESIAN_POINT('Ctrl Pts',(0.954589798932851,3.97189920765537,-32.4739262430805));
#28362=CARTESIAN_POINT('Ctrl Pts',(1.07070872142917,3.94399166693419,-32.4797439241125));
#28363=CARTESIAN_POINT('Ctrl Pts',(1.18549136719503,3.9110146058307,-32.4855616051445));
#28364=CARTESIAN_POINT('Ctrl Pts',(1.29847495825567,3.87313668526983,-32.4913792861765));
#28365=CARTESIAN_POINT('Ctrl Pts',(1.41161864663505,3.83520509183961,-32.4972052108404));
#28366=CARTESIAN_POINT('Ctrl Pts',(1.52295781293906,3.7923589246507,-32.5030311355043));
#28367=CARTESIAN_POINT('Ctrl Pts',(1.63205062850394,3.74481451423163,-32.5088570601682));
#28368=CARTESIAN_POINT('Ctrl Pts',(1.65787866393587,3.73355823937489,-32.5102363644594));
#28369=CARTESIAN_POINT('Ctrl Pts',(1.68358090163677,3.72203881844289,-32.5116156687505));
#28370=CARTESIAN_POINT('Ctrl Pts',(1.7091516998568,3.71025948780899,-32.5129949730417));
#28371=CARTESIAN_POINT('Ctrl Pts',(1.81715610775104,3.66050665570897,-32.5188207959976));
#28372=CARTESIAN_POINT('Ctrl Pts',(1.92315906681105,3.60595435836731,-32.5246466189536));
#28373=CARTESIAN_POINT('Ctrl Pts',(2.02670496799447,3.54678614702191,-32.5304724419095));
#28374=CARTESIAN_POINT('Ctrl Pts',(2.13010585702929,3.48770079853596,-32.5362901060191));
#28375=CARTESIAN_POINT('Ctrl Pts',(2.23105618476815,3.424012601285,-32.5421077701286));
#28376=CARTESIAN_POINT('Ctrl Pts',(2.32912159384625,3.3559525624,-32.5479254342381));
#28377=CARTESIAN_POINT('Ctrl Pts',(2.38264847979213,3.31880345984571,-32.5511008805672));
#28378=CARTESIAN_POINT('Ctrl Pts',(2.43531623718868,3.2803526898498,-32.5542763268962));
#28379=CARTESIAN_POINT('Ctrl Pts',(2.48705727606861,3.24064362520074,-32.5574517732253));
#28380=CARTESIAN_POINT('',(-4.08499951611116,-0.00198830873281907,-32.010384971366));
#28381=CARTESIAN_POINT('Ctrl Pts',(-4.08499951611154,-0.00198830793933937,
-32.0103849714045));
#28382=CARTESIAN_POINT('Ctrl Pts',(-4.08505857983268,0.119358726635596,
-32.0162687995861));
#28383=CARTESIAN_POINT('Ctrl Pts',(-4.07970628193321,0.240701121345341,
-32.0221526277676));
#28384=CARTESIAN_POINT('Ctrl Pts',(-4.06897033272945,0.361532061327329,
-32.0280364559492));
#28385=CARTESIAN_POINT('Ctrl Pts',(-4.05823134250943,0.482397227333078,
-32.0339219507573));
#28386=CARTESIAN_POINT('Ctrl Pts',(-4.0421056992771,0.602750259327652,-32.0398074455653));
#28387=CARTESIAN_POINT('Ctrl Pts',(-4.02067294073167,0.72209009387204,-32.0456929403733));
#28388=CARTESIAN_POINT('Ctrl Pts',(-3.99922962856903,0.84148869205761,-32.0515813332339));
#28389=CARTESIAN_POINT('Ctrl Pts',(-3.97247406722256,0.959872713557851,
-32.0574697260944));
#28390=CARTESIAN_POINT('Ctrl Pts',(-3.94053669152283,1.07675233120822,-32.0633581189549));
#28391=CARTESIAN_POINT('Ctrl Pts',(-3.90855498480322,1.19379418487639,-32.0692546852629));
#28392=CARTESIAN_POINT('Ctrl Pts',(-3.87137720107183,1.3093270849135,-32.0751512515708));
#28393=CARTESIAN_POINT('Ctrl Pts',(-3.82918353551356,1.42287682226955,-32.0810478178788));
#28394=CARTESIAN_POINT('Ctrl Pts',(-3.78695819284858,1.53651180766219,-32.0869488110635));
#28395=CARTESIAN_POINT('Ctrl Pts',(-3.73970961600701,1.64816030227053,-32.0928498042483));
#28396=CARTESIAN_POINT('Ctrl Pts',(-3.68766529048739,1.75737011051586,-32.098750797433));
#28397=CARTESIAN_POINT('Ctrl Pts',(-3.63552985940311,1.86677109467034,-32.1046621205301));
#28398=CARTESIAN_POINT('Ctrl Pts',(-3.57858209089098,1.9737245171403,-32.1105734436271));
#28399=CARTESIAN_POINT('Ctrl Pts',(-3.51709471612082,2.07780407108924,-32.1164847667241));
#28400=CARTESIAN_POINT('Ctrl Pts',(-3.47684270541128,2.14593856757502,-32.1203545471709));
#28401=CARTESIAN_POINT('Ctrl Pts',(-3.43464613454845,2.21284205347598,-32.1242243276177));
#28402=CARTESIAN_POINT('Ctrl Pts',(-3.39059098493886,2.27840246068409,-32.1280941080644));
#28403=CARTESIAN_POINT('Ctrl Pts',(-3.32427168755066,2.37709512615128,-32.1339195591763));
#28404=CARTESIAN_POINT('Ctrl Pts',(-3.25353363423184,2.47304765452436,-32.1397450102882));
#28405=CARTESIAN_POINT('Ctrl Pts',(-3.17863056473336,2.56583957661871,-32.1455704614));
#28406=CARTESIAN_POINT('Ctrl Pts',(-3.10382151111628,2.65851502932935,-32.1513886005963));
#28407=CARTESIAN_POINT('Ctrl Pts',(-3.02485809354326,2.74803745164358,-32.1572067397926));
#28408=CARTESIAN_POINT('Ctrl Pts',(-2.94203763787773,2.8340147383722,-32.1630248789889));
#28409=CARTESIAN_POINT('Ctrl Pts',(-2.85929959163333,2.91990647451585,-32.1688372289212));
#28410=CARTESIAN_POINT('Ctrl Pts',(-2.77271242393837,3.00225980063408,-32.1746495788534));
#28411=CARTESIAN_POINT('Ctrl Pts',(-2.68261369815691,3.08071562245867,-32.1804619287857));
#28412=CARTESIAN_POINT('Ctrl Pts',(-2.58947175876295,3.16182140212545,-32.1864705991685));
#28413=CARTESIAN_POINT('Ctrl Pts',(-2.492577125476,3.23876138386672,-32.1924792695512));
#28414=CARTESIAN_POINT('Ctrl Pts',(-2.39234450899972,3.31117996343582,-32.198487939934));
#28415=CARTESIAN_POINT('Ctrl Pts',(-2.29549477136494,3.38115439568874,-32.2042938160107));
#28416=CARTESIAN_POINT('Ctrl Pts',(-2.19552908759903,3.44690744019488,-32.2100996920874));
#28417=CARTESIAN_POINT('Ctrl Pts',(-2.09285465911595,3.50815968505093,-32.2159055681641));
#28418=CARTESIAN_POINT('Ctrl Pts',(-1.99019510785271,3.56940305463857,-32.2217106029866));
#28419=CARTESIAN_POINT('Ctrl Pts',(-1.88482794274692,3.62614671256697,-32.2275156378091));
#28420=CARTESIAN_POINT('Ctrl Pts',(-1.7771876815604,3.67815564441065,-32.2333206726316));
#28421=CARTESIAN_POINT('Ctrl Pts',(-1.66953766332881,3.73016929060087,-32.2391262336512));
#28422=CARTESIAN_POINT('Ctrl Pts',(-1.5596145067462,3.77744717987937,-32.2449317946707));
#28423=CARTESIAN_POINT('Ctrl Pts',(-1.44787497518768,3.81980144198953,-32.2507373556902));
#28424=CARTESIAN_POINT('Ctrl Pts',(-1.33609899585901,3.86216951942886,-32.2565448103973));
#28425=CARTESIAN_POINT('Ctrl Pts',(-1.22250584456867,3.89961063112266,-32.2623522651043));
#28426=CARTESIAN_POINT('Ctrl Pts',(-1.10756918095594,3.93198620412084,-32.2681597198113));
#28427=CARTESIAN_POINT('Ctrl Pts',(-0.99250582902963,3.96439746291862,-32.2739735757538));
#28428=CARTESIAN_POINT('Ctrl Pts',(-0.876096401827009,3.99173192748857,
-32.2797874316963));
#28429=CARTESIAN_POINT('Ctrl Pts',(-0.758826685837961,4.01390172536152,
-32.2856012876387));
#28430=CARTESIAN_POINT('Ctrl Pts',(-0.641479815316192,4.03608610927128,
-32.2914189686552));
#28431=CARTESIAN_POINT('Ctrl Pts',(-0.523271931688789,4.0530990012752,-32.2972366496716));
#28432=CARTESIAN_POINT('Ctrl Pts',(-0.404694269923536,4.0649043713095,-32.303054330688));
#28433=CARTESIAN_POINT('Ctrl Pts',(-0.285948584055017,4.07672646950898,
-32.3088802553367));
#28434=CARTESIAN_POINT('Ctrl Pts',(-0.166832480162451,4.08332629566224,
-32.3147061799854));
#28435=CARTESIAN_POINT('Ctrl Pts',(-0.0478376433608585,4.08471988756606,
-32.3205321046341));
#28436=CARTESIAN_POINT('Ctrl Pts',(-0.0196652729037597,4.08504982446446,
-32.3219114090801));
#28437=CARTESIAN_POINT('Ctrl Pts',(0.00850032292552177,4.08508817077907,
-32.3232907135262));
#28438=CARTESIAN_POINT('Ctrl Pts',(0.0366526712919777,4.08483556360439,
-32.3246700179722));
#28439=CARTESIAN_POINT('Ctrl Pts',(0.155532688907448,4.08376886945208,-32.3304944605626));
#28440=CARTESIAN_POINT('Ctrl Pts',(0.274556241674694,4.0775065597022,-32.3363189031529));
#28441=CARTESIAN_POINT('Ctrl Pts',(0.393232873428394,4.06602913261271,-32.3421433457433));
#28442=CARTESIAN_POINT('Ctrl Pts',(0.511770058277997,4.0545651916801,-32.3479609445222));
#28443=CARTESIAN_POINT('Ctrl Pts',(0.629960730346802,4.03789835645692,-32.3537785433011));
#28444=CARTESIAN_POINT('Ctrl Pts',(0.747314013723899,4.01606110074185,-32.35959614208));
#28445=CARTESIAN_POINT('Ctrl Pts',(0.864557058872457,3.9942443583036,-32.3654082759775));
#28446=CARTESIAN_POINT('Ctrl Pts',(0.98096388104933,3.96726692908919,-32.371220409875));
#28447=CARTESIAN_POINT('Ctrl Pts',(1.09604894154684,3.93521304604135,-32.3770325437724));
#28448=CARTESIAN_POINT('Ctrl Pts',(1.21105300878,3.90318172151337,-32.3828405872719));
#28449=CARTESIAN_POINT('Ctrl Pts',(1.32473677325709,3.86608115981677,-32.3886486307714));
#28450=CARTESIAN_POINT('Ctrl Pts',(1.43662573038736,3.82404648386875,-32.3944566742709));
#28451=CARTESIAN_POINT('Ctrl Pts',(1.54847062998495,3.78202835954618,-32.4002624307881));
#28452=CARTESIAN_POINT('Ctrl Pts',(1.65852174623152,3.73508012760712,-32.4060681873053));
#28453=CARTESIAN_POINT('Ctrl Pts',(1.76632106908059,3.68338633337884,-32.4118739438224));
#28454=CARTESIAN_POINT('Ctrl Pts',(1.87409602925729,3.63170422196024,-32.4176783882373));
#28455=CARTESIAN_POINT('Ctrl Pts',(1.97961984251812,3.57527886181049,-32.4234828326521));
#28456=CARTESIAN_POINT('Ctrl Pts',(2.08245644740712,3.5143420642636,-32.4292872770669));
#28457=CARTESIAN_POINT('Ctrl Pts',(2.18531388380867,3.45339292280799,-32.4350928972825));
#28458=CARTESIAN_POINT('Ctrl Pts',(2.28548267412948,3.38793072753696,-32.4408985174981));
#28459=CARTESIAN_POINT('Ctrl Pts',(2.38255355088111,3.31823199568442,-32.4467041377137));
#28460=CARTESIAN_POINT('Ctrl Pts',(2.41780252834394,3.29292256086244,-32.4488123104529));
#28461=CARTESIAN_POINT('Ctrl Pts',(2.45264329664656,3.2670549026564,-32.4509204831921));
#28462=CARTESIAN_POINT('Ctrl Pts',(2.48705727606859,3.24064362520075,-32.4530286559312));
#28463=CARTESIAN_POINT('Ctrl Pts',(2.48705727606859,3.24064362520075,-31.2032093449099));
#28464=CARTESIAN_POINT('Ctrl Pts',(2.58179338776476,3.16793765590868,-31.209016651121));
#28465=CARTESIAN_POINT('Ctrl Pts',(2.67340003593691,3.09102689829715,-31.2148239573321));
#28466=CARTESIAN_POINT('Ctrl Pts',(2.76148917095052,3.01021636410458,-31.2206312635432));
#28467=CARTESIAN_POINT('Ctrl Pts',(2.84955077592288,2.92943108520984,-31.2264367548269));
#28468=CARTESIAN_POINT('Ctrl Pts',(2.93409675328447,2.84474872873737,-31.2322422461106));
#28469=CARTESIAN_POINT('Ctrl Pts',(3.01477311734607,2.75651374945373,-31.2380477373943));
#28470=CARTESIAN_POINT('Ctrl Pts',(3.09544327087232,2.66828556257409,-31.2438527817664));
#28471=CARTESIAN_POINT('Ctrl Pts',(3.17224412831572,2.57650559795978,-31.2496578261384));
#28472=CARTESIAN_POINT('Ctrl Pts',(3.24485992657571,2.48155375861638,-31.2554628705105));
#28473=CARTESIAN_POINT('Ctrl Pts',(3.31748723886432,2.38658686362088,-31.2612688353358));
#28474=CARTESIAN_POINT('Ctrl Pts',(3.38592792457097,2.28844741789956,-31.2670748001611));
#28475=CARTESIAN_POINT('Ctrl Pts',(3.44990812167822,2.18754633139019,-31.2728807649864));
#28476=CARTESIAN_POINT('Ctrl Pts',(3.51395352814054,2.08654240532928,-31.278692647318));
#28477=CARTESIAN_POINT('Ctrl Pts',(3.57352914577614,1.98277156114108,-31.2845045296497));
#28478=CARTESIAN_POINT('Ctrl Pts',(3.62840574929162,1.87667171303548,-31.2903164119813));
#28479=CARTESIAN_POINT('Ctrl Pts',(3.68331020688576,1.77051801113196,-31.2961312442883));
#28480=CARTESIAN_POINT('Ctrl Pts',(3.73351072648581,1.66203332015816,-31.3019460765953));
#28481=CARTESIAN_POINT('Ctrl Pts',(3.77882589874646,1.55167645692102,-31.3077609089023));
#28482=CARTESIAN_POINT('Ctrl Pts',(3.82421427666205,1.44114131462091,-31.3135851349418));
#28483=CARTESIAN_POINT('Ctrl Pts',(3.86470139769733,1.32872834058064,-31.3194093609813));
#28484=CARTESIAN_POINT('Ctrl Pts',(3.90015528637214,1.2149130595164,-31.3252335870208));
#28485=CARTESIAN_POINT('Ctrl Pts',(3.93375092788814,1.10706318677746,-31.3307525474915));
#28486=CARTESIAN_POINT('Ctrl Pts',(3.96282747733818,0.99795455533443,-31.3362715079623));
#28487=CARTESIAN_POINT('Ctrl Pts',(3.9873152681288,0.887998847154075,-31.3417904684331));
#28488=CARTESIAN_POINT('Ctrl Pts',(4.01316297123626,0.771936825703536,-31.3476159205096));
#28489=CARTESIAN_POINT('Ctrl Pts',(4.03398035212741,0.654559649078143,-31.3534413725861));
#28490=CARTESIAN_POINT('Ctrl Pts',(4.04963744446642,0.536340906863787,-31.3592668246626));
#28491=CARTESIAN_POINT('Ctrl Pts',(4.06527488456825,0.418270548698773,-31.3650849648345));
#28492=CARTESIAN_POINT('Ctrl Pts',(4.07576486590849,0.299361126921743,-31.3709031050064));
#28493=CARTESIAN_POINT('Ctrl Pts',(4.08102800875816,0.180098283532682,-31.3767212451783));
#28494=CARTESIAN_POINT('Ctrl Pts',(4.08628591459541,0.0609541108712847,
-31.3825335960959));
#28495=CARTESIAN_POINT('Ctrl Pts',(4.08632731079461,-0.0585423784766985,
-31.3883459470134));
#28496=CARTESIAN_POINT('Ctrl Pts',(4.08112446558333,-0.177899118652157,
-31.394158297931));
#28497=CARTESIAN_POINT('Ctrl Pts',(4.0757458880563,-0.30128727538888,-31.4001669679481));
#28498=CARTESIAN_POINT('Ctrl Pts',(4.06476247903152,-0.424525635170655,
-31.4061756379652));
#28499=CARTESIAN_POINT('Ctrl Pts',(4.04820218464763,-0.547068617464195,
-31.4121843079823));
#28500=CARTESIAN_POINT('Ctrl Pts',(4.03220080109268,-0.665475767493723,
-31.4179901850621));
#28501=CARTESIAN_POINT('Ctrl Pts',(4.01099295722774,-0.783233284119383,
-31.4237960621419));
#28502=CARTESIAN_POINT('Ctrl Pts',(3.98465665307939,-0.899853519785383,
-31.4296019392217));
#28503=CARTESIAN_POINT('Ctrl Pts',(3.95832416496072,-1.01645685762555,-31.4354069750522));
#28504=CARTESIAN_POINT('Ctrl Pts',(3.92686478424874,-1.13192284433952,-31.4412120108826));
#28505=CARTESIAN_POINT('Ctrl Pts',(3.89040751072223,-1.24577461866745,-31.4470170467131));
#28506=CARTESIAN_POINT('Ctrl Pts',(3.85394693250546,-1.35963671315413,-31.4528226087443));
#28507=CARTESIAN_POINT('Ctrl Pts',(3.81248768516331,-1.47188391573622,-31.4586281707755));
#28508=CARTESIAN_POINT('Ctrl Pts',(3.76620826581264,-1.58205571915927,-31.4644337328067));
#28509=CARTESIAN_POINT('Ctrl Pts',(3.71991375078668,-1.69226345902648,-31.470241188528));
#28510=CARTESIAN_POINT('Ctrl Pts',(3.66879609475868,-1.80039407741151,-31.4760486442494));
#28511=CARTESIAN_POINT('Ctrl Pts',(3.61308116759669,-1.90600878181559,-31.4818560999707));
#28512=CARTESIAN_POINT('Ctrl Pts',(3.55730482898067,-2.01173989941258,-31.4876699569263));
#28513=CARTESIAN_POINT('Ctrl Pts',(3.4969212951177,-2.11494920661366,-31.4934838138819));
#28514=CARTESIAN_POINT('Ctrl Pts',(3.43220153996603,-2.21522404940331,-31.4992976708375));
#28515=CARTESIAN_POINT('Ctrl Pts',(3.36743920415105,-2.31556486539249,-31.5051153528676));
#28516=CARTESIAN_POINT('Ctrl Pts',(3.29833520087221,-2.41296703997161,-31.5109330348977));
#28517=CARTESIAN_POINT('Ctrl Pts',(3.2252018350368,-2.50704968504321,-31.5167507169277));
#28518=CARTESIAN_POINT('Ctrl Pts',(3.15196483960127,-2.60126564473496,-31.5225766425831));
#28519=CARTESIAN_POINT('Ctrl Pts',(3.07468734935894,-2.69215237714021,-31.5284025682385));
#28520=CARTESIAN_POINT('Ctrl Pts',(2.99371972014326,-2.7793645383838,-31.5342284938938));
#28521=CARTESIAN_POINT('Ctrl Pts',(2.97455053779819,-2.80001212110025,-31.5356077887095));
#28522=CARTESIAN_POINT('Ctrl Pts',(2.95517466932275,-2.82045391404605,-31.5369870835252));
#28523=CARTESIAN_POINT('Ctrl Pts',(2.93559703565821,-2.84068566445404,-31.5383663783409));
#28524=CARTESIAN_POINT('Ctrl Pts',(2.85291090821357,-2.92613445368613,-31.5441918294076));
#28525=CARTESIAN_POINT('Ctrl Pts',(2.76635857277787,-3.00810672305135,-31.5500172804743));
#28526=CARTESIAN_POINT('Ctrl Pts',(2.67626394974318,-3.08623334686557,-31.555842731541));
#28527=CARTESIAN_POINT('Ctrl Pts',(2.58628241051181,-3.16426190871488,-31.5616608706934));
#28528=CARTESIAN_POINT('Ctrl Pts',(2.49276773275701,-3.23845416086974,-31.5674790098458));
#28529=CARTESIAN_POINT('Ctrl Pts',(2.39608173715407,-3.30847658430232,-31.5732971489982));
#28530=CARTESIAN_POINT('Ctrl Pts',(2.2994919476763,-3.37842933284566,-31.5791094988879));
#28531=CARTESIAN_POINT('Ctrl Pts',(2.19973744669917,-3.44422026905515,-31.5849218487777));
#28532=CARTESIAN_POINT('Ctrl Pts',(2.09721383948261,-3.50555546404312,-31.5907341986674));
#28533=CARTESIAN_POINT('Ctrl Pts',(1.99122734940714,-3.56896234379852,-31.5967428690666));
#28534=CARTESIAN_POINT('Ctrl Pts',(1.88228171634488,-3.6276068652051,-31.6027515394658));
#28535=CARTESIAN_POINT('Ctrl Pts',(1.77084786800124,-3.68121214118331,-31.6087602098651));
#28536=CARTESIAN_POINT('Ctrl Pts',(1.6631749442234,-3.73300822361506,-31.6145660859029));
#28537=CARTESIAN_POINT('Ctrl Pts',(1.55317944793754,-3.7800995328266,-31.6203719619407));
#28538=CARTESIAN_POINT('Ctrl Pts',(1.44131147719164,-3.82228285527323,-31.6261778379786));
#28539=CARTESIAN_POINT('Ctrl Pts',(1.32945971575516,-3.86446006549201,-31.6319828727636));
#28540=CARTESIAN_POINT('Ctrl Pts',(1.21573640111529,-3.90173055933158,-31.6377879075487));
#28541=CARTESIAN_POINT('Ctrl Pts',(1.10061068905402,-3.93393964253902,-31.6435929423337));
#28542=CARTESIAN_POINT('Ctrl Pts',(0.985474541399795,-3.96615164534518,
-31.6493985033173));
#28543=CARTESIAN_POINT('Ctrl Pts',(0.868936136523122,-3.99330121539376,
-31.6552040643009));
#28544=CARTESIAN_POINT('Ctrl Pts',(0.751478212259808,-4.01528398702991,
-31.6610096252845));
#28545=CARTESIAN_POINT('Ctrl Pts',(0.633981974941117,-4.03727392912434,
-31.6668170799571));
#28546=CARTESIAN_POINT('Ctrl Pts',(0.515566022569239,-4.05409364599779,
-31.6726245346297));
#28547=CARTESIAN_POINT('Ctrl Pts',(0.396721029792019,-4.06569027651157,
-31.6784319893022));
#28548=CARTESIAN_POINT('Ctrl Pts',(0.277745040715636,-4.07729968935337,
-31.6842458452127));
#28549=CARTESIAN_POINT('Ctrl Pts',(0.158339473599013,-4.08367448471301,
-31.6900597011232));
#28550=CARTESIAN_POINT('Ctrl Pts',(0.0389979977760629,-4.08481384596281,
-31.6958735570336));
#28551=CARTESIAN_POINT('Ctrl Pts',(-0.0804219956687229,-4.08595395682572,
-31.7016912380195));
#28552=CARTESIAN_POINT('Ctrl Pts',(-0.199777407019994,-4.0818517876119,
-31.7075089190053));
#28553=CARTESIAN_POINT('Ctrl Pts',(-0.318578347341432,-4.07255851236114,
-31.7133265999911));
#28554=CARTESIAN_POINT('Ctrl Pts',(-0.437547628198452,-4.06325206857039,
-31.7191525246115));
#28555=CARTESIAN_POINT('Ctrl Pts',(-0.555960466404257,-4.04873988702924,
-31.7249784492319));
#28556=CARTESIAN_POINT('Ctrl Pts',(-0.673335713159881,-4.02912447280839,
-31.7308043738522));
#28557=CARTESIAN_POINT('Ctrl Pts',(-0.701124648250158,-4.02448046576585,
-31.7321836786511));
#28558=CARTESIAN_POINT('Ctrl Pts',(-0.728855486948905,-4.01955063384845,
-31.7335629834499));
#28559=CARTESIAN_POINT('Ctrl Pts',(-0.756521970249876,-4.01433674578121,
-31.7349422882488));
#28560=CARTESIAN_POINT('Ctrl Pts',(-0.873370502116339,-3.99231605166746,
-31.7407677391739));
#28561=CARTESIAN_POINT('Ctrl Pts',(-0.989443698158363,-3.96515409256765,
-31.7465931900991));
#28562=CARTESIAN_POINT('Ctrl Pts',(-1.1042550989485,-3.93291821380082,-31.7524186410243));
#28563=CARTESIAN_POINT('Ctrl Pts',(-1.21892239215086,-3.90072279647508,
-31.7582367800303));
#28564=CARTESIAN_POINT('Ctrl Pts',(-1.33233065082415,-3.86346623611826,
-31.7640549190363));
#28565=CARTESIAN_POINT('Ctrl Pts',(-1.44400229069796,-3.82126711765339,
-31.7698730580423));
#28566=CARTESIAN_POINT('Ctrl Pts',(-1.55556281308672,-3.77910998889978,
-31.775685407781));
#28567=CARTESIAN_POINT('Ctrl Pts',(-1.66538977487724,-3.7320202294698,-31.7814977575197));
#28568=CARTESIAN_POINT('Ctrl Pts',(-1.77302005787152,-3.68016641938721,
-31.7873101072584));
#28569=CARTESIAN_POINT('Ctrl Pts',(-1.88428571297945,-3.62656117011932,
-31.7933187777125));
#28570=CARTESIAN_POINT('Ctrl Pts',(-1.99320324284419,-3.56786446788854,
-31.7993274481666));
#28571=CARTESIAN_POINT('Ctrl Pts',(-2.09928231045757,-3.50431716330014,
-31.8053361186207));
#28572=CARTESIAN_POINT('Ctrl Pts',(-2.20178117511103,-3.44291460086588,
-31.8111419944968));
#28573=CARTESIAN_POINT('Ctrl Pts',(-2.30162970595371,-3.37698379793955,
-31.816947870373));
#28574=CARTESIAN_POINT('Ctrl Pts',(-2.39841054414801,-3.30678875371858,
-31.8227537462491));
#28575=CARTESIAN_POINT('Ctrl Pts',(-2.49517735904853,-3.23660388057842,
-31.8285587808688));
#28576=CARTESIAN_POINT('Ctrl Pts',(-2.58887703510446,-3.16215623444704,
-31.8343638154885));
#28577=CARTESIAN_POINT('Ctrl Pts',(-2.67912223909719,-3.0837524265049,-31.8401688501082));
#28578=CARTESIAN_POINT('Ctrl Pts',(-2.76937562332888,-3.00534151168222,
-31.8459744109229));
#28579=CARTESIAN_POINT('Ctrl Pts',(-2.85617360489777,-2.92297398966321,
-31.8517799717376));
#28580=CARTESIAN_POINT('Ctrl Pts',(-2.93916340009146,-2.83699550714534,
-31.8575855325522));
#28581=CARTESIAN_POINT('Ctrl Pts',(-3.02218026529552,-2.75098897975269,
-31.8633929870526));
#28582=CARTESIAN_POINT('Ctrl Pts',(-3.10138619047977,-2.66136944278746,
-31.869200441553));
#28583=CARTESIAN_POINT('Ctrl Pts',(-3.17646702976446,-2.56851751187711,
-31.8750078960534));
#28584=CARTESIAN_POINT('Ctrl Pts',(-3.25163062647782,-2.47556323545327,
-31.8808217517875));
#28585=CARTESIAN_POINT('Ctrl Pts',(-3.32265980487839,-2.37936977084228,
-31.8866356075217));
#28586=CARTESIAN_POINT('Ctrl Pts',(-3.38928222735186,-2.28034887316762,
-31.8924494632558));
#28587=CARTESIAN_POINT('Ctrl Pts',(-3.45594848228769,-2.18126282730998,
-31.8982671440627));
#28588=CARTESIAN_POINT('Ctrl Pts',(-3.51820199497138,-2.07934599100962,
-31.9040848248696));
#28589=CARTESIAN_POINT('Ctrl Pts',(-3.57581591928054,-1.975035572191,-31.9099025056765));
#28590=CARTESIAN_POINT('Ctrl Pts',(-3.63351148230604,-1.8705773458971,-31.9157284301154));
#28591=CARTESIAN_POINT('Ctrl Pts',(-3.68655415481689,-1.76371913183232,
-31.9215543545543));
#28592=CARTESIAN_POINT('Ctrl Pts',(-3.7347647606383,-1.65491908644935,-31.9273802789933));
#28593=CARTESIAN_POINT('Ctrl Pts',(-3.74617877694831,-1.62916032504463,
-31.928759585381));
#28594=CARTESIAN_POINT('Ctrl Pts',(-3.7573221650775,-1.60329278941273,-31.9301388917688));
#28595=CARTESIAN_POINT('Ctrl Pts',(-3.76819295767263,-1.57732267901859,
-31.9315181981565));
#28596=CARTESIAN_POINT('Ctrl Pts',(-3.8199909931333,-1.4535781877737,-31.9380904292573));
#28597=CARTESIAN_POINT('Ctrl Pts',(-3.86573903894072,-1.3271614817197,-31.9446626603581));
#28598=CARTESIAN_POINT('Ctrl Pts',(-3.90518392162653,-1.19865071570898,
-31.9512348914589));
#28599=CARTESIAN_POINT('Ctrl Pts',(-3.94380032604224,-1.07283911800259,
-31.9576690830909));
#28600=CARTESIAN_POINT('Ctrl Pts',(-3.97637557280735,-0.945020799958586,
-31.9641032747229));
#28601=CARTESIAN_POINT('Ctrl Pts',(-4.00271890358611,-0.815761226630919,
-31.9705374663549));
#28602=CARTESIAN_POINT('Ctrl Pts',(-4.02990999106734,-0.682341941284823,
-31.97717871719));
#28603=CARTESIAN_POINT('Ctrl Pts',(-4.05046116507769,-0.547387282983328,
-31.9838199680252));
#28604=CARTESIAN_POINT('Ctrl Pts',(-4.06421691951732,-0.411540801269059,
-31.9904612188604));
#28605=CARTESIAN_POINT('Ctrl Pts',(-4.07797267395695,-0.275694319554789,
-31.9971024696956));
#28606=CARTESIAN_POINT('Ctrl Pts',(-4.08493284911617,-0.138956294514414,
-32.0037437205308));
#28607=CARTESIAN_POINT('Ctrl Pts',(-4.08499951611116,-0.00198830873280959,
-32.010384971366));
#28608=CARTESIAN_POINT('Origin',(0.,0.,-25.2396150285955));
#28609=CARTESIAN_POINT('',(2.4870572760686,3.24064362520075,-29.953048263356));
#28610=CARTESIAN_POINT('',(2.48705727606859,3.24064362520075,-30.0573351590495));
#28611=CARTESIAN_POINT('',(2.4870572760686,3.24064362520075,-25.2396150285955));
#28612=CARTESIAN_POINT('',(-4.08499937550907,0.002258780766463,-30.8646150286367));
#28613=CARTESIAN_POINT('Ctrl Pts',(2.48705727606859,3.24064362520075,-30.0573351590495));
#28614=CARTESIAN_POINT('Ctrl Pts',(2.5819015155267,3.16785467241275,-30.0631404188983));
#28615=CARTESIAN_POINT('Ctrl Pts',(2.67354511593237,3.09090048087354,-30.0689456787472));
#28616=CARTESIAN_POINT('Ctrl Pts',(2.76161314187302,3.01010263191045,-30.074750938596));
#28617=CARTESIAN_POINT('Ctrl Pts',(2.8497034648523,2.92928432657014,-30.0805576682189));
#28618=CARTESIAN_POINT('Ctrl Pts',(2.93421611250136,2.84462070430025,-30.0863643978418));
#28619=CARTESIAN_POINT('Ctrl Pts',(3.0148123336213,2.75647085837034,-30.0921711274647));
#28620=CARTESIAN_POINT('Ctrl Pts',(3.09549460057924,2.66822690222957,-30.0979840564467));
#28621=CARTESIAN_POINT('Ctrl Pts',(3.17225181671804,2.57648959232832,-30.1037969854287));
#28622=CARTESIAN_POINT('Ctrl Pts',(3.24478480929274,2.48165197829653,-30.1096099144107));
#28623=CARTESIAN_POINT('Ctrl Pts',(3.31736077328321,2.38675817870836,-30.1154262872019));
#28624=CARTESIAN_POINT('Ctrl Pts',(3.38570729559298,2.28876075060164,-30.1212426599931));
#28625=CARTESIAN_POINT('Ctrl Pts',(3.44956888102454,2.18808124507915,-30.1270590327844));
#28626=CARTESIAN_POINT('Ctrl Pts',(3.51352628694766,2.08725067597682,-30.1328841326953));
#28627=CARTESIAN_POINT('Ctrl Pts',(3.57298511452915,1.98373034625041,-30.1387092326062));
#28628=CARTESIAN_POINT('Ctrl Pts',(3.62773594424741,1.877966165514,-30.1445343325171));
#28629=CARTESIAN_POINT('Ctrl Pts',(3.65765561320019,1.8201692464357,-30.1477175730606));
#28630=CARTESIAN_POINT('Ctrl Pts',(3.68617017732957,1.76170260746799,-30.1509008136042));
#28631=CARTESIAN_POINT('Ctrl Pts',(3.71325165581724,1.70264122485347,-30.1540840541477));
#28632=CARTESIAN_POINT('Ctrl Pts',(3.76281166486531,1.59455692443023,-30.1599094905326));
#28633=CARTESIAN_POINT('Ctrl Pts',(3.80772791300253,1.48413404864421,-30.1657349269176));
#28634=CARTESIAN_POINT('Ctrl Pts',(3.84777421648458,1.37180850666428,-30.1715603633025));
#28635=CARTESIAN_POINT('Ctrl Pts',(3.88777025349365,1.25962395669434,-30.1773784875483));
#28636=CARTESIAN_POINT('Ctrl Pts',(3.92290836847849,1.14554187177275,-30.1831966117942));
#28637=CARTESIAN_POINT('Ctrl Pts',(3.95300932257877,1.03002053164261,-30.1890147360401));
#28638=CARTESIAN_POINT('Ctrl Pts',(3.98308032398347,0.914614143866526,-30.1948270708181));
#28639=CARTESIAN_POINT('Ctrl Pts',(4.00812403386335,0.797771742659466,-30.2006394055962));
#28640=CARTESIAN_POINT('Ctrl Pts',(4.02801037385384,0.679968696430837,-30.2064517403742));
#28641=CARTESIAN_POINT('Ctrl Pts',(4.04856847625628,0.558186252358891,-30.2124604163609));
#28642=CARTESIAN_POINT('Ctrl Pts',(4.06361445849569,0.435377531316219,-30.2184690923477));
#28643=CARTESIAN_POINT('Ctrl Pts',(4.07306148925245,0.312081887921398,-30.2244777683344));
#28644=CARTESIAN_POINT('Ctrl Pts',(4.08218964709338,0.192947937478719,-30.2302836288459));
#28645=CARTESIAN_POINT('Ctrl Pts',(4.08609069153235,0.0733598444011744,
-30.2360894893574));
#28646=CARTESIAN_POINT('Ctrl Pts',(4.08473886019349,-0.0461892197937499,
-30.2418953498689));
#28647=CARTESIAN_POINT('Ctrl Pts',(4.08338722476066,-0.165720959060078,
-30.2477003690011));
#28648=CARTESIAN_POINT('Ctrl Pts',(4.07678423208726,-0.285213272806567,
-30.2535053881332));
#28649=CARTESIAN_POINT('Ctrl Pts',(4.06495624755798,-0.404172865788039,
-30.2593104072653));
#28650=CARTESIAN_POINT('Ctrl Pts',(4.05312719109958,-0.523143239664004,
-30.2651159524862));
#28651=CARTESIAN_POINT('Ctrl Pts',(4.0360722416797,-0.641580390751066,-30.270921497707));
#28652=CARTESIAN_POINT('Ctrl Pts',(4.01386958827962,-0.758996658941261,
-30.2767270429278));
#28653=CARTESIAN_POINT('Ctrl Pts',(3.99165969303522,-0.876451224821353,
-30.2825344817446));
#28654=CARTESIAN_POINT('Ctrl Pts',(3.96429883033393,-0.992883844869048,
-30.2883419205614));
#28655=CARTESIAN_POINT('Ctrl Pts',(3.93191605687673,-1.10781818078371,-30.2941493593782));
#28656=CARTESIAN_POINT('Ctrl Pts',(3.89949758990046,-1.22287920167539,-30.2999631993739));
#28657=CARTESIAN_POINT('Ctrl Pts',(3.8620462740892,-1.33643824908993,-30.3057770393697));
#28658=CARTESIAN_POINT('Ctrl Pts',(3.81974074103337,-1.44803510706399,-30.3115908793655));
#28659=CARTESIAN_POINT('Ctrl Pts',(3.77740737445923,-1.55970538647885,-30.3174085443839));
#28660=CARTESIAN_POINT('Ctrl Pts',(3.73021359112887,-1.66941053150841,-30.3232262094023));
#28661=CARTESIAN_POINT('Ctrl Pts',(3.67838508536788,-1.77671274091879,-30.3290438744207));
#28662=CARTESIAN_POINT('Ctrl Pts',(3.62648313820408,-1.88416699840903,-30.3348697831164));
#28663=CARTESIAN_POINT('Ctrl Pts',(3.5699335535695,-1.98921116644357,-30.3406956918122));
#28664=CARTESIAN_POINT('Ctrl Pts',(3.50900667166786,-2.09143423950896,-30.346521600508));
#28665=CARTESIAN_POINT('Ctrl Pts',(3.49458044792067,-2.11563854601767,-30.3479010550238));
#28666=CARTESIAN_POINT('Ctrl Pts',(3.4799089969373,-2.13968482824368,-30.3492805095397));
#28667=CARTESIAN_POINT('Ctrl Pts',(3.4649962422784,-2.16356789609122,-30.3506599640555));
#28668=CARTESIAN_POINT('Ctrl Pts',(3.40201945063289,-2.26442645791249,-30.356485421633));
#28669=CARTESIAN_POINT('Ctrl Pts',(3.33453460157875,-2.36269440139011,-30.3623108792105));
#28670=CARTESIAN_POINT('Ctrl Pts',(3.26278121164091,-2.45794299465286,-30.368136336788));
#28671=CARTESIAN_POINT('Ctrl Pts',(3.19111788326781,-2.55307203624906,-30.3739544825183));
#28672=CARTESIAN_POINT('Ctrl Pts',(3.11519691389463,-2.64518894245019,-30.3797726282486));
#28673=CARTESIAN_POINT('Ctrl Pts',(3.03530233160536,-2.73389186979864,-30.3855907739789));
#28674=CARTESIAN_POINT('Ctrl Pts',(2.95548724647239,-2.82250653546177,-30.3914031305051));
#28675=CARTESIAN_POINT('Ctrl Pts',(2.87170668579596,-2.9077136788627,-30.3972154870313));
#28676=CARTESIAN_POINT('Ctrl Pts',(2.7842859981162,-2.98914310140784,-30.4030278435576));
#28677=CARTESIAN_POINT('Ctrl Pts',(2.69391269076265,-3.07332278960993,-30.4090365114911));
#28678=CARTESIAN_POINT('Ctrl Pts',(2.59964928194172,-3.15346470158736,-30.4150451794247));
#28679=CARTESIAN_POINT('Ctrl Pts',(2.50189833929529,-3.22919954475276,-30.4210538473583));
#28680=CARTESIAN_POINT('Ctrl Pts',(2.40744637079887,-3.30237843006147,-30.4268597301355));
#28681=CARTESIAN_POINT('Ctrl Pts',(2.30973881837302,-3.37144264327577,-30.4326656129127));
#28682=CARTESIAN_POINT('Ctrl Pts',(2.20917329806707,-3.4360992912178,-30.4384714956899));
#28683=CARTESIAN_POINT('Ctrl Pts',(2.10862234890972,-3.50074657092286,-30.4442765372407));
#28684=CARTESIAN_POINT('Ctrl Pts',(2.00521459852327,-3.56098733482191,-30.4500815787914));
#28685=CARTESIAN_POINT('Ctrl Pts',(1.89937645088224,-3.61657214746699,-30.4558866203421));
#28686=CARTESIAN_POINT('Ctrl Pts',(1.79352870918881,-3.67216199878307,-30.4616921881102));
#28687=CARTESIAN_POINT('Ctrl Pts',(1.68525049345233,-3.72309486997931,-30.4674977558783));
#28688=CARTESIAN_POINT('Ctrl Pts',(1.5749920196836,-3.7691676983033,-30.4733033236464));
#28689=CARTESIAN_POINT('Ctrl Pts',(1.46469758103843,-3.81525555498312,-30.479110785115));
#28690=CARTESIAN_POINT('Ctrl Pts',(1.35242197599852,-3.85648005875395,-30.4849182465836));
#28691=CARTESIAN_POINT('Ctrl Pts',(1.2386339583867,-3.89268685063817,-30.4907257080522));
#28692=CARTESIAN_POINT('Ctrl Pts',(1.12472051898372,-3.92893355112424,-30.4965395707415));
#28693=CARTESIAN_POINT('Ctrl Pts',(1.00929172853534,-3.96015137635691,-30.5023534334309));
#28694=CARTESIAN_POINT('Ctrl Pts',(0.892830158941835,-3.9862362332511,-30.5081672961202));
#28695=CARTESIAN_POINT('Ctrl Pts',(0.776291966619323,-4.01233825196895,
-30.5139849838828));
#28696=CARTESIAN_POINT('Ctrl Pts',(0.658720042652412,-4.03330050522126,
-30.5198026716453));
#28697=CARTESIAN_POINT('Ctrl Pts',(0.540604140656138,-4.04907053076449,
-30.5256203594078));
#28698=CARTESIAN_POINT('Ctrl Pts',(0.422320870117633,-4.06486290220816,
-30.5314462907506));
#28699=CARTESIAN_POINT('Ctrl Pts',(0.3034924880319,-4.07544832564865,-30.5372722220934));
#28700=CARTESIAN_POINT('Ctrl Pts',(0.184610941756973,-4.08082636241529,
-30.5430981534362));
#28701=CARTESIAN_POINT('Ctrl Pts',(0.156466736972135,-4.08209956732256,
-30.5444773936119));
#28702=CARTESIAN_POINT('Ctrl Pts',(0.128319537569869,-4.08308114553061,
-30.5458566337877));
#28703=CARTESIAN_POINT('Ctrl Pts',(0.100175833174998,-4.08377151692497,
-30.5472358739634));
#28704=CARTESIAN_POINT('Ctrl Pts',(-0.0186938050359793,-4.08668741586732,
-30.553061325311));
#28705=CARTESIAN_POINT('Ctrl Pts',(-0.137881017317987,-4.08441362222163,
-30.5588867766586));
#28706=CARTESIAN_POINT('Ctrl Pts',(-0.256896020854348,-4.07691420494339,
-30.5647122280062));
#28707=CARTESIAN_POINT('Ctrl Pts',(-0.375761641061523,-4.06942420066256,
-30.5705303674579));
#28708=CARTESIAN_POINT('Ctrl Pts',(-0.494455078778615,-4.05672164417915,
-30.5763485069096));
#28709=CARTESIAN_POINT('Ctrl Pts',(-0.612484508638743,-4.03882256687237,
-30.5821666463614));
#28710=CARTESIAN_POINT('Ctrl Pts',(-0.73039649524063,-4.02094129975041,
-30.5879789965684));
#28711=CARTESIAN_POINT('Ctrl Pts',(-0.847645387292645,-3.99787385934325,
-30.5937913467753));
#28712=CARTESIAN_POINT('Ctrl Pts',(-0.96374304443309,-3.96968819232781,
-30.5996036969823));
#28713=CARTESIAN_POINT('Ctrl Pts',(-1.08376205877522,-3.94055051584846,
-30.6056123672694));
#28714=CARTESIAN_POINT('Ctrl Pts',(-1.20255024929556,-3.90594277036763,
-30.6116210375564));
#28715=CARTESIAN_POINT('Ctrl Pts',(-1.31957773775598,-3.8659978781705,-30.6176297078434));
#28716=CARTESIAN_POINT('Ctrl Pts',(-1.43265552380764,-3.82740113450671,
-30.6234355842415));
#28717=CARTESIAN_POINT('Ctrl Pts',(-1.54408912124532,-3.7838218328427,-30.6292414606395));
#28718=CARTESIAN_POINT('Ctrl Pts',(-1.65341517088357,-3.73543080148623,
-30.6350473370375));
#28719=CARTESIAN_POINT('Ctrl Pts',(-1.7627253798184,-3.6870467817064,-30.6408523721981));
#28720=CARTESIAN_POINT('Ctrl Pts',(-1.86992827526061,-3.63385258388174,
-30.6466574073587));
#28721=CARTESIAN_POINT('Ctrl Pts',(-1.97458094298633,-3.57606698757101,
-30.6524624425193));
#28722=CARTESIAN_POINT('Ctrl Pts',(-2.0792430972436,-3.51827615312451,-30.6582680038934));
#28723=CARTESIAN_POINT('Ctrl Pts',(-2.18135420695917,-3.455893289919,-30.6640735652675));
#28724=CARTESIAN_POINT('Ctrl Pts',(-2.28049697495161,-3.38918257803214,
-30.6698791266416));
#28725=CARTESIAN_POINT('Ctrl Pts',(-2.37967208211172,-3.32245010592069,
-30.6756865817194));
#28726=CARTESIAN_POINT('Ctrl Pts',(-2.47587658358236,-3.25138720521719,
-30.6814940367971));
#28727=CARTESIAN_POINT('Ctrl Pts',(-2.56872364793758,-3.17630033537861,
-30.6873014918749));
#28728=CARTESIAN_POINT('Ctrl Pts',(-2.66167305281528,-3.10113070116245,
-30.6931153482104));
#28729=CARTESIAN_POINT('Ctrl Pts',(-2.75125731632493,-3.0219285012329,-30.6989292045459));
#28730=CARTESIAN_POINT('Ctrl Pts',(-2.83712397431085,-2.93903939313352,
-30.7047430608813));
#28731=CARTESIAN_POINT('Ctrl Pts',(-2.92304712620692,-2.85609575013158,
-30.7105607423043));
#28732=CARTESIAN_POINT('Ctrl Pts',(-3.00524752123524,-2.76946066331204,
-30.7163784237272));
#28733=CARTESIAN_POINT('Ctrl Pts',(-3.0834118540804,-2.67951419815542,-30.7221961051502));
#28734=CARTESIAN_POINT('Ctrl Pts',(-3.16168694570897,-2.58944027894539,
-30.7280220302221));
#28735=CARTESIAN_POINT('Ctrl Pts',(-3.23591430765873,-2.49604593459566,
-30.7338479552939));
#28736=CARTESIAN_POINT('Ctrl Pts',(-3.30582286615256,-2.39974168977057,
-30.7396738803658));
#28737=CARTESIAN_POINT('Ctrl Pts',(-3.32237387826253,-2.376941438175,-30.7410531815342));
#28738=CARTESIAN_POINT('Ctrl Pts',(-3.33868301416142,-2.3539781956605,-30.7424324827027));
#28739=CARTESIAN_POINT('Ctrl Pts',(-3.35474705291792,-2.33085761275512,
-30.7438117838712));
#28740=CARTESIAN_POINT('Ctrl Pts',(-3.42331240557961,-2.23217315707866,
-30.7496989877354));
#28741=CARTESIAN_POINT('Ctrl Pts',(-3.48762617031097,-2.13030776213689,
-30.7555861915996));
#28742=CARTESIAN_POINT('Ctrl Pts',(-3.54738393391391,-2.02565846711864,
-30.7614733954638));
#28743=CARTESIAN_POINT('Ctrl Pts',(-3.60706316142376,-1.9211467064772,-30.7673528621243));
#28744=CARTESIAN_POINT('Ctrl Pts',(-3.66219810464387,-1.81385866534241,
-30.7732323287848));
#28745=CARTESIAN_POINT('Ctrl Pts',(-3.71252654954439,-1.70422170474619,
-30.7791117954454));
#28746=CARTESIAN_POINT('Ctrl Pts',(-3.76279980455952,-1.59470497141514,
-30.7849848147163));
#28747=CARTESIAN_POINT('Ctrl Pts',(-3.80827688453195,-1.48284480201287,
-30.7908578339872));
#28748=CARTESIAN_POINT('Ctrl Pts',(-3.84874084897415,-1.36909418136144,
-30.7967308532581));
#28749=CARTESIAN_POINT('Ctrl Pts',(-3.88916423668627,-1.25545762833275,
-30.8025979831428));
#28750=CARTESIAN_POINT('Ctrl Pts',(-3.92458438771809,-1.13993477134696,
-30.8084651130274));
#28751=CARTESIAN_POINT('Ctrl Pts',(-3.95483223170249,-1.02299903181141,
-30.814332242912));
#28752=CARTESIAN_POINT('Ctrl Pts',(-3.98506197191538,-0.906133280004967,
-30.8201958612347));
#28753=CARTESIAN_POINT('Ctrl Pts',(-4.01012546641762,-0.787856711325189,
-30.8260594795573));
#28754=CARTESIAN_POINT('Ctrl Pts',(-4.02990337715007,-0.668658186844704,
-30.83192309788));
#28755=CARTESIAN_POINT('Ctrl Pts',(-4.04967567644589,-0.54949348165766,
-30.8377850525627));
#28756=CARTESIAN_POINT('Ctrl Pts',(-4.06416530707864,-0.429407731267402,
-30.8436470072454));
#28757=CARTESIAN_POINT('Ctrl Pts',(-4.07330404263058,-0.308899945434376,
-30.8495089619281));
#28758=CARTESIAN_POINT('Ctrl Pts',(-4.08115411744783,-0.205385063153964,
-30.8545443174839));
#28759=CARTESIAN_POINT('Ctrl Pts',(-4.08505678108027,-0.101559090407424,
-30.8595796730397));
#28760=CARTESIAN_POINT('Ctrl Pts',(-4.08499937550953,0.00225877991778599,
-30.8646150285955));
#28761=CARTESIAN_POINT('Ctrl Pts',(-4.08499937550906,0.00225878076645493,
-30.8646150286367));
#28762=CARTESIAN_POINT('Ctrl Pts',(-4.08492561213899,0.135659651349435,
-30.8710852135166));
#28763=CARTESIAN_POINT('Ctrl Pts',(-4.07831318027114,0.268830275595934,
-30.8775553983965));
#28764=CARTESIAN_POINT('Ctrl Pts',(-4.06525415584447,0.401165362898193,
-30.8840255832764));
#28765=CARTESIAN_POINT('Ctrl Pts',(-4.05215046831583,0.533953048748885,
-30.8905178968022));
#28766=CARTESIAN_POINT('Ctrl Pts',(-4.03255612843008,0.66589925285231,-30.897010210328));
#28767=CARTESIAN_POINT('Ctrl Pts',(-4.00661426767472,0.796408883718279,
-30.9035025238538));
#28768=CARTESIAN_POINT('Ctrl Pts',(-3.98054550005077,0.927556964105285,
-30.9100265975987));
#28769=CARTESIAN_POINT('Ctrl Pts',(-3.94806706131849,1.05725416485448,-30.9165506713435));
#28770=CARTESIAN_POINT('Ctrl Pts',(-3.90937308787973,1.18491647796868,-30.9230747450883));
#28771=CARTESIAN_POINT('Ctrl Pts',(-3.87514566071344,1.29784239732178,-30.9288457279852));
#28772=CARTESIAN_POINT('Ctrl Pts',(-3.83605559115198,1.4091762978872,-30.9346167108821));
#28773=CARTESIAN_POINT('Ctrl Pts',(-3.79226783004088,1.51852879631472,-30.9403876937791));
#28774=CARTESIAN_POINT('Ctrl Pts',(-3.74806677993901,1.62891341382224,-30.9462131458618));
#28775=CARTESIAN_POINT('Ctrl Pts',(-3.69897144175243,1.73754311851044,-30.9520385979445));
#28776=CARTESIAN_POINT('Ctrl Pts',(-3.64514196067406,1.84395365628674,-30.9578640500273));
#28777=CARTESIAN_POINT('Ctrl Pts',(-3.5913800444854,1.95023063126244,-30.9636821902055));
#28778=CARTESIAN_POINT('Ctrl Pts',(-3.53289598698534,2.05429361865815,-30.9695003303837));
#28779=CARTESIAN_POINT('Ctrl Pts',(-3.46989848950998,2.15569698067617,-30.9753184705619));
#28780=CARTESIAN_POINT('Ctrl Pts',(-3.40696367676164,2.25699944278035,-30.9811308214858));
#28781=CARTESIAN_POINT('Ctrl Pts',(-3.33952457267184,2.35564719972549,-30.9869431724098));
#28782=CARTESIAN_POINT('Ctrl Pts',(-3.26783613254311,2.45121847472756,-30.9927555233338));
#28783=CARTESIAN_POINT('Ctrl Pts',(-3.19372632977344,2.55001778362771,-30.9987641933485));
#28784=CARTESIAN_POINT('Ctrl Pts',(-3.11507525756464,2.64552871191254,-31.0047728633632));
#28785=CARTESIAN_POINT('Ctrl Pts',(-3.03221404090021,2.73731675371477,-31.0107815333779));
#28786=CARTESIAN_POINT('Ctrl Pts',(-2.95214939464771,2.82600694428811,-31.0165874104642));
#28787=CARTESIAN_POINT('Ctrl Pts',(-2.8681544986675,2.91122116165802,-31.0223932875505));
#28788=CARTESIAN_POINT('Ctrl Pts',(-2.78056907741362,2.99260097669755,-31.0281991646368));
#28789=CARTESIAN_POINT('Ctrl Pts',(-2.69299634695159,3.0739690001138,-31.0340042004738));
#28790=CARTESIAN_POINT('Ctrl Pts',(-2.60183442470136,3.15150344847954,-31.0398092363108));
#28791=CARTESIAN_POINT('Ctrl Pts',(-2.50745903644586,3.22488359178219,-31.0456142721478));
#28792=CARTESIAN_POINT('Ctrl Pts',(-2.41307509347945,3.2982703866698,-31.0514198341855));
#28793=CARTESIAN_POINT('Ctrl Pts',(-2.31547742748063,3.36750187732411,-31.0572253962233));
#28794=CARTESIAN_POINT('Ctrl Pts',(-2.21507338178205,3.43229877972776,-31.063030958261));
#28795=CARTESIAN_POINT('Ctrl Pts',(-2.11463658573953,3.49711681794146,-31.068838413989));
#28796=CARTESIAN_POINT('Ctrl Pts',(-2.01139193209287,3.55749716998283,-31.0746458697169));
#28797=CARTESIAN_POINT('Ctrl Pts',(-1.90577360130433,3.61320522259275,-31.0804533254448));
#28798=CARTESIAN_POINT('Ctrl Pts',(-1.80003885332598,3.66897467907912,-31.086267182407));
#28799=CARTESIAN_POINT('Ctrl Pts',(-1.69192556689879,3.72006136601361,-31.0920810393691));
#28800=CARTESIAN_POINT('Ctrl Pts',(-1.58189038937199,3.76627771095183,-31.0978948963313));
#28801=CARTESIAN_POINT('Ctrl Pts',(-1.47178281709053,3.81252446272019,-31.1037125783679));
#28802=CARTESIAN_POINT('Ctrl Pts',(-1.35975121732951,3.85389434991448,-31.1095302604046));
#28803=CARTESIAN_POINT('Ctrl Pts',(-1.24626841271652,3.89024935492123,-31.1153479424412));
#28804=CARTESIAN_POINT('Ctrl Pts',(-1.13262480355803,3.9266558747815,-31.1211738681031));
#28805=CARTESIAN_POINT('Ctrl Pts',(-1.0175262775519,3.95803322277259,-31.126999793765));
#28806=CARTESIAN_POINT('Ctrl Pts',(-0.90145699208723,3.98429420241742,-31.1328257194269));
#28807=CARTESIAN_POINT('Ctrl Pts',(-0.87397745222479,3.9905115202383,-31.1342050141802));
#28808=CARTESIAN_POINT('Ctrl Pts',(-0.846443525971942,3.99644228842767,
-31.1355843089335));
#28809=CARTESIAN_POINT('Ctrl Pts',(-0.818861676052402,4.00208577562908,
-31.1369636036868));
#28810=CARTESIAN_POINT('Ctrl Pts',(-0.702359155593036,4.02592320803711,
-31.1427895840212));
#28811=CARTESIAN_POINT('Ctrl Pts',(-0.584628507797557,4.04470739476196,
-31.1486155643556));
#28812=CARTESIAN_POINT('Ctrl Pts',(-0.466145630715787,4.05831655381447,
-31.15444154469));
#28813=CARTESIAN_POINT('Ctrl Pts',(-0.34781401136114,4.07190833912897,-31.1602600874556));
#28814=CARTESIAN_POINT('Ctrl Pts',(-0.228732474960152,4.08033819224685,
-31.1660786302213));
#28815=CARTESIAN_POINT('Ctrl Pts',(-0.109388066938815,4.08353514137094,
-31.1718971729869));
#28816=CARTESIAN_POINT('Ctrl Pts',(0.00981731446799178,4.08672836630702,
-31.1777089376193));
#28817=CARTESIAN_POINT('Ctrl Pts',(0.129284552250609,4.08470081266939,-31.1835207022516));
#28818=CARTESIAN_POINT('Ctrl Pts',(0.248521322754568,4.07743327991229,-31.189332466884));
#28819=CARTESIAN_POINT('Ctrl Pts',(0.367680019558455,4.070170505781,-31.1951404260965));
#28820=CARTESIAN_POINT('Ctrl Pts',(0.486608143423988,4.05767460030551,-31.2009483853091));
#28821=CARTESIAN_POINT('Ctrl Pts',(0.604813442383292,4.0399784281494,-31.2067563445217));
#28822=CARTESIAN_POINT('Ctrl Pts',(0.722969186547713,4.02228967469777,-31.2125618688837));
#28823=CARTESIAN_POINT('Ctrl Pts',(0.840402305801329,3.99940505161285,-31.2183673932458));
#28824=CARTESIAN_POINT('Ctrl Pts',(0.95662637542646,3.97140919294882,-31.2241729176079));
#28825=CARTESIAN_POINT('Ctrl Pts',(1.07282909645558,3.94341847669875,-31.2299773755834));
#28826=CARTESIAN_POINT('Ctrl Pts',(1.18782281360997,3.91031848945809,-31.2357818335588));
#28827=CARTESIAN_POINT('Ctrl Pts',(1.30113261510672,3.87224468724609,-31.2415862915343));
#28828=CARTESIAN_POINT('Ctrl Pts',(1.41449321598884,3.83415381567445,-31.2473933517815));
#28829=CARTESIAN_POINT('Ctrl Pts',(1.52616800452399,3.79108480033464,-31.2532004120287));
#28830=CARTESIAN_POINT('Ctrl Pts',(1.6356985823936,3.7432225618517,-31.259007472276));
#28831=CARTESIAN_POINT('Ctrl Pts',(1.74525281094271,3.69534998858841,-31.264815786428));
#28832=CARTESIAN_POINT('Ctrl Pts',(1.85266153693647,3.64268230381903,-31.2706241005801));
#28833=CARTESIAN_POINT('Ctrl Pts',(1.95748887066811,3.58545148080552,-31.2764324147321));
#28834=CARTESIAN_POINT('Ctrl Pts',(2.06242494028727,3.52816129308138,-31.282246753765));
#28835=CARTESIAN_POINT('Ctrl Pts',(2.16477391544684,3.46629871683843,-31.2880610927979));
#28836=CARTESIAN_POINT('Ctrl Pts',(2.26412673941784,3.40014045413614,-31.2938754318308));
#28837=CARTESIAN_POINT('Ctrl Pts',(2.34025237969557,3.34944899005311,-31.2983304665644));
#28838=CARTESIAN_POINT('Ctrl Pts',(2.41461955876163,3.29623651745497,-31.302785501298));
#28839=CARTESIAN_POINT('Ctrl Pts',(2.4870572760686,3.24064362520075,-31.3072405360316));
#28840=CARTESIAN_POINT('',(-4.0849998777634,-0.000999336289953151,-30.7603849714308));
#28841=CARTESIAN_POINT('Ctrl Pts',(-4.0849998777634,-0.000999336289958593,
-30.7603849714308));
#28842=CARTESIAN_POINT('Ctrl Pts',(-4.08502878140532,0.117150454651573,
-30.7661717510729));
#28843=CARTESIAN_POINT('Ctrl Pts',(-4.07992758781669,0.235499771329081,
-30.771958530715));
#28844=CARTESIAN_POINT('Ctrl Pts',(-4.06967048002941,0.353563550125268,
-30.7777453103571));
#28845=CARTESIAN_POINT('Ctrl Pts',(-4.05942604544232,0.471481454866637,
-30.7835249401264));
#28846=CARTESIAN_POINT('Ctrl Pts',(-4.0440383996604,0.58911411442606,-30.7893045698956));
#28847=CARTESIAN_POINT('Ctrl Pts',(-4.02353372521156,0.70597546847266,-30.7950841996648));
#28848=CARTESIAN_POINT('Ctrl Pts',(-4.00304886281704,0.822723908583459,
-30.8008582450323));
#28849=CARTESIAN_POINT('Ctrl Pts',(-3.97745687652882,0.938702119897351,
-30.8066322903999));
#28850=CARTESIAN_POINT('Ctrl Pts',(-3.94683577764503,1.05342885108637,-30.8124063357674));
#28851=CARTESIAN_POINT('Ctrl Pts',(-3.91623499835199,1.16807945175393,-30.818176549586));
#28852=CARTESIAN_POINT('Ctrl Pts',(-3.88061185040692,1.28147982521651,-30.8239467634046));
#28853=CARTESIAN_POINT('Ctrl Pts',(-3.84009535765694,1.39315923142388,-30.8297169772232));
#28854=CARTESIAN_POINT('Ctrl Pts',(-3.79959285552512,1.50480007397923,-30.835485198548));
#28855=CARTESIAN_POINT('Ctrl Pts',(-3.75420050846812,1.61472074181599,-30.8412534198729));
#28856=CARTESIAN_POINT('Ctrl Pts',(-3.70409691358811,1.7224665612856,-30.8470216411977));
#28857=CARTESIAN_POINT('Ctrl Pts',(-3.65399840620415,1.83020144029411,-30.85278927682));
#28858=CARTESIAN_POINT('Ctrl Pts',(-3.59918977690339,1.93576153470512,-30.8585569124423));
#28859=CARTESIAN_POINT('Ctrl Pts',(-3.539897097881,2.03871369652868,-30.8643245480646));
#28860=CARTESIAN_POINT('Ctrl Pts',(-3.48059598553024,2.14168050146506,-30.8700930040304));
#28861=CARTESIAN_POINT('Ctrl Pts',(-3.41680976255271,2.24203827781851,-30.8758614599962));
#28862=CARTESIAN_POINT('Ctrl Pts',(-3.34880926292386,2.33938058480346,-30.8816299159621));
#28863=CARTESIAN_POINT('Ctrl Pts',(-3.28074086235099,2.43682009158211,-30.8874041319386));
#28864=CARTESIAN_POINT('Ctrl Pts',(-3.20845001801478,2.531237775147,-30.8931783479151));
#28865=CARTESIAN_POINT('Ctrl Pts',(-3.13224961987479,2.62225805724651,-30.8989525638916));
#28866=CARTESIAN_POINT('Ctrl Pts',(-3.05601051015036,2.71332457977812,-30.9047297133049));
#28867=CARTESIAN_POINT('Ctrl Pts',(-2.97585817003844,2.80098995764446,-30.9105068627182));
#28868=CARTESIAN_POINT('Ctrl Pts',(-2.89214309340475,2.88491478683014,-30.9162840121315));
#28869=CARTESIAN_POINT('Ctrl Pts',(-2.80829517133501,2.96897279430314,-30.9220703291638));
#28870=CARTESIAN_POINT('Ctrl Pts',(-2.72087352310968,3.04927811451934,-30.9278566461962));
#28871=CARTESIAN_POINT('Ctrl Pts',(-2.63026287228673,3.1255307105626,-30.9336429632285));
#28872=CARTESIAN_POINT('Ctrl Pts',(-2.55198804997586,3.19140219864728,-30.9386415250248));
#28873=CARTESIAN_POINT('Ctrl Pts',(-2.47133408077662,3.25424990784216,-30.9436400868211));
#28874=CARTESIAN_POINT('Ctrl Pts',(-2.38856553803204,3.31390700993943,-30.9486386486174));
#28875=CARTESIAN_POINT('Ctrl Pts',(-2.29210496822836,3.38343291761305,-30.9544640999675));
#28876=CARTESIAN_POINT('Ctrl Pts',(-2.1924519525515,3.44885491838803,-30.9602895513175));
#28877=CARTESIAN_POINT('Ctrl Pts',(-2.08999043653105,3.50986680305802,-30.9661150026675));
#28878=CARTESIAN_POINT('Ctrl Pts',(-1.98765752650204,3.57080210781565,-30.9719331421215));
#28879=CARTESIAN_POINT('Ctrl Pts',(-1.88252347519659,3.62733809957456,-30.9777512815756));
#28880=CARTESIAN_POINT('Ctrl Pts',(-1.77500325432677,3.67921030210688,-30.9835694210296));
#28881=CARTESIAN_POINT('Ctrl Pts',(-1.66759001969913,3.73103089005007,-30.9893817712389));
#28882=CARTESIAN_POINT('Ctrl Pts',(-1.55779570442558,3.77819674462592,-30.9951941214482));
#28883=CARTESIAN_POINT('Ctrl Pts',(-1.44606155265126,3.82048831773424,-31.0010064716574));
#28884=CARTESIAN_POINT('Ctrl Pts',(-1.33055342710085,3.86420834655934,-31.0070151419436));
#28885=CARTESIAN_POINT('Ctrl Pts',(-1.21297248583528,3.90271876722747,-31.0130238122297));
#28886=CARTESIAN_POINT('Ctrl Pts',(-1.09383110888818,3.93583009100094,-31.0190324825159));
#28887=CARTESIAN_POINT('Ctrl Pts',(-0.978710778472982,3.96782390063249,
-31.024838358916));
#28888=CARTESIAN_POINT('Ctrl Pts',(-0.862134067259083,3.99477705599787,
-31.0306442353162));
#28889=CARTESIAN_POINT('Ctrl Pts',(-0.744579858420503,4.01656891319376,
-31.0364501117163));
#28890=CARTESIAN_POINT('Ctrl Pts',(-0.62704268249851,4.03835761287713,-31.042255146879));
#28891=CARTESIAN_POINT('Ctrl Pts',(-0.508528691703095,4.05498642731745,
-31.0480601820417));
#28892=CARTESIAN_POINT('Ctrl Pts',(-0.389526970813251,4.06638583253103,
-31.0538652172043));
#28893=CARTESIAN_POINT('Ctrl Pts',(-0.270514462684037,4.07778627107515,
-31.0596707785804));
#28894=CARTESIAN_POINT('Ctrl Pts',(-0.151014542731728,4.08395631899025,
-31.0654763399565));
#28895=CARTESIAN_POINT('Ctrl Pts',(-0.0315207883900234,4.08487838740632,
-31.0712819013326));
#28896=CARTESIAN_POINT('Ctrl Pts',(0.0880119433641171,4.08580075658992,
-31.0770893564123));
#28897=CARTESIAN_POINT('Ctrl Pts',(0.207538097719214,4.08147173864878,-31.082896811492));
#28898=CARTESIAN_POINT('Ctrl Pts',(0.326565368729646,4.07192584165607,-31.0887042665718));
#28899=CARTESIAN_POINT('Ctrl Pts',(0.445723837348451,4.06236942271452,-31.0945181229091));
#28900=CARTESIAN_POINT('Ctrl Pts',(0.564381918077031,4.04758467950395,-31.1003319792464));
#28901=CARTESIAN_POINT('Ctrl Pts',(0.682053536347371,4.02765787692501,-31.1061458355837));
#28902=CARTESIAN_POINT('Ctrl Pts',(0.799802573837945,4.00771796398402,-31.1119635170084));
#28903=CARTESIAN_POINT('Ctrl Pts',(0.916563458334111,3.98262933956737,-31.1177811984331));
#28904=CARTESIAN_POINT('Ctrl Pts',(1.03186300602667,3.95252877747824,-31.1235988798578));
#28905=CARTESIAN_POINT('Ctrl Pts',(1.14732593306399,3.92238556292247,-31.1294248049313));
#28906=CARTESIAN_POINT('Ctrl Pts',(1.26132300197495,3.88721635606053,-31.1352507300048));
#28907=CARTESIAN_POINT('Ctrl Pts',(1.37339868535747,3.84720691555034,-31.1410766550783));
#28908=CARTESIAN_POINT('Ctrl Pts',(1.39993286094534,3.83773458856888,-31.1424559562273));
#28909=CARTESIAN_POINT('Ctrl Pts',(1.42635944038976,3.82799116528291,-31.1438352573762));
#28910=CARTESIAN_POINT('Ctrl Pts',(1.45267257479978,3.81797949057149,-31.1452145585252));
#28911=CARTESIAN_POINT('Ctrl Pts',(1.56379356903068,3.77569994946805,-31.1510393801763));
#28912=CARTESIAN_POINT('Ctrl Pts',(1.67324497728437,3.72849754926938,-31.1568642018273));
#28913=CARTESIAN_POINT('Ctrl Pts',(1.78055999398934,3.67652432438637,-31.1626890234784));
#28914=CARTESIAN_POINT('Ctrl Pts',(1.88775658178706,3.62460845524368,-31.1685074170704));
#28915=CARTESIAN_POINT('Ctrl Pts',(1.99282110020167,3.56793240220706,-31.1743258106624));
#28916=CARTESIAN_POINT('Ctrl Pts',(2.09530430566209,3.50669714498898,-31.1801442042544));
#28917=CARTESIAN_POINT('Ctrl Pts',(2.19767752415647,3.44552760663798,-31.1859563534334));
#28918=CARTESIAN_POINT('Ctrl Pts',(2.29747459476058,3.37980881012102,-31.1917685026124));
#28919=CARTESIAN_POINT('Ctrl Pts',(2.39426943353907,3.30978834362871,-31.1975806517915));
#28920=CARTESIAN_POINT('Ctrl Pts',(2.42551596135264,3.28718490235662,-31.199456882831));
#28921=CARTESIAN_POINT('Ctrl Pts',(2.45644982626913,3.2641335517492,-31.2013331138705));
#28922=CARTESIAN_POINT('Ctrl Pts',(2.48705727606859,3.24064362520075,-31.2032093449099));
#28923=CARTESIAN_POINT('Ctrl Pts',(2.4870572760686,3.24064362520074,-29.953048263356));
#28924=CARTESIAN_POINT('Ctrl Pts',(2.55581230516247,3.1878770407962,-29.9572852085968));
#28925=CARTESIAN_POINT('Ctrl Pts',(2.62281785134413,3.1329747184487,-29.9615221538375));
#28926=CARTESIAN_POINT('Ctrl Pts',(2.68793986680533,3.07606961436807,-29.9657590990783));
#28927=CARTESIAN_POINT('Ctrl Pts',(2.77747548878455,2.99783134346125,-29.9715844336405));
#28928=CARTESIAN_POINT('Ctrl Pts',(2.86373562734555,2.91555542942311,-29.9774097682026));
#28929=CARTESIAN_POINT('Ctrl Pts',(2.94633518555609,2.82954660225877,-29.9832351027648));
#28930=CARTESIAN_POINT('Ctrl Pts',(3.0288310416831,2.74364575744655,-29.9890531237366));
#28931=CARTESIAN_POINT('Ctrl Pts',(3.10767517837059,2.6540216129624,-29.9948711447084));
#28932=CARTESIAN_POINT('Ctrl Pts',(3.18251613281278,2.56101855994571,-30.0006891656802));
#28933=CARTESIAN_POINT('Ctrl Pts',(3.25728259667433,2.46810807458094,-30.0065013958686));
#28934=CARTESIAN_POINT('Ctrl Pts',(3.32805355063709,2.37182568735685,-30.0123136260569));
#28935=CARTESIAN_POINT('Ctrl Pts',(3.39451535374224,2.27255154247559,-30.0181258562453));
#28936=CARTESIAN_POINT('Ctrl Pts',(3.46322392174458,2.1699213998107,-30.0241345709428));
#28937=CARTESIAN_POINT('Ctrl Pts',(3.52732652509763,2.06409396154969,-30.0301432856404));
#28938=CARTESIAN_POINT('Ctrl Pts',(3.58652269135608,1.95552550082783,-30.0361520003379));
#28939=CARTESIAN_POINT('Ctrl Pts',(3.64371933917572,1.85062424784606,-30.0419577536514));
#28940=CARTESIAN_POINT('Ctrl Pts',(3.6963354435903,1.74316454032156,-30.047763506965));
#28941=CARTESIAN_POINT('Ctrl Pts',(3.74414519394622,1.63358555535039,-30.0535692602785));
#28942=CARTESIAN_POINT('Ctrl Pts',(3.79194800921432,1.52402246546081,-30.0593741714331));
#28943=CARTESIAN_POINT('Ctrl Pts',(3.83494569383507,1.41234108338631,-30.0651790825877));
#28944=CARTESIAN_POINT('Ctrl Pts',(3.87295992550226,1.29900208446851,-30.0709839937423));
#28945=CARTESIAN_POINT('Ctrl Pts',(3.91097759798832,1.18565282678842,-30.0767894303224));
#28946=CARTESIAN_POINT('Ctrl Pts',(3.94401079092465,1.07064604082764,-30.0825948669025));
#28947=CARTESIAN_POINT('Ctrl Pts',(3.97193075561521,0.954458523246536,-30.0884003034826));
#28948=CARTESIAN_POINT('Ctrl Pts',(3.99985982450558,0.838233118999529,-30.0942076331115));
#28949=CARTESIAN_POINT('Ctrl Pts',(4.02267225388032,0.72082661394739,-30.1000149627404));
#28950=CARTESIAN_POINT('Ctrl Pts',(4.04029032990276,0.602726347602504,-30.1058222923693));
#28951=CARTESIAN_POINT('Ctrl Pts',(4.05792782479383,0.48449590963416,-30.1116360229111));
#28952=CARTESIAN_POINT('Ctrl Pts',(4.07035947817291,0.365570587843263,-30.1174497534529));
#28953=CARTESIAN_POINT('Ctrl Pts',(4.07755940143801,0.246443356056747,-30.1232634839948));
#28954=CARTESIAN_POINT('Ctrl Pts',(4.08476406139379,0.127237752761492,-30.1290810392778));
#28955=CARTESIAN_POINT('Ctrl Pts',(4.08673012989666,0.00783038195283492,
-30.1348985945609));
#28956=CARTESIAN_POINT('Ctrl Pts',(4.08348383393083,-0.111286917584897,
-30.140716149844));
#28957=CARTESIAN_POINT('Ctrl Pts',(4.08023293762059,-0.23057301892339,-30.1465419492176));
#28958=CARTESIAN_POINT('Ctrl Pts',(4.07175496331674,-0.349567823055712,
-30.1523677485913));
#28959=CARTESIAN_POINT('Ctrl Pts',(4.05812784669207,-0.467785613184488,
-30.1581935479649));
#28960=CARTESIAN_POINT('Ctrl Pts',(4.05489875206701,-0.495798614115334,
-30.159574034972));
#28961=CARTESIAN_POINT('Ctrl Pts',(4.05138075511121,-0.523768036727955,
-30.160954521979));
#28962=CARTESIAN_POINT('Ctrl Pts',(4.0475753082676,-0.551687523787168,-30.1623350089861));
#28963=CARTESIAN_POINT('Ctrl Pts',(4.03151677086633,-0.669504470282694,
-30.1681605015356));
#28964=CARTESIAN_POINT('Ctrl Pts',(4.01028415179671,-0.786808135138811,
-30.1739859940851));
#28965=CARTESIAN_POINT('Ctrl Pts',(3.98392001214754,-0.903109260726691,
-30.1798114866346));
#28966=CARTESIAN_POINT('Ctrl Pts',(3.95758896192584,-1.01926441767273,-30.1856296676535));
#28967=CARTESIAN_POINT('Ctrl Pts',(3.92613929087898,-1.1344191436337,-30.1914478486725));
#28968=CARTESIAN_POINT('Ctrl Pts',(3.88966518421875,-1.2480904433079,-30.1972660296914));
#28969=CARTESIAN_POINT('Ctrl Pts',(3.85322736831024,-1.36164864310685,-30.2030784217772));
#28970=CARTESIAN_POINT('Ctrl Pts',(3.81177518619867,-1.47372596663755,-30.2088908138631));
#28971=CARTESIAN_POINT('Ctrl Pts',(3.76545348818231,-1.58385132772482,-30.2147032059489));
#28972=CARTESIAN_POINT('Ctrl Pts',(3.7175676806409,-1.697695208072,-30.220711860655));
#28973=CARTESIAN_POINT('Ctrl Pts',(3.66447778562353,-1.80945253930661,-30.226720515361));
#28974=CARTESIAN_POINT('Ctrl Pts',(3.60639944226682,-1.91862139642442,-30.2327291700671));
#28975=CARTESIAN_POINT('Ctrl Pts',(3.55028070006073,-2.02410682516504,-30.2385350888479));
#28976=CARTESIAN_POINT('Ctrl Pts',(3.48950491311273,-2.12717524673955,-30.2443410076287));
#28977=CARTESIAN_POINT('Ctrl Pts',(3.42431455073011,-2.22739643028762,-30.2501469264095));
#28978=CARTESIAN_POINT('Ctrl Pts',(3.35913363272308,-2.32760309441189,-30.2559520040648));
#28979=CARTESIAN_POINT('Ctrl Pts',(3.28953963361879,-2.42496299892272,-30.2617570817201));
#28980=CARTESIAN_POINT('Ctrl Pts',(3.21581910435427,-2.51907373613201,-30.2675621593754));
#28981=CARTESIAN_POINT('Ctrl Pts',(3.14209189171015,-2.61319300526298,-30.2733677633094));
#28982=CARTESIAN_POINT('Ctrl Pts',(3.06423765671202,-2.70406220021829,-30.2791733672433));
#28983=CARTESIAN_POINT('Ctrl Pts',(2.98258368984066,-2.79131143606307,-30.2849789711772));
#28984=CARTESIAN_POINT('Ctrl Pts',(2.90090308837341,-2.87858913161689,-30.2907864688331));
#28985=CARTESIAN_POINT('Ctrl Pts',(2.81542056870581,-2.96224422196422,-30.296593966489));
#28986=CARTESIAN_POINT('Ctrl Pts',(2.72650030718747,-3.04194363440656,-30.302401464145));
#28987=CARTESIAN_POINT('Ctrl Pts',(2.63748203703935,-3.12173089218444,-30.3082153628717));
#28988=CARTESIAN_POINT('Ctrl Pts',(2.54501876580553,-3.19755349686545,-30.3140292615984));
#28989=CARTESIAN_POINT('Ctrl Pts',(2.44950789225112,-3.26911854875278,-30.3198431603251));
#28990=CARTESIAN_POINT('Ctrl Pts',(2.35393418106028,-3.34073068406155,-30.3256608840786));
#28991=CARTESIAN_POINT('Ctrl Pts',(2.25530921053142,-3.40807945849512,-30.3314786078321));
#28992=CARTESIAN_POINT('Ctrl Pts',(2.15405810963678,-3.47091611254262,-30.3372963315857));
#28993=CARTESIAN_POINT('Ctrl Pts',(2.05266354416293,-3.53384180102089,-30.3431222985809));
#28994=CARTESIAN_POINT('Ctrl Pts',(1.94863577614577,-3.5922424099139,-30.348948265576));
#28995=CARTESIAN_POINT('Ctrl Pts',(1.84242327695448,-3.64591572427783,-30.3547742325712));
#28996=CARTESIAN_POINT('Ctrl Pts',(1.8172848010542,-3.65861917565972,-30.3561531280121));
#28997=CARTESIAN_POINT('Ctrl Pts',(1.79202402162829,-3.67105802936119,-30.3575320234531));
#28998=CARTESIAN_POINT('Ctrl Pts',(1.76664702472144,-3.68323000775717,-30.358910918894));
#28999=CARTESIAN_POINT('Ctrl Pts',(1.65943611569282,-3.73465330552956,-30.3647363770528));
#29000=CARTESIAN_POINT('Ctrl Pts',(1.54980661304529,-3.78147396035117,-30.3705618352116));
#29001=CARTESIAN_POINT('Ctrl Pts',(1.43819045162136,-3.82345828078,-30.3763872933704));
#29002=CARTESIAN_POINT('Ctrl Pts',(1.32671438278899,-3.86538990550438,-30.3822054398324));
#29003=CARTESIAN_POINT('Ctrl Pts',(1.2132569933931,-3.90249712720995,-30.3880235862944));
#29004=CARTESIAN_POINT('Ctrl Pts',(1.09827339743581,-3.93459280542279,-30.3938417327564));
#29005=CARTESIAN_POINT('Ctrl Pts',(0.983404210146548,-3.96665654843859,
-30.3996540901631));
#29006=CARTESIAN_POINT('Ctrl Pts',(0.8670122281456,-3.99371855908819,-30.4054664475699));
#29007=CARTESIAN_POINT('Ctrl Pts',(0.749570501840176,-4.01564055447833,
-30.4112788049767));
#29008=CARTESIAN_POINT('Ctrl Pts',(0.628162224040345,-4.03830295727145,
-30.417287472636));
#29009=CARTESIAN_POINT('Ctrl Pts',(0.505632453066731,-4.05547183861424,
-30.4232961402954));
#29010=CARTESIAN_POINT('Ctrl Pts',(0.382518955690571,-4.06705105064313,
-30.4293048079548));
#29011=CARTESIAN_POINT('Ctrl Pts',(0.263560356499327,-4.07823948141679,
-30.4351106919805));
#29012=CARTESIAN_POINT('Ctrl Pts',(0.144057233575435,-4.08420940007617,
-30.4409165760062));
#29013=CARTESIAN_POINT('Ctrl Pts',(0.024502242208067,-4.08492651587844,
-30.4467224600319));
#29014=CARTESIAN_POINT('Ctrl Pts',(-0.0950354293644703,-4.08564352779297,
-30.4525275029658));
#29015=CARTESIAN_POINT('Ctrl Pts',(-0.214624546535855,-4.08110924778427,
-30.4583325458998));
#29016=CARTESIAN_POINT('Ctrl Pts',(-0.333771428519917,-4.07134150293288,
-30.4641375888337));
#29017=CARTESIAN_POINT('Ctrl Pts',(-0.452929113715939,-4.06157287242661,
-30.4699431581189));
#29018=CARTESIAN_POINT('Ctrl Pts',(-0.571644077331451,-4.04656986694565,
-30.4757487274041));
#29019=CARTESIAN_POINT('Ctrl Pts',(-0.689427376299411,-4.02640222690293,
-30.4815542966892));
#29020=CARTESIAN_POINT('Ctrl Pts',(-0.807249097334082,-4.00622800797834,
-30.487361759808));
#29021=CARTESIAN_POINT('Ctrl Pts',(-0.924138147339345,-3.98088587267945,
-30.4931692229268));
#29022=CARTESIAN_POINT('Ctrl Pts',(-1.03961602327505,-3.95049661740771,
-30.4989766860456));
#29023=CARTESIAN_POINT('Ctrl Pts',(-1.15522118737406,-3.92007386487552,
-30.5047905505751));
#29024=CARTESIAN_POINT('Ctrl Pts',(-1.26941167775888,-3.88459299165533,
-30.5106044151046));
#29025=CARTESIAN_POINT('Ctrl Pts',(-1.38172425354188,-3.84422464057112,
-30.5164182796341));
#29026=CARTESIAN_POINT('Ctrl Pts',(-1.49411072450046,-3.80382972944793,
-30.52223596935));
#29027=CARTESIAN_POINT('Ctrl Pts',(-1.60461644351643,-3.75854109062448,
-30.528053659066));
#29028=CARTESIAN_POINT('Ctrl Pts',(-1.71279976673854,-3.70857681045713,
-30.5338713487819));
#29029=CARTESIAN_POINT('Ctrl Pts',(-1.82113638694164,-3.65854173034503,
-30.5396972822294));
#29030=CARTESIAN_POINT('Ctrl Pts',(-1.92714368200098,-3.60381797186832,
-30.5455232156768));
#29031=CARTESIAN_POINT('Ctrl Pts',(-2.03040602722965,-3.54466872423778,
-30.5513491491242));
#29032=CARTESIAN_POINT('Ctrl Pts',(-2.05485226754216,-3.53066578135789,
-30.5527283756834));
#29033=CARTESIAN_POINT('Ctrl Pts',(-2.07914480153312,-3.51641499580859,
-30.5541076022426));
#29034=CARTESIAN_POINT('Ctrl Pts',(-2.10327837461796,-3.50192019881442,
-30.5554868288017));
#29035=CARTESIAN_POINT('Ctrl Pts',(-2.20521129883434,-3.44069855383277,
-30.5613122652524));
#29036=CARTESIAN_POINT('Ctrl Pts',(-2.30463204263936,-3.374924722447,-30.567137701703));
#29037=CARTESIAN_POINT('Ctrl Pts',(-2.40110779457756,-3.30483076099502,
-30.5729631381536));
#29038=CARTESIAN_POINT('Ctrl Pts',(-2.49746244931989,-3.23482478208795,
-30.5787812624662));
#29039=CARTESIAN_POINT('Ctrl Pts',(-2.59087913752951,-3.16050969663225,
-30.5845993867787));
#29040=CARTESIAN_POINT('Ctrl Pts',(-2.6809511614434,-3.08216253139825,-30.5904175110913));
#29041=CARTESIAN_POINT('Ctrl Pts',(-2.77093355698706,-3.00389332742711,
-30.596229845937));
#29042=CARTESIAN_POINT('Ctrl Pts',(-2.85757760328303,-2.92160029192114,
-30.6020421807826));
#29043=CARTESIAN_POINT('Ctrl Pts',(-2.9405075272883,-2.83560231378817,-30.6078545156283));
#29044=CARTESIAN_POINT('Ctrl Pts',(-3.0262388304751,-2.74669931737037,-30.61386319159));
#29045=CARTESIAN_POINT('Ctrl Pts',(-3.10800028326864,-2.65383690175527,
-30.6198718675517));
#29046=CARTESIAN_POINT('Ctrl Pts',(-3.18541567626639,-2.5574111850456,-30.6258805435135));
#29047=CARTESIAN_POINT('Ctrl Pts',(-3.26021800899849,-2.46424019842466,
-30.6316864040945));
#29048=CARTESIAN_POINT('Ctrl Pts',(-3.33096266304827,-2.36774292183173,
-30.6374922646755));
#29049=CARTESIAN_POINT('Ctrl Pts',(-3.39734990832777,-2.26831183931691,
-30.6432981252565));
#29050=CARTESIAN_POINT('Ctrl Pts',(-3.46372753284194,-2.16889516624336,
-30.6491031444586));
#29051=CARTESIAN_POINT('Ctrl Pts',(-3.52574877792394,-2.06654587204177,
-30.6549081636608));
#29052=CARTESIAN_POINT('Ctrl Pts',(-3.583156866379,-1.96168597663362,-30.660713182863));
#29053=CARTESIAN_POINT('Ctrl Pts',(-3.64057015753436,-1.85681657812889,
-30.6665187281543));
#29054=CARTESIAN_POINT('Ctrl Pts',(-3.69336926488391,-1.74943648394792,
-30.6723242734457));
#29055=CARTESIAN_POINT('Ctrl Pts',(-3.74134336481207,-1.63999232515787,
-30.6781298187371));
#29056=CARTESIAN_POINT('Ctrl Pts',(-3.78933311246614,-1.53051246893521,
-30.6839372576248));
#29057=CARTESIAN_POINT('Ctrl Pts',(-3.83249455906068,-1.41896758266827,
-30.6897446965126));
#29058=CARTESIAN_POINT('Ctrl Pts',(-3.87066525660072,-1.30582367544171,
-30.6955521354003));
#29059=CARTESIAN_POINT('Ctrl Pts',(-3.90887802733028,-1.19255505671236,
-30.7013659754673));
#29060=CARTESIAN_POINT('Ctrl Pts',(-3.94208893827324,-1.07768428581265,
-30.7071798155343));
#29061=CARTESIAN_POINT('Ctrl Pts',(-3.97018556064206,-0.961692057817527,
-30.7129936556013));
#29062=CARTESIAN_POINT('Ctrl Pts',(-3.99830066824993,-0.845623516590301,
-30.7188113206911));
#29063=CARTESIAN_POINT('Ctrl Pts',(-4.02129470776966,-0.728432448295096,
-30.724628985781));
#29064=CARTESIAN_POINT('Ctrl Pts',(-4.03910674923444,-0.610607622200049,
-30.7304466508709));
#29065=CARTESIAN_POINT('Ctrl Pts',(-4.05694403050203,-0.492615837399969,
-30.7362725596379));
#29066=CARTESIAN_POINT('Ctrl Pts',(-4.06958461511904,-0.373988906664999,
-30.742098468405));
#29067=CARTESIAN_POINT('Ctrl Pts',(-4.07701955093888,-0.255218693010852,
-30.747924377172));
#29068=CARTESIAN_POINT('Ctrl Pts',(-4.07877998887574,-0.227096380330193,
-30.7493038310179));
#29069=CARTESIAN_POINT('Ctrl Pts',(-4.08024880514175,-0.198966023605966,
-30.7506832848637));
#29070=CARTESIAN_POINT('Ctrl Pts',(-4.08142630741086,-0.170834121809958,
-30.7520627387096));
#29071=CARTESIAN_POINT('Ctrl Pts',(-4.08379426095805,-0.114260951299124,
-30.7548368162745));
#29072=CARTESIAN_POINT('Ctrl Pts',(-4.08498602187232,-0.0576382110579216,
-30.7576108938395));
#29073=CARTESIAN_POINT('Ctrl Pts',(-4.08499987776327,-0.000999336826385626,
-30.7603849714045));
#29074=CARTESIAN_POINT('Origin',(0.,0.,-25.2396150285955));
#29075=CARTESIAN_POINT('',(2.4870572760686,3.24064362520074,-28.7030585997167));
#29076=CARTESIAN_POINT('',(2.48705727606859,3.24064362520075,-28.807442179994));
#29077=CARTESIAN_POINT('',(2.4870572760686,3.24064362520075,-25.2396150285955));
#29078=CARTESIAN_POINT('',(-4.08246318168416,-0.00445590608020525,-28.2603840116597));
#29079=CARTESIAN_POINT('Ctrl Pts',(-4.08499758825475,-0.00443891347911176,
-28.2603849714045));
#29080=CARTESIAN_POINT('Ctrl Pts',(-4.08512632133835,0.114030243104064,
-28.2661368812369));
#29081=CARTESIAN_POINT('Ctrl Pts',(-4.08009719924304,0.232579851337021,
-28.2718887910694));
#29082=CARTESIAN_POINT('Ctrl Pts',(-4.06991623004305,0.350723367388326,
-28.2776407009018));
#29083=CARTESIAN_POINT('Ctrl Pts',(-4.05973778505935,0.468837591553652,
-28.2833911846358));
#29084=CARTESIAN_POINT('Ctrl Pts',(-4.04441006739671,0.586545509497618,
-28.2891416683697));
#29085=CARTESIAN_POINT('Ctrl Pts',(-4.02399111300928,0.703363719865031,
-28.2948921521037));
#29086=CARTESIAN_POINT('Ctrl Pts',(-4.00357219517005,0.820181721137633,
-28.3006426255448));
#29087=CARTESIAN_POINT('Ctrl Pts',(-3.97806213047916,0.936109608232255,
-28.3063930989858));
#29088=CARTESIAN_POINT('Ctrl Pts',(-3.94757030760067,1.05067295889327,-28.3121435724269));
#29089=CARTESIAN_POINT('Ctrl Pts',(-3.91707103353571,1.16526430502351,-28.3178954510923));
#29090=CARTESIAN_POINT('Ctrl Pts',(-3.8815876883295,1.27849004999528,-28.3236473297576));
#29091=CARTESIAN_POINT('Ctrl Pts',(-3.84127966719592,1.38989046992459,-28.329399208423));
#29092=CARTESIAN_POINT('Ctrl Pts',(-3.80092654050279,1.50141554936666,-28.3351575235667));
#29093=CARTESIAN_POINT('Ctrl Pts',(-3.75573810001732,1.61111083384206,-28.3409158387104));
#29094=CARTESIAN_POINT('Ctrl Pts',(-3.70592215450002,1.7185360004335,-28.3466741538541));
#29095=CARTESIAN_POINT('Ctrl Pts',(-3.65607626045009,1.82602574928012,-28.3524359308029));
#29096=CARTESIAN_POINT('Ctrl Pts',(-3.60159751384272,1.93124229436399,-28.3581977077516));
#29097=CARTESIAN_POINT('Ctrl Pts',(-3.54273911394695,2.03377102214343,-28.3639594847003));
#29098=CARTESIAN_POINT('Ctrl Pts',(-3.48378491100313,2.13646663459273,-28.369730640018));
#29099=CARTESIAN_POINT('Ctrl Pts',(-3.42043704149256,2.23646534248467,-28.3755017953357));
#29100=CARTESIAN_POINT('Ctrl Pts',(-3.35299154004781,2.33338225166127,-28.3812729506534));
#29101=CARTESIAN_POINT('Ctrl Pts',(-3.30671679128229,2.39987750378645,-28.3852325737075));
#29102=CARTESIAN_POINT('Ctrl Pts',(-3.25851398781532,2.4649226912196,-28.3891921967616));
#29103=CARTESIAN_POINT('Ctrl Pts',(-3.20848902628625,2.52840328432802,-28.3931518198157));
#29104=CARTESIAN_POINT('Ctrl Pts',(-3.13480852911598,2.62190224000785,-28.3989838481934));
#29105=CARTESIAN_POINT('Ctrl Pts',(-3.0569211542648,2.71232566598092,-28.4048158765711));
#29106=CARTESIAN_POINT('Ctrl Pts',(-2.97511270936837,2.79927300679208,-28.4106479049488));
#29107=CARTESIAN_POINT('Ctrl Pts',(-2.89340694843843,2.88611121341983,-28.4164726131066));
#29108=CARTESIAN_POINT('Ctrl Pts',(-2.80779018365383,2.96948171979137,-28.4222973212644));
#29109=CARTESIAN_POINT('Ctrl Pts',(-2.71858950157756,3.04901559883059,-28.4281220294222));
#29110=CARTESIAN_POINT('Ctrl Pts',(-2.62947773498685,3.12847019828015,-28.4339409314949));
#29111=CARTESIAN_POINT('Ctrl Pts',(-2.53678946060952,3.20409550973873,-28.4397598335676));
#29112=CARTESIAN_POINT('Ctrl Pts',(-2.44088935787284,3.27555860008993,-28.4455787356402));
#29113=CARTESIAN_POINT('Ctrl Pts',(-2.34190230406297,3.3493220327469,-28.451584943727));
#29114=CARTESIAN_POINT('Ctrl Pts',(-2.23949345769402,3.41865043738168,-28.4575911518138));
#29115=CARTESIAN_POINT('Ctrl Pts',(-2.1341021784629,3.4832216254324,-28.4635973599006));
#29116=CARTESIAN_POINT('Ctrl Pts',(-2.03211269591741,3.54570859878243,-28.469409700915));
#29117=CARTESIAN_POINT('Ctrl Pts',(-1.9273307206189,3.60374050069382,-28.4752220419294));
#29118=CARTESIAN_POINT('Ctrl Pts',(-1.82018425426441,3.65706908336825,-28.4810343829438));
#29119=CARTESIAN_POINT('Ctrl Pts',(-1.71305411494676,3.71038953980424,-28.4868458382705));
#29120=CARTESIAN_POINT('Ctrl Pts',(-1.60356056538362,3.75900792119536,-28.4926572935972));
#29121=CARTESIAN_POINT('Ctrl Pts',(-1.49215549176468,3.80272231281703,-28.4984687489239));
#29122=CARTESIAN_POINT('Ctrl Pts',(-1.38074132962146,3.84644027069737,-28.5042806783542));
#29123=CARTESIAN_POINT('Ctrl Pts',(-1.26741571220278,3.88525329475721,-28.5100926077846));
#29124=CARTESIAN_POINT('Ctrl Pts',(-1.15264916036561,3.91900815425389,-28.515904537215));
#29125=CARTESIAN_POINT('Ctrl Pts',(-1.03784639515901,3.95277366473883,-28.5217183005381));
#29126=CARTESIAN_POINT('Ctrl Pts',(-0.92160218145053,3.98147772156695,-28.5275320638612));
#29127=CARTESIAN_POINT('Ctrl Pts',(-0.804400192932084,4.00501751926391,
-28.5333458271843));
#29128=CARTESIAN_POINT('Ctrl Pts',(-0.687071603170412,4.0285827445811,-28.5391658705174));
#29129=CARTESIAN_POINT('Ctrl Pts',(-0.568783572669926,4.04697249560267,
-28.5449859138506));
#29130=CARTESIAN_POINT('Ctrl Pts',(-0.450028068493812,4.06013543340216,
-28.5508059571837));
#29131=CARTESIAN_POINT('Ctrl Pts',(-0.331195822144487,4.07330687735435,
-28.5566297615448));
#29132=CARTESIAN_POINT('Ctrl Pts',(-0.211895905580145,4.08124475368808,
-28.562453565906));
#29133=CARTESIAN_POINT('Ctrl Pts',(-0.0926218644566019,4.08394982709442,
-28.5682773702671));
#29134=CARTESIAN_POINT('Ctrl Pts',(0.0268181448968271,4.08665866457417,
-28.5741092783739));
#29135=CARTESIAN_POINT('Ctrl Pts',(0.146231801521961,4.08412017465436,-28.5799411864808));
#29136=CARTESIAN_POINT('Ctrl Pts',(0.265128984138461,4.07638707948224,-28.5857730945876));
#29137=CARTESIAN_POINT('Ctrl Pts',(0.292003834662801,4.07463913413763,-28.5870913062996));
#29138=CARTESIAN_POINT('Ctrl Pts',(0.318852333909899,4.07262599601133,-28.5884095180115));
#29139=CARTESIAN_POINT('Ctrl Pts',(0.345668893292544,4.07034863570799,-28.5897277297235));
#29140=CARTESIAN_POINT('Ctrl Pts',(0.464353441204676,4.06026950981499,-28.5955618622404));
#29141=CARTESIAN_POINT('Ctrl Pts',(0.582779642271394,4.04497959911709,-28.6013959947573));
#29142=CARTESIAN_POINT('Ctrl Pts',(0.700455418714115,4.02449837947464,-28.6072301272742));
#29143=CARTESIAN_POINT('Ctrl Pts',(0.817994270885021,4.00404099121169,-28.6130574713562));
#29144=CARTESIAN_POINT('Ctrl Pts',(0.934784037864472,3.97840437561073,-28.6188848154382));
#29145=CARTESIAN_POINT('Ctrl Pts',(1.05033640115567,3.94765986939191,-28.6247121595202));
#29146=CARTESIAN_POINT('Ctrl Pts',(1.16578128015835,3.91694396104234,-28.6305340831338));
#29147=CARTESIAN_POINT('Ctrl Pts',(1.27999065436538,3.88112971718499,-28.6363560067474));
#29148=CARTESIAN_POINT('Ctrl Pts',(1.39248566642517,3.84033965539514,-28.642177930361));
#29149=CARTESIAN_POINT('Ctrl Pts',(1.50489892442149,3.79957923717116,-28.647995622979));
#29150=CARTESIAN_POINT('Ctrl Pts',(1.61559991907097,3.75385033633467,-28.6538133155969));
#29151=CARTESIAN_POINT('Ctrl Pts',(1.72412488494293,3.70332531397399,-28.6596310082148));
#29152=CARTESIAN_POINT('Ctrl Pts',(1.83260372794383,3.65282176463633,-28.6654462283262));
#29153=CARTESIAN_POINT('Ctrl Pts',(1.93890801482212,3.59752632167616,-28.6712614484376));
#29154=CARTESIAN_POINT('Ctrl Pts',(2.04259438139677,3.53765928165593,-28.6770766685489));
#29155=CARTESIAN_POINT('Ctrl Pts',(2.14627427464938,3.4777959792402,-28.6828915256059));
#29156=CARTESIAN_POINT('Ctrl Pts',(2.24733621845074,3.41336184642097,-28.6887063826629));
#29157=CARTESIAN_POINT('Ctrl Pts',(2.34536224459767,3.34462269047135,-28.6945212397199));
#29158=CARTESIAN_POINT('Ctrl Pts',(2.393336107989,3.31098179930414,-28.6973670263855));
#29159=CARTESIAN_POINT('Ctrl Pts',(2.44058325170965,3.27631047839352,-28.7002128130511));
#29160=CARTESIAN_POINT('Ctrl Pts',(2.48705727606861,3.24064362520074,-28.7030585997167));
#29161=CARTESIAN_POINT('',(-1.05790442297295,-3.94563850749841,-28.));
#29162=CARTESIAN_POINT('Ctrl Pts',(-1.05790442297292,-3.94563850749842,
-28.));
#29163=CARTESIAN_POINT('Ctrl Pts',(-2.35746398375646,-3.59720065525805,
-28.0655253033026));
#29164=CARTESIAN_POINT('Ctrl Pts',(-3.81889380336946,-2.22310313068615,
-28.1523197509));
#29165=CARTESIAN_POINT('Ctrl Pts',(-4.08374969685893,-0.442080030969895,
-28.2391141984974));
#29166=CARTESIAN_POINT('Ctrl Pts',(-4.08069689719269,-0.00446774860307798,
-28.2603833427922));
#29167=CARTESIAN_POINT('',(1.05868926563988,-3.94542799184308,-28.0000001371954));
#29168=CARTESIAN_POINT('Origin',(0.,0.,-28.));
#29169=CARTESIAN_POINT('',(-4.08499944003493,0.00213890492626102,-28.3646150285541));
#29170=CARTESIAN_POINT('Ctrl Pts',(1.05868926563988,-3.94542799184308,-28.0000001371954));
#29171=CARTESIAN_POINT('Ctrl Pts',(0.944487741664465,-3.97607205068852,
-28.0057918022596));
#29172=CARTESIAN_POINT('Ctrl Pts',(0.828763515936965,-4.00180483333926,
-28.0115834673238));
#29173=CARTESIAN_POINT('Ctrl Pts',(0.71197907953204,-4.02247570412908,-28.0173751323881));
#29174=CARTESIAN_POINT('Ctrl Pts',(0.595339831784719,-4.04312087649474,
-28.0231595971429));
#29175=CARTESIAN_POINT('Ctrl Pts',(0.477643397790502,-4.05871657973845,
-28.0289440618977));
#29176=CARTESIAN_POINT('Ctrl Pts',(0.359366687456463,-4.06916214765971,
-28.0347285266525));
#29177=CARTESIAN_POINT('Ctrl Pts',(0.241205292609614,-4.07959753153247,
-28.0405073517648));
#29178=CARTESIAN_POINT('Ctrl Pts',(0.122465156075204,-4.08489273104913,
-28.046286176877));
#29179=CARTESIAN_POINT('Ctrl Pts',(0.00363196429894841,-4.08499838541404,
-28.0520650019893));
#29180=CARTESIAN_POINT('Ctrl Pts',(-0.115120392989385,-4.08510396790916,
-28.0578398961428));
#29181=CARTESIAN_POINT('Ctrl Pts',(-0.233965267613007,-4.08002702667372,
-28.0636147902964));
#29182=CARTESIAN_POINT('Ctrl Pts',(-0.352413915646341,-4.06977019401081,
-28.06938968445));
#29183=CARTESIAN_POINT('Ctrl Pts',(-0.470820428073106,-4.05951700999965,
-28.0751625243068));
#29184=CARTESIAN_POINT('Ctrl Pts',(-0.588830582873998,-4.04408763321666,
-28.0809353641637));
#29185=CARTESIAN_POINT('Ctrl Pts',(-0.705958295995525,-4.02353673828326,
-28.0867082040205));
#29186=CARTESIAN_POINT('Ctrl Pts',(-0.823072782862149,-4.00298816399088,
-28.0924803919987));
#29187=CARTESIAN_POINT('Ctrl Pts',(-0.939304619208435,-3.97731929313919,
-28.098252579977));
#29188=CARTESIAN_POINT('Ctrl Pts',(-1.05417618725878,-3.94663623434141,
-28.1040247679552));
#29189=CARTESIAN_POINT('Ctrl Pts',(-1.16906267583302,-3.91594919015961,
-28.1097977056757));
#29190=CARTESIAN_POINT('Ctrl Pts',(-1.28258814568584,-3.88024677034843,
-28.1155706433962));
#29191=CARTESIAN_POINT('Ctrl Pts',(-1.39428914366026,-3.83968524541676,
-28.1213435811166));
#29192=CARTESIAN_POINT('Ctrl Pts',(-1.50609908259559,-3.79908416120108,
-28.1271221491305));
#29193=CARTESIAN_POINT('Ctrl Pts',(-1.61608060651625,-3.75361464786899,
-28.1329007171443));
#29194=CARTESIAN_POINT('Ctrl Pts',(-1.7237891450077,-3.70348160297221,-28.1386792851581));
#29195=CARTESIAN_POINT('Ctrl Pts',(-1.83155109714163,-3.65332369664314,
-28.1444607188162));
#29196=CARTESIAN_POINT('Ctrl Pts',(-1.9370374518408,-3.59849784256731,-28.1502421524744));
#29197=CARTESIAN_POINT('Ctrl Pts',(-2.03982878353896,-3.53925465795356,
-28.1560235861326));
#29198=CARTESIAN_POINT('Ctrl Pts',(-2.14278062254969,-3.47991896588618,
-28.1618140474234));
#29199=CARTESIAN_POINT('Ctrl Pts',(-2.24302868230147,-3.41615238495911,
-28.1676045087141));
#29200=CARTESIAN_POINT('Ctrl Pts',(-2.34018264791322,-3.34824882205697,
-28.1733949700049));
#29201=CARTESIAN_POINT('Ctrl Pts',(-2.42368245807194,-3.28988852172617,
-28.1783716316931));
#29202=CARTESIAN_POINT('Ctrl Pts',(-2.50489715596483,-3.22847315025996,
-28.1833482933813));
#29203=CARTESIAN_POINT('Ctrl Pts',(-2.58359992194831,-3.16421182023402,
-28.1883249550694));
#29204=CARTESIAN_POINT('Ctrl Pts',(-2.67469731745531,-3.08983019305706,
-28.1940853741912));
#29205=CARTESIAN_POINT('Ctrl Pts',(-2.76273867255094,-3.01138150679804,
-28.199845793313));
#29206=CARTESIAN_POINT('Ctrl Pts',(-2.84733401246239,-2.92914902684633,
-28.2056062124348));
#29207=CARTESIAN_POINT('Ctrl Pts',(-2.9318248531792,-2.84701812728827,-28.2113595158082));
#29208=CARTESIAN_POINT('Ctrl Pts',(-3.01287784470125,-2.76111301561177,
-28.2171128191815));
#29209=CARTESIAN_POINT('Ctrl Pts',(-3.09013500250625,-2.67175797299937,
-28.2228661225549));
#29210=CARTESIAN_POINT('Ctrl Pts',(-3.16944536336043,-2.58002821131674,
-28.2287723269715));
#29211=CARTESIAN_POINT('Ctrl Pts',(-3.2447549366599,-2.48466283089649,-28.2346785313882));
#29212=CARTESIAN_POINT('Ctrl Pts',(-3.31571541134042,-2.38605454904108,
-28.2405847358048));
#29213=CARTESIAN_POINT('Ctrl Pts',(-3.38472557811072,-2.29015645920428,
-28.2463286115836));
#29214=CARTESIAN_POINT('Ctrl Pts',(-3.44962232801767,-2.19119176343797,
-28.2520724873625));
#29215=CARTESIAN_POINT('Ctrl Pts',(-3.5101256581818,-2.0895556618032,-28.2578163631413));
#29216=CARTESIAN_POINT('Ctrl Pts',(-3.5706092748088,-1.98795267581772,-28.263558367418));
#29217=CARTESIAN_POINT('Ctrl Pts',(-3.62670210361944,-1.8836803731514,-28.2693003716948));
#29218=CARTESIAN_POINT('Ctrl Pts',(-3.67816803242041,-1.77716204249375,
-28.2750423759715));
#29219=CARTESIAN_POINT('Ctrl Pts',(-3.72963000019004,-1.67065190992864,
-28.2807839383198));
#29220=CARTESIAN_POINT('Ctrl Pts',(-3.7764655949168,-1.56189646994867,-28.286525500668));
#29221=CARTESIAN_POINT('Ctrl Pts',(-3.81848550066746,-1.45134195873763,
-28.2922670630163));
#29222=CARTESIAN_POINT('Ctrl Pts',(-3.86260901195734,-1.3352528543852,-28.2982960601445));
#29223=CARTESIAN_POINT('Ctrl Pts',(-3.90142197438789,-1.2171803472074,-28.3043250572726));
#29224=CARTESIAN_POINT('Ctrl Pts',(-3.93476355908691,-1.09766148428454,
-28.3103540544008));
#29225=CARTESIAN_POINT('Ctrl Pts',(-3.96655034192614,-0.983716086211329,
-28.316101904246));
#29226=CARTESIAN_POINT('Ctrl Pts',(-3.99336447619579,-0.868456616329263,
-28.3218497540911));
#29227=CARTESIAN_POINT('Ctrl Pts',(-4.0151189006144,-0.75235976362975,-28.3275976039363));
#29228=CARTESIAN_POINT('Ctrl Pts',(-4.03688549258311,-0.636197976356727,
-28.3333486686334));
#29229=CARTESIAN_POINT('Ctrl Pts',(-4.0535866823057,-0.51919828700352,-28.3390997333304));
#29230=CARTESIAN_POINT('Ctrl Pts',(-4.06518723530116,-0.401842931933019,
-28.3448507980274));
#29231=CARTESIAN_POINT('Ctrl Pts',(-4.07680234166089,-0.284340349809415,
-28.3506090776683));
#29232=CARTESIAN_POINT('Ctrl Pts',(-4.0833040231341,-0.166481627636198,
-28.3563673573093));
#29233=CARTESIAN_POINT('Ctrl Pts',(-4.08470910919766,-0.0487492896119779,
-28.3621256369502));
#29234=CARTESIAN_POINT('Ctrl Pts',(-4.08491158920137,-0.0317834646288076,
-28.3629554341515));
#29235=CARTESIAN_POINT('Ctrl Pts',(-4.085008319848,-0.0148202553170852,
-28.3637852313528));
#29236=CARTESIAN_POINT('Ctrl Pts',(-4.08499944003493,0.00213890492626079,
-28.3646150285541));
#29237=CARTESIAN_POINT('Ctrl Pts',(-4.08499944003449,0.00213890577315302,
-28.3646150285955));
#29238=CARTESIAN_POINT('Ctrl Pts',(-4.08492707917895,0.140337632456191,
-28.3713769740561));
#29239=CARTESIAN_POINT('Ctrl Pts',(-4.07784209632971,0.278340655571587,
-28.3781389195167));
#29240=CARTESIAN_POINT('Ctrl Pts',(-4.06380108016489,0.415626973199183,
-28.3849008649773));
#29241=CARTESIAN_POINT('Ctrl Pts',(-4.05171852571603,0.533764392054479,
-28.3907196442771));
#29242=CARTESIAN_POINT('Ctrl Pts',(-4.03446041943139,0.651567788878492,
-28.3965384235768));
#29243=CARTESIAN_POINT('Ctrl Pts',(-4.01205176362136,0.768547751296376,
-28.4023572028766));
#29244=CARTESIAN_POINT('Ctrl Pts',(-3.98967159419813,0.885379006157445,
-28.4081685852134));
#29245=CARTESIAN_POINT('Ctrl Pts',(-3.96215397380015,1.00138851032704,-28.4139799675502));
#29246=CARTESIAN_POINT('Ctrl Pts',(-3.92957571838599,1.11609124782484,-28.419791349887));
#29247=CARTESIAN_POINT('Ctrl Pts',(-3.89703034532761,1.23067821189725,-28.4255968665953));
#29248=CARTESIAN_POINT('Ctrl Pts',(-3.85943460944823,1.34396064186545,-28.4314023833036));
#29249=CARTESIAN_POINT('Ctrl Pts',(-3.8169163835786,1.45546361025252,-28.437207900012));
#29250=CARTESIAN_POINT('Ctrl Pts',(-3.77289175927167,1.57091707031454,-28.4432191031317));
#29251=CARTESIAN_POINT('Ctrl Pts',(-3.72358945971961,1.68446220186831,-28.4492303062514));
#29252=CARTESIAN_POINT('Ctrl Pts',(-3.6692079963623,1.79558839365567,-28.4552415093711));
#29253=CARTESIAN_POINT('Ctrl Pts',(-3.61674721143371,1.90278976131629,-28.4610404050712));
#29254=CARTESIAN_POINT('Ctrl Pts',(-3.55956016589634,2.00773976713687,-28.4668393007712));
#29255=CARTESIAN_POINT('Ctrl Pts',(-3.49787380820038,2.11000090566468,-28.4726381964713));
#29256=CARTESIAN_POINT('Ctrl Pts',(-3.43619685151291,2.21224645958241,-28.4784362084189));
#29257=CARTESIAN_POINT('Ctrl Pts',(-3.37002215752528,2.31180361090308,-28.4842342203666));
#29258=CARTESIAN_POINT('Ctrl Pts',(-3.29962169624125,2.40826112821969,-28.4900322323142));
#29259=CARTESIAN_POINT('Ctrl Pts',(-3.22921527113157,2.50472681673015,-28.4958307354281));
#29260=CARTESIAN_POINT('Ctrl Pts',(-3.15458260825463,2.59809201874398,-28.501629238542));
#29261=CARTESIAN_POINT('Ctrl Pts',(-3.0760375138906,2.68797660204433,-28.5074277416559));
#29262=CARTESIAN_POINT('Ctrl Pts',(-2.99746714174169,2.777890112462,-28.5132281108738));
#29263=CARTESIAN_POINT('Ctrl Pts',(-2.91498210321149,2.86432046866093,-28.5190284800917));
#29264=CARTESIAN_POINT('Ctrl Pts',(-2.82893432733294,2.94692306849658,-28.5248288493096));
#29265=CARTESIAN_POINT('Ctrl Pts',(-2.74279167424872,3.02961674684965,-28.5306356140772));
#29266=CARTESIAN_POINT('Ctrl Pts',(-2.65307873813565,3.10847396111878,-28.5364423788448));
#29267=CARTESIAN_POINT('Ctrl Pts',(-2.56018201574489,3.18318913139896,-28.5422491436123));
#29268=CARTESIAN_POINT('Ctrl Pts',(-2.46722428548866,3.25795336921283,-28.5480597218441));
#29269=CARTESIAN_POINT('Ctrl Pts',(-2.37107893407291,3.32856990437002,-28.5538703000758));
#29270=CARTESIAN_POINT('Ctrl Pts',(-2.27216165718837,3.39477634073336,-28.5596808783076));
#29271=CARTESIAN_POINT('Ctrl Pts',(-2.17310342341672,3.46107712111294,-28.5654997365996));
#29272=CARTESIAN_POINT('Ctrl Pts',(-2.07126572900084,3.52295504848583,-28.5713185948917));
#29273=CARTESIAN_POINT('Ctrl Pts',(-1.96708915965088,3.58019346376477,-28.5771374531838));
#29274=CARTESIAN_POINT('Ctrl Pts',(-1.94119314904434,3.5944216785967,-28.5785838937509));
#29275=CARTESIAN_POINT('Ctrl Pts',(-1.91515271299772,3.60836344604473,-28.580030334318));
#29276=CARTESIAN_POINT('Ctrl Pts',(-1.88897479802175,3.6220159044983,-28.5814767748851));
#29277=CARTESIAN_POINT('Ctrl Pts',(-1.78352022539363,3.67701318647691,-28.587303586225));
#29278=CARTESIAN_POINT('Ctrl Pts',(-1.67549364854706,3.72748889979843,-28.5931303975648));
#29279=CARTESIAN_POINT('Ctrl Pts',(-1.56531918384874,3.77319504567086,-28.5989572089047));
#29280=CARTESIAN_POINT('Ctrl Pts',(-1.45528287044541,3.81884387914101,-28.6047767138189));
#29281=CARTESIAN_POINT('Ctrl Pts',(-1.34310439969314,3.859734886133,-28.6105962187331));
#29282=CARTESIAN_POINT('Ctrl Pts',(-1.2292325975245,3.8956658251425,-28.6164157236474));
#29283=CARTESIAN_POINT('Ctrl Pts',(-1.11547400212432,3.93156104305672,-28.6222294430437));
#29284=CARTESIAN_POINT('Ctrl Pts',(-1.00002581111627,3.96250588109683,-28.6280431624401));
#29285=CARTESIAN_POINT('Ctrl Pts',(-0.883356399224285,3.98834633299937,
-28.6338568818365));
#29286=CARTESIAN_POINT('Ctrl Pts',(-0.762784994606225,4.01505101532637,
-28.639865040293));
#29287=CARTESIAN_POINT('Ctrl Pts',(-0.640909659491408,4.03630372418732,
-28.6458731987495));
#29288=CARTESIAN_POINT('Ctrl Pts',(-0.518264356245074,4.05199050554735,
-28.651881357206));
#29289=CARTESIAN_POINT('Ctrl Pts',(-0.399720308404025,4.06715272139088,
-28.657688603017));
#29290=CARTESIAN_POINT('Ctrl Pts',(-0.280457401269083,4.0771152535832,-28.6634958488279));
#29291=CARTESIAN_POINT('Ctrl Pts',(-0.160967062866826,4.08182736095882,
-28.6693030946388));
#29292=CARTESIAN_POINT('Ctrl Pts',(-0.041494082617508,4.08653878381482,
-28.6751094968412));
#29293=CARTESIAN_POINT('Ctrl Pts',(0.078205855823146,4.08600128267971,-28.6809158990437));
#29294=CARTESIAN_POINT('Ctrl Pts',(0.197638558319185,4.08021617077643,-28.6867223012462));
#29295=CARTESIAN_POINT('Ctrl Pts',(0.317082004084967,4.07443053848791,-28.692529225749));
#29296=CARTESIAN_POINT('Ctrl Pts',(0.43625775877849,4.0633963766382,-28.6983361502518));
#29297=CARTESIAN_POINT('Ctrl Pts',(0.554674625996545,4.04716704118765,-28.7041430747546));
#29298=CARTESIAN_POINT('Ctrl Pts',(0.673129998971635,4.03093242842431,-28.7099518875022));
#29299=CARTESIAN_POINT('Ctrl Pts',(0.790825589889218,4.00949933765131,-28.7157607002497));
#29300=CARTESIAN_POINT('Ctrl Pts',(0.907278924941074,3.98297250208406,-28.7215695129973));
#29301=CARTESIAN_POINT('Ctrl Pts',(1.02386029044877,3.95641650253582,-28.7273847120363));
#29302=CARTESIAN_POINT('Ctrl Pts',(1.13919627614658,3.92475567064944,-28.7331999110754));
#29303=CARTESIAN_POINT('Ctrl Pts',(1.2528179897162,3.88814506990717,-28.7390151101144));
#29304=CARTESIAN_POINT('Ctrl Pts',(1.36651429963588,3.8515104331149,-28.7448341270207));
#29305=CARTESIAN_POINT('Ctrl Pts',(1.47849371455021,3.80991969708604,-28.7506531439271));
#29306=CARTESIAN_POINT('Ctrl Pts',(1.58830733071757,3.76357606847382,-28.7564721608334));
#29307=CARTESIAN_POINT('Ctrl Pts',(1.69827612786726,3.71716695026145,-28.7622994007706));
#29308=CARTESIAN_POINT('Ctrl Pts',(1.80607265072477,3.6659917084866,-28.7681266407079));
#29309=CARTESIAN_POINT('Ctrl Pts',(1.911272482402,3.61029950253617,-28.7739538806451));
#29310=CARTESIAN_POINT('Ctrl Pts',(1.93593787637183,3.5972417801148,-28.7753201486944));
#29311=CARTESIAN_POINT('Ctrl Pts',(1.96046065045553,3.58393593536615,-28.7766864167436));
#29312=CARTESIAN_POINT('Ctrl Pts',(1.98483557515258,3.57038551694474,-28.7780526847929));
#29313=CARTESIAN_POINT('Ctrl Pts',(2.08876992332173,3.51260671665906,-28.7838784332163));
#29314=CARTESIAN_POINT('Ctrl Pts',(2.19034481944784,3.45019380377238,-28.7897041816397));
#29315=CARTESIAN_POINT('Ctrl Pts',(2.2891200188456,3.38336438169469,-28.7955299300632));
#29316=CARTESIAN_POINT('Ctrl Pts',(2.35644383584311,3.33781436702057,-28.7995006800401));
#29317=CARTESIAN_POINT('Ctrl Pts',(2.42246738896646,3.2902136388328,-28.8034714300171));
#29318=CARTESIAN_POINT('Ctrl Pts',(2.48705727606859,3.24064362520075,-28.807442179994));
#29319=CARTESIAN_POINT('Origin',(0.,0.,0.));
#29320=CARTESIAN_POINT('',(-1.30343164629623,3.1291326283706,-38.999956889224));
#29321=CARTESIAN_POINT('',(-2.89372837779137,-1.76542944862289,-39.));
#29322=CARTESIAN_POINT('Origin',(0.,0.,-39.));
#29323=CARTESIAN_POINT('',(-3.38974897938027,0.00263045440945954,-38.7660178032496));
#29324=CARTESIAN_POINT('Ctrl Pts',(-1.30343164629623,3.1291326283706,-38.999956889224));
#29325=CARTESIAN_POINT('Ctrl Pts',(-1.39833027824498,3.08960286253366,-38.99388871478));
#29326=CARTESIAN_POINT('Ctrl Pts',(-1.49159532416278,3.04568278774804,-38.987820540336));
#29327=CARTESIAN_POINT('Ctrl Pts',(-1.58278977870312,2.9975292457177,-38.9817523658921));
#29328=CARTESIAN_POINT('Ctrl Pts',(-1.67386612085234,2.94943807074705,-38.9756920507702));
#29329=CARTESIAN_POINT('Ctrl Pts',(-1.76287682226379,2.89712452704605,-38.9696317356483));
#29330=CARTESIAN_POINT('Ctrl Pts',(-1.84940424216492,2.84079372914726,-38.9635714205265));
#29331=CARTESIAN_POINT('Ctrl Pts',(-1.93976809019622,2.78196535235498,-38.9572424048767));
#29332=CARTESIAN_POINT('Ctrl Pts',(-2.02742291519195,2.71875542496574,-38.9509133892268));
#29333=CARTESIAN_POINT('Ctrl Pts',(-2.11192072102072,2.65145166477221,-38.944584373577));
#29334=CARTESIAN_POINT('Ctrl Pts',(-2.19269466403182,2.5871140167471,-38.9385342809811));
#29335=CARTESIAN_POINT('Ctrl Pts',(-2.2705835622744,2.51903600965155,-38.9324841883852));
#29336=CARTESIAN_POINT('Ctrl Pts',(-2.34522613869442,2.44751290515177,-38.9264340957893));
#29337=CARTESIAN_POINT('Ctrl Pts',(-2.41984501993697,2.37601250555763,-38.9203859237864));
#29338=CARTESIAN_POINT('Ctrl Pts',(-2.49121931485692,2.30106948112322,-38.9143377517836));
#29339=CARTESIAN_POINT('Ctrl Pts',(-2.55902268804625,2.2230177562414,-38.9082895797808));
#29340=CARTESIAN_POINT('Ctrl Pts',(-2.62682261012922,2.14497000409414,-38.9022417156224));
#29341=CARTESIAN_POINT('Ctrl Pts',(-2.69105168836955,2.06381419339159,-38.8961938514639));
#29342=CARTESIAN_POINT('Ctrl Pts',(-2.75142282563774,1.9799185581886,-38.8901459873054));
#29343=CARTESIAN_POINT('Ctrl Pts',(-2.81180698217444,1.89600483056843,-38.8840968189018));
#29344=CARTESIAN_POINT('Ctrl Pts',(-2.86833129250096,1.80935045635071,-38.8780476504981));
#29345=CARTESIAN_POINT('Ctrl Pts',(-2.92075163866745,1.72035314041083,-38.8719984820944));
#29346=CARTESIAN_POINT('Ctrl Pts',(-2.97322659162087,1.63126311509713,-38.8659430122128));
#29347=CARTESIAN_POINT('Ctrl Pts',(-3.02158882850242,1.53982565066671,-38.8598875423313));
#29348=CARTESIAN_POINT('Ctrl Pts',(-3.0656400215595,1.44646338381332,-38.8538320724498));
#29349=CARTESIAN_POINT('Ctrl Pts',(-3.10971820406863,1.35304391541214,-38.84777289248));
#29350=CARTESIAN_POINT('Ctrl Pts',(-3.14947991874989,1.25769769613465,-38.8417137125102));
#29351=CARTESIAN_POINT('Ctrl Pts',(-3.18477558775203,1.16086584847635,-38.8356545325404));
#29352=CARTESIAN_POINT('Ctrl Pts',(-3.22012294762422,1.06389218958184,-38.8295864788393));
#29353=CARTESIAN_POINT('Ctrl Pts',(-3.25099108070739,0.965428972501001,
-38.8235184251381));
#29354=CARTESIAN_POINT('Ctrl Pts',(-3.27728073635541,0.865930734882268,
-38.817450371437));
#29355=CARTESIAN_POINT('Ctrl Pts',(-3.28562121105491,0.834364610752882,
-38.8155252626015));
#29356=CARTESIAN_POINT('Ctrl Pts',(-3.29350125325975,0.802694372619393,
-38.813600153766));
#29357=CARTESIAN_POINT('Ctrl Pts',(-3.30091878121429,0.770934668001608,
-38.8116750449306));
#29358=CARTESIAN_POINT('Ctrl Pts',(-3.33201007028159,0.637810780499659,
-38.8036057642138));
#29359=CARTESIAN_POINT('Ctrl Pts',(-3.35505703564748,0.5027501102116,-38.7955364834971));
#29360=CARTESIAN_POINT('Ctrl Pts',(-3.36986949869865,0.366585084585444,
-38.7874672027803));
#29361=CARTESIAN_POINT('Ctrl Pts',(-3.3829941066685,0.245935833048101,-38.7803174029367));
#29362=CARTESIAN_POINT('Ctrl Pts',(-3.38965447070927,0.12441955287756,-38.7731676030932));
#29363=CARTESIAN_POINT('Ctrl Pts',(-3.38974897938027,0.00263045440945954,
-38.7660178032496));
#29364=CARTESIAN_POINT('',(-3.38517229864742,-0.00153545903651936,-37.5160178032496));
#29365=CARTESIAN_POINT('Ctrl Pts',(-3.38956806600938,0.0026303140201922,
-38.7660178032496));
#29366=CARTESIAN_POINT('Ctrl Pts',(-3.38196169697795,-0.854242402898206,
-38.7157115805073));
#29367=CARTESIAN_POINT('Ctrl Pts',(-2.62050801171528,-2.83865004984225,
-38.5998800544626));
#29368=CARTESIAN_POINT('Ctrl Pts',(0.699092616145842,-3.93244007385531,
-38.4185232251148));
#29369=CARTESIAN_POINT('Ctrl Pts',(3.66779171704377,-1.58009583571682,-38.2219473152072));
#29370=CARTESIAN_POINT('Ctrl Pts',(3.33787025741108,2.1929856073312,-38.0253714052993));
#29371=CARTESIAN_POINT('Ctrl Pts',(0.00554946209745111,3.99384108558651,
-37.8287954953915));
#29372=CARTESIAN_POINT('Ctrl Pts',(-2.87684185453993,2.44650803385519,-37.659010961375));
#29373=CARTESIAN_POINT('Ctrl Pts',(-3.38241331840635,0.660535797814238,
-37.5547517306609));
#29374=CARTESIAN_POINT('Ctrl Pts',(-3.38517229864742,-0.00153545903651936,
-37.5160178032496));
#29375=CARTESIAN_POINT('',(-3.38974885847844,0.0027818957803985,-35.0146790786306));
#29376=CARTESIAN_POINT('Ctrl Pts',(-3.38974971482863,-0.00139043850725259,
-37.5133796950408));
#29377=CARTESIAN_POINT('Ctrl Pts',(-3.38963540845987,-0.280057908424469,
-37.4978425875729));
#29378=CARTESIAN_POINT('Ctrl Pts',(-3.35516103288601,-0.557648974801886,
-37.4833830197543));
#29379=CARTESIAN_POINT('Ctrl Pts',(-3.25561678295251,-0.952875792877547,
-37.4615574925989));
#29380=CARTESIAN_POINT('Ctrl Pts',(-3.21704324491428,-1.07593653096365,
-37.4545556953373));
#29381=CARTESIAN_POINT('Ctrl Pts',(-3.16085149518451,-1.22488526578853,
-37.4455004378842));
#29382=CARTESIAN_POINT('Ctrl Pts',(-3.14975886689697,-1.25313408462521,
-37.4437563425721));
#29383=CARTESIAN_POINT('Ctrl Pts',(-3.13118482705633,-1.29863000893447,
-37.4408981292982));
#29384=CARTESIAN_POINT('Ctrl Pts',(-3.12393634803657,-1.31597111737372,
-37.4397969630444));
#29385=CARTESIAN_POINT('Ctrl Pts',(-3.10909088499153,-1.35067317583879,
-37.4375680137118));
#29386=CARTESIAN_POINT('Ctrl Pts',(-3.10149179434903,-1.36803244507079,
-37.436440149866));
#29387=CARTESIAN_POINT('Ctrl Pts',(-3.08104545250067,-1.41369375209662,
-37.4334411339879));
#29388=CARTESIAN_POINT('Ctrl Pts',(-3.06795406907797,-1.44188376329372,
-37.4315565766478));
#29389=CARTESIAN_POINT('Ctrl Pts',(-2.99128261356095,-1.60120959250344,
-37.4207324475503));
#29390=CARTESIAN_POINT('Ctrl Pts',(-2.91968998855778,-1.72830749538175,
-37.4114314136678));
#29391=CARTESIAN_POINT('Ctrl Pts',(-2.73788159051288,-2.00736348670642,
-37.3900152668832));
#29392=CARTESIAN_POINT('Ctrl Pts',(-2.62276765961903,-2.15559806704704,
-37.3779037505251));
#29393=CARTESIAN_POINT('Ctrl Pts',(-2.42333512627505,-2.37263183313778,
-37.3594093966504));
#29394=CARTESIAN_POINT('Ctrl Pts',(-2.34696086604114,-2.44820613917663,
-37.3527929769091));
#29395=CARTESIAN_POINT('Ctrl Pts',(-2.23539596463779,-2.54857430955382,
-37.3437582625166));
#29396=CARTESIAN_POINT('Ctrl Pts',(-2.20313382079788,-2.5765146507674,-37.3412133491296));
#29397=CARTESIAN_POINT('Ctrl Pts',(-2.14603341260647,-2.62410896963293,
-37.3368232030854));
#29398=CARTESIAN_POINT('Ctrl Pts',(-2.12143193505007,-2.64403743127729,
-37.3349671727457));
#29399=CARTESIAN_POINT('Ctrl Pts',(-2.0696393654739,-2.68480374906934,-37.3311310704333));
#29400=CARTESIAN_POINT('Ctrl Pts',(-2.04240425341824,-2.70558002341925,
-37.3291535184971));
#29401=CARTESIAN_POINT('Ctrl Pts',(-1.96930754881953,-2.75960889653867,
-37.3239463890803));
#29402=CARTESIAN_POINT('Ctrl Pts',(-1.92291852092737,-2.79213150784517,
-37.3207442956922));
#29403=CARTESIAN_POINT('Ctrl Pts',(-1.69126127141587,-2.94602946603464,
-37.3052071942986));
#29404=CARTESIAN_POINT('Ctrl Pts',(-1.49522021485583,-3.05020996918097,
-37.2934905946234));
#29405=CARTESIAN_POINT('Ctrl Pts',(-1.17115894301394,-3.18361758405139,
-37.2748888614377));
#29406=CARTESIAN_POINT('Ctrl Pts',(-1.04921620738403,-3.2258605134561,-37.2680344628154));
#29407=CARTESIAN_POINT('Ctrl Pts',(-0.856542246070162,-3.28052274294266,
-37.2570449311983));
#29408=CARTESIAN_POINT('Ctrl Pts',(-0.787320272462905,-3.29782041749641,
-37.2530650195709));
#29409=CARTESIAN_POINT('Ctrl Pts',(-0.692464501908122,-3.31836705228204,
-37.24750650796));
#29410=CARTESIAN_POINT('Ctrl Pts',(-0.667259489825077,-3.32352699212036,
-37.2460195384264));
#29411=CARTESIAN_POINT('Ctrl Pts',(-0.624385947828445,-3.33179666432789,
-37.2434696442412));
#29412=CARTESIAN_POINT('Ctrl Pts',(-0.606747255388106,-3.33505390999365,
-37.2424146452682));
#29413=CARTESIAN_POINT('Ctrl Pts',(-0.568902731844816,-3.34173228415333,
-37.240137255103));
#29414=CARTESIAN_POINT('Ctrl Pts',(-0.548691396713423,-3.34511026448881,
-37.2389128053741));
#29415=CARTESIAN_POINT('Ctrl Pts',(-0.491488497042306,-3.35413839860511,
-37.2354266033609));
#29416=CARTESIAN_POINT('Ctrl Pts',(-0.45443327077754,-3.35935938769356,
-37.233143893227));
#29417=CARTESIAN_POINT('Ctrl Pts',(-0.278234446005362,-3.3812169021349,
-37.2221975052339));
#29418=CARTESIAN_POINT('Ctrl Pts',(-0.13824217771398,-3.38982673429237,
-37.2132344463832));
#29419=CARTESIAN_POINT('Ctrl Pts',(0.180879260881719,-3.38965078839984,
-37.1927027217061));
#29420=CARTESIAN_POINT('Ctrl Pts',(0.359613646406424,-3.37537199890944,
-37.181142917244));
#29421=CARTESIAN_POINT('Ctrl Pts',(0.643743779185407,-3.32983775579119,
-37.1630773731505));
#29422=CARTESIAN_POINT('Ctrl Pts',(0.750213658200293,-3.30747770784222,
-37.156375013297));
#29423=CARTESIAN_POINT('Ctrl Pts',(0.896894210673183,-3.2692234156588,-37.1472471643914));
#29424=CARTESIAN_POINT('Ctrl Pts',(0.938147434880559,-3.25762499498695,
-37.1446915064063));
#29425=CARTESIAN_POINT('Ctrl Pts',(1.00950729334849,-3.23609396502341,-37.1402888758628));
#29426=CARTESIAN_POINT('Ctrl Pts',(1.039714347059,-3.22651565982465,-37.1384309341173));
#29427=CARTESIAN_POINT('Ctrl Pts',(1.10222659122524,-3.20572465957939,-37.1345963158099));
#29428=CARTESIAN_POINT('Ctrl Pts',(1.13450544613777,-3.19444385877272,-37.132622076957));
#29429=CARTESIAN_POINT('Ctrl Pts',(1.21948563729376,-3.1632943971537,-37.1274364308162));
#29430=CARTESIAN_POINT('Ctrl Pts',(1.27187298856821,-3.14259705765547,-37.1242520709946));
#29431=CARTESIAN_POINT('Ctrl Pts',(1.53312660093978,-3.0317764030757,-37.1083940019937));
#29432=CARTESIAN_POINT('Ctrl Pts',(1.73306040307067,-2.92209806939385,-37.096379427684));
#29433=CARTESIAN_POINT('Ctrl Pts',(2.02362355231975,-2.72231711417247,-37.0776567639117));
#29434=CARTESIAN_POINT('Ctrl Pts',(2.12272344425099,-2.64577108350339,-37.0709964134981));
#29435=CARTESIAN_POINT('Ctrl Pts',(2.27038593574331,-2.51806823261727,-37.0602758875193));
#29436=CARTESIAN_POINT('Ctrl Pts',(2.3219736320467,-2.47057828583941,-37.0563619986539));
#29437=CARTESIAN_POINT('Ctrl Pts',(2.39032007572925,-2.40362834051028,-37.050881193941));
#29438=CARTESIAN_POINT('Ctrl Pts',(2.40838795298934,-2.38552439665988,-37.0494025962997));
#29439=CARTESIAN_POINT('Ctrl Pts',(2.4387613683404,-2.35439357229379,-37.0468622450008));
#29440=CARTESIAN_POINT('Ctrl Pts',(2.45117145587889,-2.3414706038599,-37.0458082567081));
#29441=CARTESIAN_POINT('Ctrl Pts',(2.4776081814976,-2.31350077822359,-37.0435271392372));
#29442=CARTESIAN_POINT('Ctrl Pts',(2.49160055708871,-2.29842440999425,-37.0422978618386));
#29443=CARTESIAN_POINT('Ctrl Pts',(2.53090583014691,-2.25529344460598,-37.0387843399938));
#29444=CARTESIAN_POINT('Ctrl Pts',(2.55588732691935,-2.22694242434155,-37.0364786491366));
#29445=CARTESIAN_POINT('Ctrl Pts',(2.67702066273505,-2.08474709737769,-37.024958165882));
#29446=CARTESIAN_POINT('Ctrl Pts',(2.7660607728452,-1.96507283719963,-37.0154051702325));
#29447=CARTESIAN_POINT('Ctrl Pts',(2.92058453359913,-1.72597881861116,-36.9970778900346));
#29448=CARTESIAN_POINT('Ctrl Pts',(2.98733039815867,-1.60769301421061,-36.9883260596764));
#29449=CARTESIAN_POINT('Ctrl Pts',(3.08689678282724,-1.40350959963229,-36.9739255933961));
#29450=CARTESIAN_POINT('Ctrl Pts',(3.12364412436115,-1.31970463846546,-36.9681994225809));
#29451=CARTESIAN_POINT('Ctrl Pts',(3.18206775740662,-1.17030049618221,-36.958332226596));
#29452=CARTESIAN_POINT('Ctrl Pts',(3.20521317281995,-1.10533614854875,-36.9541500786922));
#29453=CARTESIAN_POINT('Ctrl Pts',(3.23760283507773,-1.00482634346251,-36.9478416790135));
#29454=CARTESIAN_POINT('Ctrl Pts',(3.24827728849505,-0.969764359213442,
-36.9456705258882));
#29455=CARTESIAN_POINT('Ctrl Pts',(3.26612683571896,-0.907529530516667,
-36.9418669513655));
#29456=CARTESIAN_POINT('Ctrl Pts',(3.27353642503602,-0.880428134212425,
-36.9402272215186));
#29457=CARTESIAN_POINT('Ctrl Pts',(3.28994593809484,-0.817335256605636,
-36.9364468937442));
#29458=CARTESIAN_POINT('Ctrl Pts',(3.2986937525358,-0.781281561849035,-36.9343144044559));
#29459=CARTESIAN_POINT('Ctrl Pts',(3.32205393578808,-0.67760478434035,-36.928256036336));
#29460=CARTESIAN_POINT('Ctrl Pts',(3.33519086007305,-0.609666638926558,
-36.9243757263973));
#29461=CARTESIAN_POINT('Ctrl Pts',(3.38593130831218,-0.296037321377273,
-36.9067957535624));
#29462=CARTESIAN_POINT('Ctrl Pts',(3.39852253502943,-0.0470894588677387,
-36.8938370785724));
#29463=CARTESIAN_POINT('Ctrl Pts',(3.37613239024138,0.329834739874389,-36.8736691421433));
#29464=CARTESIAN_POINT('Ctrl Pts',(3.36112902024774,0.458112252655445,-36.8666926566614));
#29465=CARTESIAN_POINT('Ctrl Pts',(3.33255306525874,0.621149297998841,-36.8573479236848));
#29466=CARTESIAN_POINT('Ctrl Pts',(3.32567426244639,0.656983149682284,-36.8552638049035));
#29467=CARTESIAN_POINT('Ctrl Pts',(3.31411472531476,0.712356635612162,-36.851986628945));
#29468=CARTESIAN_POINT('Ctrl Pts',(3.30983623744387,0.731978432981562,-36.8508142461076));
#29469=CARTESIAN_POINT('Ctrl Pts',(3.30142031677509,0.76899188285912,-36.8485797427721));
#29470=CARTESIAN_POINT('Ctrl Pts',(3.2973192564117,0.786390672315879,-36.8475195568989));
#29471=CARTESIAN_POINT('Ctrl Pts',(3.28781378529916,0.825335699727807,-36.845125362408));
#29472=CARTESIAN_POINT('Ctrl Pts',(3.28233480387825,0.846862847541506,-36.8437874592787));
#29473=CARTESIAN_POINT('Ctrl Pts',(3.26195011065856,0.923784172914644,-36.8389585648473));
#29474=CARTESIAN_POINT('Ctrl Pts',(3.24585105380082,0.978849263470516,-36.835411755264));
#29475=CARTESIAN_POINT('Ctrl Pts',(3.14671399007535,1.28853281277306,-36.8150489715525));
#29476=CARTESIAN_POINT('Ctrl Pts',(3.03512728580681,1.53301667217336,-36.7974540857716));
#29477=CARTESIAN_POINT('Ctrl Pts',(2.83127818513881,1.86808407053455,-36.7726834517822));
#29478=CARTESIAN_POINT('Ctrl Pts',(2.76082995469431,1.97070996222896,-36.7649766481907));
#29479=CARTESIAN_POINT('Ctrl Pts',(2.65764289395974,2.10459782470753,-36.7547785215423));
#29480=CARTESIAN_POINT('Ctrl Pts',(2.62969640471604,2.13941460640223,-36.7521117654725));
#29481=CARTESIAN_POINT('Ctrl Pts',(2.58057133996229,2.19819890626915,-36.7475814060649));
#29482=CARTESIAN_POINT('Ctrl Pts',(2.55972693292132,2.22243672680613,-36.7457049822149));
#29483=CARTESIAN_POINT('Ctrl Pts',(2.51630172941993,2.27150984692276,-36.7418866949192));
#29484=CARTESIAN_POINT('Ctrl Pts',(2.49368863783129,2.29631192832581,-36.7399464504953));
#29485=CARTESIAN_POINT('Ctrl Pts',(2.43431512589236,2.35952131539616,-36.7349710953629));
#29486=CARTESIAN_POINT('Ctrl Pts',(2.3970122292564,2.39740771893907,-36.7319590102458));
#29487=CARTESIAN_POINT('Ctrl Pts',(2.15088632243893,2.63589321649151,-36.712758227023));
#29488=CARTESIAN_POINT('Ctrl Pts',(1.91799292279426,2.80990251898898,-36.6977432595635));
#29489=CARTESIAN_POINT('Ctrl Pts',(1.55314974567294,3.01576933811904,-36.6753127763765));
#29490=CARTESIAN_POINT('Ctrl Pts',(1.43695196584987,3.07283282443071,-36.6682858473396));
#29491=CARTESIAN_POINT('Ctrl Pts',(1.28980836909209,3.13491975252192,-36.6592018255467));
#29492=CARTESIAN_POINT('Ctrl Pts',(1.26166959434878,3.14634981889251,-36.6574564540419));
#29493=CARTESIAN_POINT('Ctrl Pts',(1.21587004403559,3.16424059868812,-36.6545966320535));
#29494=CARTESIAN_POINT('Ctrl Pts',(1.19830180062916,3.17093539698664,-36.6534951583886));
#29495=CARTESIAN_POINT('Ctrl Pts',(1.16291816173434,3.18408313651429,-36.6512660514002));
#29496=CARTESIAN_POINT('Ctrl Pts',(1.14510257695021,3.19053351675171,-36.6501383437206));
#29497=CARTESIAN_POINT('Ctrl Pts',(1.09793790533473,3.20716423215931,-36.6471405291085));
#29498=CARTESIAN_POINT('Ctrl Pts',(1.06850196797633,3.21709083682903,-36.6452570381004));
#29499=CARTESIAN_POINT('Ctrl Pts',(0.903354215304466,3.27026668065216,-36.6346362138455));
#29500=CARTESIAN_POINT('Ctrl Pts',(0.76516796330292,3.30532962305828,-36.6255538485042));
#29501=CARTESIAN_POINT('Ctrl Pts',(0.438688555273904,3.36659606322334,-36.604201646272));
#29502=CARTESIAN_POINT('Ctrl Pts',(0.24955235674908,3.38587506471536,-36.5919267647744));
#29503=CARTESIAN_POINT('Ctrl Pts',(-0.0482586469328648,3.39112874000251,
-36.573232101153));
#29504=CARTESIAN_POINT('Ctrl Pts',(-0.156343374508001,3.38786710198308,
-36.5665717655171));
#29505=CARTESIAN_POINT('Ctrl Pts',(-0.306730355255403,3.3761146722249,-36.5574893862273));
#29506=CARTESIAN_POINT('Ctrl Pts',(-0.349298503499069,3.37197636346342,
-36.5549389206137));
#29507=CARTESIAN_POINT('Ctrl Pts',(-0.423239823571647,3.36337276156537,
-36.5505422834501));
#29508=CARTESIAN_POINT('Ctrl Pts',(-0.454649092917693,3.35927113887308,
-36.5486852265698));
#29509=CARTESIAN_POINT('Ctrl Pts',(-0.519865078520934,3.34982335021355,
-36.54484977863));
#29510=CARTESIAN_POINT('Ctrl Pts',(-0.553657688208975,3.34440420177297,
-36.5428738656095));
#29511=CARTESIAN_POINT('Ctrl Pts',(-0.642986736253272,3.32868785719603,
-36.5376775800884));
#29512=CARTESIAN_POINT('Ctrl Pts',(-0.698358870837683,3.31751265083307,
-36.5344844687493));
#29513=CARTESIAN_POINT('Ctrl Pts',(-0.972632597582847,3.25498673347624,
-36.5187668276294));
#29514=CARTESIAN_POINT('Ctrl Pts',(-1.18632412308613,3.18333127265262,-36.5068832572459));
#29515=CARTESIAN_POINT('Ctrl Pts',(-1.50697620799302,3.0389970525262,-36.4882152280711));
#29516=CARTESIAN_POINT('Ctrl Pts',(-1.61957504954803,2.98051231352566,-36.4814707004853));
#29517=CARTESIAN_POINT('Ctrl Pts',(-1.78939514211345,2.87983692166256,-36.4706332817705));
#29518=CARTESIAN_POINT('Ctrl Pts',(-1.84901829541532,2.84192288414976,-36.4666905246977));
#29519=CARTESIAN_POINT('Ctrl Pts',(-1.92860798984674,2.7877470975686,-36.4611757219193));
#29520=CARTESIAN_POINT('Ctrl Pts',(-1.94964149379764,2.77307782418434,-36.4596934336464));
#29521=CARTESIAN_POINT('Ctrl Pts',(-1.98509225644066,2.74775092645692,-36.4571488777277));
#29522=CARTESIAN_POINT('Ctrl Pts',(-1.99959488379094,2.73721513790705,-36.4560944459888));
#29523=CARTESIAN_POINT('Ctrl Pts',(-2.0305309959958,2.71436375693765,-36.4538150025067));
#29524=CARTESIAN_POINT('Ctrl Pts',(-2.04693642275421,2.70201368700692,-36.4525878825084));
#29525=CARTESIAN_POINT('Ctrl Pts',(-2.09307938011474,2.66661569695726,-36.449086528822));
#29526=CARTESIAN_POINT('Ctrl Pts',(-2.12254597947455,2.64322130772275,-36.4467910663034));
#29527=CARTESIAN_POINT('Ctrl Pts',(-2.26415715591376,2.52689713479139,-36.4354902678453));
#29528=CARTESIAN_POINT('Ctrl Pts',(-2.37061544419424,2.42730154426324,-36.4261615471792));
#29529=CARTESIAN_POINT('Ctrl Pts',(-2.56435969262928,2.2211078204855,-36.4079504145397));
#29530=CARTESIAN_POINT('Ctrl Pts',(-2.6522246367592,2.11541198741061,-36.3990894847843));
#29531=CARTESIAN_POINT('Ctrl Pts',(-2.81460296825852,1.89400395431492,-36.3816750048194));
#29532=CARTESIAN_POINT('Ctrl Pts',(-2.88897867676167,1.77849665377634,-36.3731374462106));
#29533=CARTESIAN_POINT('Ctrl Pts',(-2.97860289939383,1.61877566047522,-36.3620740851882));
#29534=CARTESIAN_POINT('Ctrl Pts',(-3.00023974070472,1.57831292113921,-36.3593305186187));
#29535=CARTESIAN_POINT('Ctrl Pts',(-3.03564331088719,1.50874455258696,-36.354710883625));
#29536=CARTESIAN_POINT('Ctrl Pts',(-3.0498285821636,1.4798601829526,-36.3528206853845));
#29537=CARTESIAN_POINT('Ctrl Pts',(-3.07781449699598,1.42076244132663,-36.3490079180979));
#29538=CARTESIAN_POINT('Ctrl Pts',(-3.09158667677173,1.39053943694513,-36.347086467368));
#29539=CARTESIAN_POINT('Ctrl Pts',(-3.12552945611725,1.31305398188221,-36.3422291699285));
#29540=CARTESIAN_POINT('Ctrl Pts',(-3.1450740137539,1.26552557359411,-36.3393141875322));
#29541=CARTESIAN_POINT('Ctrl Pts',(-3.26042524067152,0.965815988506703,
-36.3212943391837));
#29542=CARTESIAN_POINT('Ctrl Pts',(-3.32692152549007,0.703403048467539,
-36.3071956188689));
#29543=CARTESIAN_POINT('Ctrl Pts',(-3.37484868173537,0.333768330703661,
-36.2873331531732));
#29544=CARTESIAN_POINT('Ctrl Pts',(-3.38342800232922,0.231122495838761,
-36.2818043858664));
#29545=CARTESIAN_POINT('Ctrl Pts',(-3.38895531052209,0.085137740948565,
-36.2737404954765));
#29546=CARTESIAN_POINT('Ctrl Pts',(-3.38976435368707,0.0419983438670175,
-36.2713325854174));
#29547=CARTESIAN_POINT('Ctrl Pts',(-3.38973839521835,-0.0349886614083398,
-36.2669728674685));
#29548=CARTESIAN_POINT('Ctrl Pts',(-3.38922007416214,-0.0688309581393426,
-36.2650348265363));
#29549=CARTESIAN_POINT('Ctrl Pts',(-3.38760352429533,-0.12218444861052,
-36.2619376108225));
#29550=CARTESIAN_POINT('Ctrl Pts',(-3.38684314440264,-0.141704452383818,
-36.2607956163946));
#29551=CARTESIAN_POINT('Ctrl Pts',(-3.38504113885493,-0.179550731973185,
-36.2585624594746));
#29552=CARTESIAN_POINT('Ctrl Pts',(-3.38401930001063,-0.197876979546816,
-36.2574723222941));
#29553=CARTESIAN_POINT('Ctrl Pts',(-3.38105278745011,-0.2442949827133,-36.2546903034723));
#29554=CARTESIAN_POINT('Ctrl Pts',(-3.37890681710992,-0.27237216931501,
-36.2529881945179));
#29555=CARTESIAN_POINT('Ctrl Pts',(-3.36799641371311,-0.394994544287951,
-36.245479299598));
#29556=CARTESIAN_POINT('Ctrl Pts',(-3.35561202683189,-0.489168258874862,
-36.2395175926695));
#29557=CARTESIAN_POINT('Ctrl Pts',(-3.29921295692525,-0.812381407571793,
-36.2186386217596));
#29558=CARTESIAN_POINT('Ctrl Pts',(-3.23553595440599,-1.03734737911403,
-36.2034229629017));
#29559=CARTESIAN_POINT('Ctrl Pts',(-3.10719430582373,-1.35966359966522,
-36.1815814961799));
#29560=CARTESIAN_POINT('Ctrl Pts',(-3.05982341694822,-1.46315634725182,
-36.1745508426855));
#29561=CARTESIAN_POINT('Ctrl Pts',(-2.98679581922174,-1.60357009832929,
-36.1650036378923));
#29562=CARTESIAN_POINT('Ctrl Pts',(-2.96548110509562,-1.64265286118646,
-36.1623448312114));
#29563=CARTESIAN_POINT('Ctrl Pts',(-2.92771424475063,-1.70876995032401,
-36.1578423493469));
#29564=CARTESIAN_POINT('Ctrl Pts',(-2.91164247062311,-1.73601372854303,
-36.1559857128867));
#29565=CARTESIAN_POINT('Ctrl Pts',(-2.87775686237685,-1.79165961057409,
-36.1521890920382));
#29566=CARTESIAN_POINT('Ctrl Pts',(-2.85989824314657,-1.82003045964922,
-36.150250977227));
#29567=CARTESIAN_POINT('Ctrl Pts',(-2.81274790603219,-1.89252710178116,
-36.1452889876274));
#29568=CARTESIAN_POINT('Ctrl Pts',(-2.78283716256883,-1.93624052328844,
-36.1422878896269));
#29569=CARTESIAN_POINT('Ctrl Pts',(-2.61171169171275,-2.17417184715629,
-36.125865148514));
#29570=CARTESIAN_POINT('Ctrl Pts',(-2.4511953361399,-2.35365964699743,-36.1132062187244));
#29571=CARTESIAN_POINT('Ctrl Pts',(-2.1516137921046,-2.62445375285005,-36.0917555682986));
#29572=CARTESIAN_POINT('Ctrl Pts',(-2.02240006915864,-2.72526829712647,
-36.0830245805293));
#29573=CARTESIAN_POINT('Ctrl Pts',(-1.85443367684918,-2.83777438219757,
-36.0716417696793));
#29574=CARTESIAN_POINT('Ctrl Pts',(-1.82208061079064,-2.8586552249444,-36.0694474577999));
#29575=CARTESIAN_POINT('Ctrl Pts',(-1.77178215599723,-2.88991736675737,
-36.0660221020505));
#29576=CARTESIAN_POINT('Ctrl Pts',(-1.75408454353289,-2.90069332427577,
-36.0648142893501));
#29577=CARTESIAN_POINT('Ctrl Pts',(-1.72093607994034,-2.92046291783851,
-36.0625450703752));
#29578=CARTESIAN_POINT('Ctrl Pts',(-1.70551117556095,-2.92949760569601,
-36.0614861976795));
#29579=CARTESIAN_POINT('Ctrl Pts',(-1.66809839286833,-2.95101543464584,
-36.0589116005543));
#29580=CARTESIAN_POINT('Ctrl Pts',(-1.64604126486683,-2.96337517275562,
-36.0573886523304));
#29581=CARTESIAN_POINT('Ctrl Pts',(-1.56432258236601,-3.00797250833878,
-36.0517335326194));
#29582=CARTESIAN_POINT('Ctrl Pts',(-1.50383885698185,-3.03866273527339,
-36.0475232784955));
#29583=CARTESIAN_POINT('Ctrl Pts',(-1.33544950623357,-3.1178467429777,-36.0358126086579));
#29584=CARTESIAN_POINT('Ctrl Pts',(-1.22586271860974,-3.16253885004161,
-36.0282057087537));
#29585=CARTESIAN_POINT('Ctrl Pts',(-0.888254867450782,-3.2800347041917,
-36.0051825609125));
#29586=CARTESIAN_POINT('Ctrl Pts',(-0.654618483524561,-3.33453609092645,
-35.9898530327583));
#29587=CARTESIAN_POINT('Ctrl Pts',(-0.362261221123828,-3.37079110216086,
-35.971908066701));
#29588=CARTESIAN_POINT('Ctrl Pts',(-0.307196747023287,-3.37625480977194,
-35.9685774097085));
#29589=CARTESIAN_POINT('Ctrl Pts',(-0.218123255140295,-3.38289561332583,
-35.9632665174595));
#29590=CARTESIAN_POINT('Ctrl Pts',(-0.184188855582638,-3.38491286087705,
-35.9612611032613));
#29591=CARTESIAN_POINT('Ctrl Pts',(-0.11849771889123,-3.38782706213647,
-35.9574119329923));
#29592=CARTESIAN_POINT('Ctrl Pts',(-0.0867475641552904,-3.38878870282408,
-35.9555663972429));
#29593=CARTESIAN_POINT('Ctrl Pts',(-0.0116322428499328,-3.39000736728844,
-35.9512330582839));
#29594=CARTESIAN_POINT('Ctrl Pts',(0.0317340902763956,-3.38987882492134,
-35.9487572233508));
#29595=CARTESIAN_POINT('Ctrl Pts',(0.187992105544546,-3.38641665289971,
-35.9399180038886));
#29596=CARTESIAN_POINT('Ctrl Pts',(0.300707005503613,-3.37827431458885,
-35.9336987043895));
#29597=CARTESIAN_POINT('Ctrl Pts',(0.619594829507402,-3.33914804678742,
-35.9163039542508));
#29598=CARTESIAN_POINT('Ctrl Pts',(0.823591161485063,-3.2947690859119,-35.9054385378855));
#29599=CARTESIAN_POINT('Ctrl Pts',(1.13570417907403,-3.1960519131598,-35.8878626376712));
#29600=CARTESIAN_POINT('Ctrl Pts',(1.24720835052323,-3.15420957655838,-35.8813723102588));
#29601=CARTESIAN_POINT('Ctrl Pts',(1.38404174785385,-3.09447115720145,-35.8728790888058));
#29602=CARTESIAN_POINT('Ctrl Pts',(1.41164814078924,-3.08197545324783,-35.8711375438792));
#29603=CARTESIAN_POINT('Ctrl Pts',(1.45609166648871,-3.06113623517513,-35.8682824142993));
#29604=CARTESIAN_POINT('Ctrl Pts',(1.47303406830883,-3.05301958604326,-35.8671817266046));
#29605=CARTESIAN_POINT('Ctrl Pts',(1.50694078355954,-3.03642785717476,-35.8649524553408));
#29606=CARTESIAN_POINT('Ctrl Pts',(1.52390314248648,-3.02795043409674,-35.8638237741904));
#29607=CARTESIAN_POINT('Ctrl Pts',(1.56852791514194,-3.00517799536937,-35.8608204983834));
#29608=CARTESIAN_POINT('Ctrl Pts',(1.59606542350502,-2.99064367976562,-35.8589324370416));
#29609=CARTESIAN_POINT('Ctrl Pts',(1.75515405330412,-2.90385358523485,-35.8478377590605));
#29610=CARTESIAN_POINT('Ctrl Pts',(1.88198005820198,-2.82330916098814,-35.8382477837061));
#29611=CARTESIAN_POINT('Ctrl Pts',(2.22190461392328,-2.5743244473306,-35.811142967574));
#29612=CARTESIAN_POINT('Ctrl Pts',(2.4207719259826,-2.38828735094287,-35.793666225208));
#29613=CARTESIAN_POINT('Ctrl Pts',(2.62824357639812,-2.14134463149509,-35.7740878728666));
#29614=CARTESIAN_POINT('Ctrl Pts',(2.66025562186351,-2.10144273738525,-35.7710171302957));
#29615=CARTESIAN_POINT('Ctrl Pts',(2.71151645436461,-2.03449833384725,-35.7660131284493));
#29616=CARTESIAN_POINT('Ctrl Pts',(2.73129216285076,-2.00787155713928,-35.7640598230247));
#29617=CARTESIAN_POINT('Ctrl Pts',(2.7694970082527,-1.9548219286716,-35.7602387472698));
#29618=CARTESIAN_POINT('Ctrl Pts',(2.7879465419603,-1.92841816900404,-35.7583703340007));
#29619=CARTESIAN_POINT('Ctrl Pts',(2.83185644359355,-1.86362961156201,-35.753863551595));
#29620=CARTESIAN_POINT('Ctrl Pts',(2.85691658203132,-1.8249805958334,-35.7512399971177));
#29621=CARTESIAN_POINT('Ctrl Pts',(2.95456302344382,-1.66744211377166,-35.7407876002999));
#29622=CARTESIAN_POINT('Ctrl Pts',(3.02058102121791,-1.5446363899599,-35.7331885529657));
#29623=CARTESIAN_POINT('Ctrl Pts',(3.13779660490655,-1.29014891682289,-35.7181530819279));
#29624=CARTESIAN_POINT('Ctrl Pts',(3.18869885792408,-1.15864214182427,-35.7107336777653));
#29625=CARTESIAN_POINT('Ctrl Pts',(3.27357568452938,-0.890901410643851,
-35.6957682698137));
#29626=CARTESIAN_POINT('Ctrl Pts',(3.30756907122169,-0.754972180261875,
-35.6882360499423));
#29627=CARTESIAN_POINT('Ctrl Pts',(3.33987432595466,-0.580555294451817,
-35.6782367155578));
#29628=CARTESIAN_POINT('Ctrl Pts',(3.34607856261757,-0.543657039550838,
-35.6761024735501));
#29629=CARTESIAN_POINT('Ctrl Pts',(3.35473323994378,-0.486404986074056,
-35.6727515128988));
#29630=CARTESIAN_POINT('Ctrl Pts',(3.35761209360037,-0.466117908197508,
-35.6715564866613));
#29631=CARTESIAN_POINT('Ctrl Pts',(3.36266612317762,-0.428022707125048,
-35.6692961122991));
#29632=CARTESIAN_POINT('Ctrl Pts',(3.36488412333369,-0.410221494465349,
-35.6682330218748));
#29633=CARTESIAN_POINT('Ctrl Pts',(3.36993951203867,-0.366844527507218,
-35.6656267425808));
#29634=CARTESIAN_POINT('Ctrl Pts',(3.37262711463376,-0.341252809454412,
-35.6640758649838));
#29635=CARTESIAN_POINT('Ctrl Pts',(3.38166803055292,-0.244579717956199,
-35.6581737932529));
#29636=CARTESIAN_POINT('Ctrl Pts',(3.38606709792027,-0.173338154094305,
-35.6537358352297));
#29637=CARTESIAN_POINT('Ctrl Pts',(3.39209787000417,0.0269591193623061,
-35.6411024242808));
#29638=CARTESIAN_POINT('Ctrl Pts',(3.3886135728306,0.156046133010528,-35.6327827053161));
#29639=CARTESIAN_POINT('Ctrl Pts',(3.35919806089852,0.505146437764565,-35.6102193697391));
#29640=CARTESIAN_POINT('Ctrl Pts',(3.31906075600859,0.723357316537435,-35.5960839801021));
#29641=CARTESIAN_POINT('Ctrl Pts',(3.24228276425979,0.990563709351955,-35.579131222648));
#29642=CARTESIAN_POINT('Ctrl Pts',(3.22527598938504,1.04460966478665,-35.5757181242752));
#29643=CARTESIAN_POINT('Ctrl Pts',(3.19582385311498,1.13061416202461,-35.570309960583));
#29644=CARTESIAN_POINT('Ctrl Pts',(3.18423499574958,1.16285257169047,-35.5682880035938));
#29645=CARTESIAN_POINT('Ctrl Pts',(3.16099830853646,1.2245395834795,-35.5644276608068));
#29646=CARTESIAN_POINT('Ctrl Pts',(3.14942266251315,1.25401135960587,-35.5625871655881));
#29647=CARTESIAN_POINT('Ctrl Pts',(3.12127764948337,1.32281987468349,-35.5582969606599));
#29648=CARTESIAN_POINT('Ctrl Pts',(3.10437471087395,1.36201485701024,-35.5558585177571));
#29649=CARTESIAN_POINT('Ctrl Pts',(3.04234956386105,1.49868254100265,-35.547364184295));
#29650=CARTESIAN_POINT('Ctrl Pts',(2.99333835916829,1.59432386103436,-35.541437015488));
#29651=CARTESIAN_POINT('Ctrl Pts',(2.84655605256545,1.85004207590527,-35.5254372455207));
#29652=CARTESIAN_POINT('Ctrl Pts',(2.73992619745353,2.00458042800868,-35.5156083257711));
#29653=CARTESIAN_POINT('Ctrl Pts',(2.52872369518004,2.26211583136712,-35.4978420196618));
#29654=CARTESIAN_POINT('Ctrl Pts',(2.4292286334931,2.36863913446108,-35.4899830205033));
#29655=CARTESIAN_POINT('Ctrl Pts',(2.30057154086953,2.48972724355342,-35.4799431363505));
#29656=CARTESIAN_POINT('Ctrl Pts',(2.27764635977323,2.510716646156,-35.4781583002393));
#29657=CARTESIAN_POINT('Ctrl Pts',(2.24028431650326,2.54399103644436,-35.4752499083225));
#29658=CARTESIAN_POINT('Ctrl Pts',(2.22602688251641,2.55647579551089,-35.4741401558282));
#29659=CARTESIAN_POINT('Ctrl Pts',(2.19742069022496,2.58110455369589,-35.4719119940472));
#29660=CARTESIAN_POINT('Ctrl Pts',(2.18307413061031,2.59325002772499,-35.470793748612));
#29661=CARTESIAN_POINT('Ctrl Pts',(2.14529786002383,2.62469494669861,-35.467848942649));
#29662=CARTESIAN_POINT('Ctrl Pts',(2.12170906474633,2.64379972334544,-35.4660097871439));
#29663=CARTESIAN_POINT('Ctrl Pts',(1.99654586488111,2.74241663346574,-35.4562634997736));
#29664=CARTESIAN_POINT('Ctrl Pts',(1.89075797493347,2.81639359174969,-35.4480716716442));
#29665=CARTESIAN_POINT('Ctrl Pts',(1.53412583652597,3.03662093769474,-35.4211804309473));
#29666=CARTESIAN_POINT('Ctrl Pts',(1.26862023717671,3.15678103822604,-35.402377130979));
#29667=CARTESIAN_POINT('Ctrl Pts',(0.940328517767844,3.25714570684734,-35.3815053250412));
#29668=CARTESIAN_POINT('Ctrl Pts',(0.88926918375433,3.27145482434731,-35.3783183075523));
#29669=CARTESIAN_POINT('Ctrl Pts',(0.805400792195501,3.29284968847446,-35.3731770256372));
#29670=CARTESIAN_POINT('Ctrl Pts',(0.772786597138734,3.300656071499,-35.3712004682832));
#29671=CARTESIAN_POINT('Ctrl Pts',(0.708851055281177,3.31495973724186,-35.367368413038));
#29672=CARTESIAN_POINT('Ctrl Pts',(0.677543080154877,3.32150016626207,-35.3655117429411));
#29673=CARTESIAN_POINT('Ctrl Pts',(0.602233899826317,3.33612356035288,-35.3610906496112));
#29674=CARTESIAN_POINT('Ctrl Pts',(0.558155540942289,3.34378060511813,-35.3585396273404));
#29675=CARTESIAN_POINT('Ctrl Pts',(0.390112332263439,3.36955645889512,-35.3489390989292));
#29676=CARTESIAN_POINT('Ctrl Pts',(0.265323540830097,3.38167207190852,-35.3420711985415));
#29677=CARTESIAN_POINT('Ctrl Pts',(-0.133825280243136,3.39818802304987,
-35.3205395814368));
#29678=CARTESIAN_POINT('Ctrl Pts',(-0.408123693636666,3.37624031980092,
-35.3064587443863));
#29679=CARTESIAN_POINT('Ctrl Pts',(-0.72917124688984,3.31082706671568,-35.2882542383586));
#29680=CARTESIAN_POINT('Ctrl Pts',(-0.781324390242077,3.29890862792953,
-35.2852380316754));
#29681=CARTESIAN_POINT('Ctrl Pts',(-0.855426656402831,3.28011851518359,
-35.2808400857608));
#29682=CARTESIAN_POINT('Ctrl Pts',(-0.877624030616094,3.27424926300633,
-35.2795081033863));
#29683=CARTESIAN_POINT('Ctrl Pts',(-0.916816127973238,3.26345924341068,
-35.2771277156001));
#29684=CARTESIAN_POINT('Ctrl Pts',(-0.933834647300374,3.25863021426924,
-35.276084315212));
#29685=CARTESIAN_POINT('Ctrl Pts',(-0.971939212435668,3.24749496755305,
-35.273725733932));
#29686=CARTESIAN_POINT('Ctrl Pts',(-0.993002081545012,3.24111650608469,
-35.2724067790341));
#29687=CARTESIAN_POINT('Ctrl Pts',(-1.05834747716395,3.22063124100564,-35.2682705981386));
#29688=CARTESIAN_POINT('Ctrl Pts',(-1.1024013976433,3.20581903481167,-35.2654185209672));
#29689=CARTESIAN_POINT('Ctrl Pts',(-1.20876620773108,3.16760451992292,-35.2583994904839));
#29690=CARTESIAN_POINT('Ctrl Pts',(-1.27071869601075,3.14326379231797,-35.2541985019763));
#29691=CARTESIAN_POINT('Ctrl Pts',(-1.5646566151258,3.01766719613628,-35.2338390689934));
#29692=CARTESIAN_POINT('Ctrl Pts',(-1.78556139979106,2.89244838674332,-35.2173119344543));
#29693=CARTESIAN_POINT('Ctrl Pts',(-2.06815256537044,2.68744509732641,-35.1954943415727));
#29694=CARTESIAN_POINT('Ctrl Pts',(-2.14341477093615,2.62781124612691,-35.1895974241435));
#29695=CARTESIAN_POINT('Ctrl Pts',(-2.244879163353,2.5401523672277,-35.1815282750651));
#29696=CARTESIAN_POINT('Ctrl Pts',(-2.27328707125211,2.51476093791386,-35.1792548913127));
#29697=CARTESIAN_POINT('Ctrl Pts',(-2.32456864559389,2.46734539104511,-35.1751231716981));
#29698=CARTESIAN_POINT('Ctrl Pts',(-2.34757222579197,2.4454687511797,-35.173259075372));
#29699=CARTESIAN_POINT('Ctrl Pts',(-2.39408409152166,2.39997427236873,-35.1694661800941));
#29700=CARTESIAN_POINT('Ctrl Pts',(-2.41755826841108,2.37632642502359,-35.1675389688969));
#29701=CARTESIAN_POINT('Ctrl Pts',(-2.4767171268181,2.31494578202879,-35.1626453363539));
#29702=CARTESIAN_POINT('Ctrl Pts',(-2.51189093953784,2.27673143094917,-35.1597004368941));
#29703=CARTESIAN_POINT('Ctrl Pts',(-2.68311125714268,2.08190979673944,-35.1451537794022));
#29704=CARTESIAN_POINT('Ctrl Pts',(-2.8054612434935,1.91385276459354,-35.1341008080905));
#29705=CARTESIAN_POINT('Ctrl Pts',(-3.01581907170894,1.56096125538752,-35.112297331369));
#29706=CARTESIAN_POINT('Ctrl Pts',(-3.10400753889546,1.37727412792108,-35.1015783717022));
#29707=CARTESIAN_POINT('Ctrl Pts',(-3.18781449811626,1.15305796832824,-35.0880578608937));
#29708=CARTESIAN_POINT('Ctrl Pts',(-3.19989312193933,1.11910131089135,-35.0859984435236));
#29709=CARTESIAN_POINT('Ctrl Pts',(-3.21782618493657,1.06602033691627,-35.0827516677928));
#29710=CARTESIAN_POINT('Ctrl Pts',(-3.22405697578774,1.04702497047019,-35.0815843734478));
#29711=CARTESIAN_POINT('Ctrl Pts',(-3.23561446776625,1.01070887697591,-35.0793404501551));
#29712=CARTESIAN_POINT('Ctrl Pts',(-3.24097087998713,0.993398769585393,
-35.078265455474));
#29713=CARTESIAN_POINT('Ctrl Pts',(-3.25392415086441,0.950318111576882,
-35.07557777389));
#29714=CARTESIAN_POINT('Ctrl Pts',(-3.26135380112186,0.924498879218724,
-35.073956218275));
#29715=CARTESIAN_POINT('Ctrl Pts',(-3.29003392315046,0.820180159838878,
-35.0673688655477));
#29716=CARTESIAN_POINT('Ctrl Pts',(-3.30876191773472,0.741020462581538,
-35.0622897317037));
#29717=CARTESIAN_POINT('Ctrl Pts',(-3.3677558328077,0.444420749121013,-35.0431403213278));
#29718=CARTESIAN_POINT('Ctrl Pts',(-3.3895674096443,0.223877877417544,-35.0287082001579));
#29719=CARTESIAN_POINT('Ctrl Pts',(-3.38974885847844,0.0027818957803985,
-35.0146790786306));
#29720=CARTESIAN_POINT('',(-3.38974998254981,0.000343952908442827,-32.5190351755825));
#29721=CARTESIAN_POINT('Ctrl Pts',(-3.38974886104885,0.00277876196049448,
-35.0146788797815));
#29722=CARTESIAN_POINT('Ctrl Pts',(-3.38982690422481,-0.0924243430868422,
-35.0086379939658));
#29723=CARTESIAN_POINT('Ctrl Pts',(-3.38589419625354,-0.187595440304559,
-35.0026733461612));
#29724=CARTESIAN_POINT('Ctrl Pts',(-3.37293905739721,-0.342514592893689,
-34.9931112098591));
#29725=CARTESIAN_POINT('Ctrl Pts',(-3.36631922380223,-0.402404885928521,
-34.9894503069998));
#29726=CARTESIAN_POINT('Ctrl Pts',(-3.35379977026001,-0.493386448102765,
-34.9839425626804));
#29727=CARTESIAN_POINT('Ctrl Pts',(-3.34905581760021,-0.524622071065607,
-34.982061307855));
#29728=CARTESIAN_POINT('Ctrl Pts',(-3.33864491805334,-0.587258865172567,
-34.9783072956048));
#29729=CARTESIAN_POINT('Ctrl Pts',(-3.33296990619702,-0.618655454138839,
-34.9764349946944));
#29730=CARTESIAN_POINT('Ctrl Pts',(-3.32039385159822,-0.683025811840888,
-34.9726140902599));
#29731=CARTESIAN_POINT('Ctrl Pts',(-3.3134428264174,-0.715986272984172,
-34.9706672713481));
#29732=CARTESIAN_POINT('Ctrl Pts',(-3.2941222857227,-0.801283347624241,
-34.9656510515532));
#29733=CARTESIAN_POINT('Ctrl Pts',(-3.28099640480404,-0.853439904297473,
-34.9626054396638));
#29734=CARTESIAN_POINT('Ctrl Pts',(-3.19872454510333,-1.15031689560506,
-34.9453548010599));
#29735=CARTESIAN_POINT('Ctrl Pts',(-3.10345829663412,-1.3869478189448,-34.9320159235403));
#29736=CARTESIAN_POINT('Ctrl Pts',(-2.91209376832095,-1.74130504901877,
-34.9105885352962));
#29737=CARTESIAN_POINT('Ctrl Pts',(-2.83307429722507,-1.8671142113853,-34.9026298518415));
#29738=CARTESIAN_POINT('Ctrl Pts',(-2.72340772966983,-2.01865060633102,
-34.8920944175098));
#29739=CARTESIAN_POINT('Ctrl Pts',(-2.70020698384903,-2.04958091179739,
-34.8898902172084));
#29740=CARTESIAN_POINT('Ctrl Pts',(-2.66388893673579,-2.09631152873596,
-34.8864653816285));
#29741=CARTESIAN_POINT('Ctrl Pts',(-2.651147961684,-2.11240165016111,-34.8852684963686));
#29742=CARTESIAN_POINT('Ctrl Pts',(-2.62700414677674,-2.14232951565063,
-34.8830068796901));
#29743=CARTESIAN_POINT('Ctrl Pts',(-2.61563641773531,-2.15619401155531,
-34.8819444464711));
#29744=CARTESIAN_POINT('Ctrl Pts',(-2.58773013465438,-2.18968410729951,
-34.8793429744375));
#29745=CARTESIAN_POINT('Ctrl Pts',(-2.57107787604637,-2.2092130290383,-34.8777963171741));
#29746=CARTESIAN_POINT('Ctrl Pts',(-2.51093542071305,-2.27814403811377,
-34.8722361233496));
#29747=CARTESIAN_POINT('Ctrl Pts',(-2.46623226764138,-2.32646388856345,
-34.8681505158557));
#29748=CARTESIAN_POINT('Ctrl Pts',(-2.24375158879616,-2.55332261558018,
-34.8481621869646));
#29749=CARTESIAN_POINT('Ctrl Pts',(-2.04784572541907,-2.71297165087198,
-34.8316493323975));
#29750=CARTESIAN_POINT('Ctrl Pts',(-1.72815727676698,-2.91896408340487,
-34.8075972434133));
#29751=CARTESIAN_POINT('Ctrl Pts',(-1.61639515349901,-2.98230643125532,
-34.7996342873614));
#29752=CARTESIAN_POINT('Ctrl Pts',(-1.46091289751696,-3.05911221545851,
-34.78916749588));
#29753=CARTESIAN_POINT('Ctrl Pts',(-1.4201324522529,-3.07825569928002,-34.7864756530796));
#29754=CARTESIAN_POINT('Ctrl Pts',(-1.34971782903468,-3.10961299889367,
-34.7819161898915));
#29755=CARTESIAN_POINT('Ctrl Pts',(-1.32027064987619,-3.12222944965444,
-34.7800353246241));
#29756=CARTESIAN_POINT('Ctrl Pts',(-1.2634153235531,-3.14564050097317,-34.7764517186054));
#29757=CARTESIAN_POINT('Ctrl Pts',(-1.23603678667977,-3.15649894378423,
-34.7747470011713));
#29758=CARTESIAN_POINT('Ctrl Pts',(-1.16290015217932,-3.18440771224144,
-34.7702464072632));
#29759=CARTESIAN_POINT('Ctrl Pts',(-1.1169084277803,-3.20082882119852,-34.767471080449));
#29760=CARTESIAN_POINT('Ctrl Pts',(-0.900493809802508,-3.27286559500886,
-34.7546428422546));
#29761=CARTESIAN_POINT('Ctrl Pts',(-0.72618148303251,-3.31590226899461,
-34.7449914641347));
#29762=CARTESIAN_POINT('Ctrl Pts',(-0.379578793328886,-3.37281719444198,
-34.726300713963));
#29763=CARTESIAN_POINT('Ctrl Pts',(-0.208023834352916,-3.38772733832745,
-34.7172749306414));
#29764=CARTESIAN_POINT('Ctrl Pts',(0.047085910097641,-3.39044342520962,
-34.7033694546863));
#29765=CARTESIAN_POINT('Ctrl Pts',(0.130257999734886,-3.38826718370647,
-34.6987573660932));
#29766=CARTESIAN_POINT('Ctrl Pts',(0.240265078516032,-3.38133257232834,
-34.6924579124442));
#29767=CARTESIAN_POINT('Ctrl Pts',(0.267248596295292,-3.37930693511218,
-34.6908967460967));
#29768=CARTESIAN_POINT('Ctrl Pts',(0.312288774480554,-3.375382989154,-34.6882599348768));
#29769=CARTESIAN_POINT('Ctrl Pts',(0.330360255566219,-3.37366220801277,
-34.6871935860849));
#29770=CARTESIAN_POINT('Ctrl Pts',(0.368228177019154,-3.36974921072111,
-34.6849401296154));
#29771=CARTESIAN_POINT('Ctrl Pts',(0.388020327948082,-3.36752756711329,
-34.683751625354));
#29772=CARTESIAN_POINT('Ctrl Pts',(0.443209978488878,-3.3608396107482,-34.6804097647904));
#29773=CARTESIAN_POINT('Ctrl Pts',(0.47855730307099,-3.35598877603464,-34.6782374617739));
#29774=CARTESIAN_POINT('Ctrl Pts',(0.758580321919093,-3.31304655222868,
-34.6608083933622));
#29775=CARTESIAN_POINT('Ctrl Pts',(0.998479534114965,-3.24880794519959,
-34.6446007813284));
#29776=CARTESIAN_POINT('Ctrl Pts',(1.33625315593318,-3.11737391340009,-34.6214151778978));
#29777=CARTESIAN_POINT('Ctrl Pts',(1.44109473445916,-3.0703162874983,-34.614151712773));
#29778=CARTESIAN_POINT('Ctrl Pts',(1.61507637750078,-2.9813458370174,-34.6020485668035));
#29779=CARTESIAN_POINT('Ctrl Pts',(1.68547421987451,-2.9421204875355,-34.5971356323225));
#29780=CARTESIAN_POINT('Ctrl Pts',(1.78754027826934,-2.88038258668276,-34.5899885204448));
#29781=CARTESIAN_POINT('Ctrl Pts',(1.82032374714407,-2.85977721737487,-34.5876888672072));
#29782=CARTESIAN_POINT('Ctrl Pts',(1.87891134715219,-2.82153740751192,-34.5835700369392));
#29783=CARTESIAN_POINT('Ctrl Pts',(1.90483791915879,-2.80409946156646,-34.5817440172448));
#29784=CARTESIAN_POINT('Ctrl Pts',(1.96052894272978,-2.7655133591886,-34.5778126423914));
#29785=CARTESIAN_POINT('Ctrl Pts',(1.99020046699295,-2.74423762164994,-34.5757123216832));
#29786=CARTESIAN_POINT('Ctrl Pts',(2.07269969422843,-2.68304020503453,-34.5698513756995));
#29787=CARTESIAN_POINT('Ctrl Pts',(2.12471106887763,-2.64204322917209,-34.566131601432));
#29788=CARTESIAN_POINT('Ctrl Pts',(2.36883912125081,-2.43773906428165,-34.5484816449661));
#29789=CARTESIAN_POINT('Ctrl Pts',(2.54352796260521,-2.25487041198006,-34.5353339358947));
#29790=CARTESIAN_POINT('Ctrl Pts',(2.78161233832029,-1.94238020353759,-34.5143564651655));
#29791=CARTESIAN_POINT('Ctrl Pts',(2.85983464248742,-1.82525233641982,-34.5067468903608));
#29792=CARTESIAN_POINT('Ctrl Pts',(2.94604314139119,-1.67695729859936,-34.496996244675));
#29793=CARTESIAN_POINT('Ctrl Pts',(2.96117599889122,-1.65008864443326,-34.4952250266343));
#29794=CARTESIAN_POINT('Ctrl Pts',(2.98498861800167,-1.60642621811201,-34.4923334026055));
#29795=CARTESIAN_POINT('Ctrl Pts',(2.9938984525569,-1.58975918375157,-34.4912265136524));
#29796=CARTESIAN_POINT('Ctrl Pts',(3.01141434457904,-1.55632385093623,-34.4889981508541));
#29797=CARTESIAN_POINT('Ctrl Pts',(3.02002084306773,-1.53955654410371,-34.4878767579429));
#29798=CARTESIAN_POINT('Ctrl Pts',(3.04222895874108,-1.49538753152628,-34.4849142697675));
#29799=CARTESIAN_POINT('Ctrl Pts',(3.05559995408492,-1.46787250316995,-34.4830603185984));
#29800=CARTESIAN_POINT('Ctrl Pts',(3.12203706839389,-1.32631486062107,-34.4734931609101));
#29801=CARTESIAN_POINT('Ctrl Pts',(3.16909422511869,-1.2095713718572,-34.4655108527891));
#29802=CARTESIAN_POINT('Ctrl Pts',(3.27478666286398,-0.898496657571354,
-34.4444418374273));
#29803=CARTESIAN_POINT('Ctrl Pts',(3.32266627058404,-0.701015921487936,
-34.4312867947251));
#29804=CARTESIAN_POINT('Ctrl Pts',(3.36907463558273,-0.390108002041411,
-34.4115286979423));
#29805=CARTESIAN_POINT('Ctrl Pts',(3.38008809278936,-0.279028156420628,
-34.4046454587518));
#29806=CARTESIAN_POINT('Ctrl Pts',(3.387739896363,-0.124455798019335,-34.395322880176));
#29807=CARTESIAN_POINT('Ctrl Pts',(3.38905080939095,-0.0812755772965244,
-34.3927456916865));
#29808=CARTESIAN_POINT('Ctrl Pts',(3.38989263039676,-0.00634539808840575,
-34.3883185136122));
#29809=CARTESIAN_POINT('Ctrl Pts',(3.38980346890386,0.0253939600347397,
-34.3864571985843));
#29810=CARTESIAN_POINT('Ctrl Pts',(3.38869465853402,0.0911768085449157,
-34.3826267956063));
#29811=CARTESIAN_POINT('Ctrl Pts',(3.38760768910887,0.12521567487828,-34.3806599755761));
#29812=CARTESIAN_POINT('Ctrl Pts',(3.38339448490624,0.214807128708987,-34.3755198093596));
#29813=CARTESIAN_POINT('Ctrl Pts',(3.37941314899832,0.270310188160491,-34.3723726237765));
#29814=CARTESIAN_POINT('Ctrl Pts',(3.35138791555575,0.560642492992985,-34.356064483073));
#29815=CARTESIAN_POINT('Ctrl Pts',(3.30423138807837,0.792581950040394,-34.3436247233995));
#29816=CARTESIAN_POINT('Ctrl Pts',(3.18203957869957,1.18077919016614,-34.3220050374073));
#29817=CARTESIAN_POINT('Ctrl Pts',(3.11847370633536,1.33967349091239,-34.3128847286386));
#29818=CARTESIAN_POINT('Ctrl Pts',(3.028184406851,1.52370197866563,-34.3012802745253));
#29819=CARTESIAN_POINT('Ctrl Pts',(3.01269946871612,1.55409467099378,-34.2993276287108));
#29820=CARTESIAN_POINT('Ctrl Pts',(2.98760338732323,1.60156637139249,-34.2962124072376));
#29821=CARTESIAN_POINT('Ctrl Pts',(2.97829786937535,1.61880530089336,-34.2950673489921));
#29822=CARTESIAN_POINT('Ctrl Pts',(2.96010590324536,1.65181896467861,-34.2928459738907));
#29823=CARTESIAN_POINT('Ctrl Pts',(2.95124160465024,1.66760480554725,-34.2917709541762));
#29824=CARTESIAN_POINT('Ctrl Pts',(2.92845116777581,1.70743993326548,-34.2890268015878));
#29825=CARTESIAN_POINT('Ctrl Pts',(2.91435508712683,1.73139010196063,-34.2873476786546));
#29826=CARTESIAN_POINT('Ctrl Pts',(2.85671301609949,1.82662914591736,-34.2805608077938));
#29827=CARTESIAN_POINT('Ctrl Pts',(2.81083545310889,1.89646652462634,-34.2753352262041));
#29828=CARTESIAN_POINT('Ctrl Pts',(2.6380484380674,2.13943112941956,-34.25643062724));
#29829=CARTESIAN_POINT('Ctrl Pts',(2.49733850557292,2.3021230731035,-34.2424324035838));
#29830=CARTESIAN_POINT('Ctrl Pts',(2.2405586149924,2.54756079739279,-34.2198805859861));
#29831=CARTESIAN_POINT('Ctrl Pts',(2.13297840919079,2.63829108123176,-34.2111266444174));
#29832=CARTESIAN_POINT('Ctrl Pts',(1.9829884592345,2.74959874265178,-34.1998407347253));
#29833=CARTESIAN_POINT('Ctrl Pts',(1.94535511608205,2.77635196988582,-34.1970792399544));
#29834=CARTESIAN_POINT('Ctrl Pts',(1.88054234961348,2.82046169728733,-34.1924386905388));
#29835=CARTESIAN_POINT('Ctrl Pts',(1.85364125362016,2.8382138615208,-34.1905451964203));
#29836=CARTESIAN_POINT('Ctrl Pts',(1.79857558217943,2.87343504720916,-34.1867331930546));
#29837=CARTESIAN_POINT('Ctrl Pts',(1.77039980389121,2.89088009818977,-34.1848156913425));
#29838=CARTESIAN_POINT('Ctrl Pts',(1.69821794267487,2.93412036244863,-34.1799834300892));
#29839=CARTESIAN_POINT('Ctrl Pts',(1.65387640054368,2.95934109472077,-34.1770890852916));
#29840=CARTESIAN_POINT('Ctrl Pts',(1.36931157522843,3.11280223228045,-34.1589416404228));
#29841=CARTESIAN_POINT('Ctrl Pts',(1.1149486422462,3.21270146399418,-34.1447188437405));
#29842=CARTESIAN_POINT('Ctrl Pts',(0.706691321019504,3.31863389521196,-34.1222359671799));
#29843=CARTESIAN_POINT('Ctrl Pts',(0.559711031811383,3.34655914131875,-34.1141814014913));
#29844=CARTESIAN_POINT('Ctrl Pts',(0.380495662063168,3.36847094907184,-34.103921970846));
#29845=CARTESIAN_POINT('Ctrl Pts',(0.349556827479023,3.37182196490236,-34.1021350630129));
#29846=CARTESIAN_POINT('Ctrl Pts',(0.29970217596337,3.37652826406392,-34.099224119708));
#29847=CARTESIAN_POINT('Ctrl Pts',(0.280812807596176,3.37815166056643,-34.0981139312925));
#29848=CARTESIAN_POINT('Ctrl Pts',(0.245425847365641,3.38089405612176,-34.0960189027458));
#29849=CARTESIAN_POINT('Ctrl Pts',(0.228931684723151,3.38205096360446,-34.0950361934042));
#29850=CARTESIAN_POINT('Ctrl Pts',(0.184365920817121,3.38484932843634,-34.0923654626453));
#29851=CARTESIAN_POINT('Ctrl Pts',(0.156281830147808,3.38626219395434,-34.0906658153288));
#29852=CARTESIAN_POINT('Ctrl Pts',(0.0410736120218453,3.39062194637338,
-34.0836340332441));
#29853=CARTESIAN_POINT('Ctrl Pts',(-0.0461256647190106,3.39055664230569,
-34.0781733023392));
#29854=CARTESIAN_POINT('Ctrl Pts',(-0.344170923460956,3.37883430929543,
-34.0592348346581));
#29855=CARTESIAN_POINT('Ctrl Pts',(-0.5538886370471,3.35084877875865,-34.0454722381292));
#29856=CARTESIAN_POINT('Ctrl Pts',(-0.895972408694878,3.27218670582534,
-34.0231917227614));
#29857=CARTESIAN_POINT('Ctrl Pts',(-1.03023846418474,3.23242769352349,-34.0144831957068));
#29858=CARTESIAN_POINT('Ctrl Pts',(-1.2049923575738,3.16867865182188,-34.0032439002521));
#29859=CARTESIAN_POINT('Ctrl Pts',(-1.247982515665,3.15199475459977,-34.0004860993103));
#29860=CARTESIAN_POINT('Ctrl Pts',(-1.32041155998456,3.12217173589579,-33.9958498607988));
#29861=CARTESIAN_POINT('Ctrl Pts',(-1.35002690204469,3.10948074541583,-33.9939570476905));
#29862=CARTESIAN_POINT('Ctrl Pts',(-1.40617296441659,3.08446721872072,-33.9903726190409));
#29863=CARTESIAN_POINT('Ctrl Pts',(-1.4327337628727,3.07221979542705,-33.9886787036729));
#29864=CARTESIAN_POINT('Ctrl Pts',(-1.50211284904934,3.03913300309358,-33.9842566093757));
#29865=CARTESIAN_POINT('Ctrl Pts',(-1.54465707347693,3.01773213870837,-33.9815475853754));
#29866=CARTESIAN_POINT('Ctrl Pts',(-1.71123422964111,2.92949329442905,-33.9709334303889));
#29867=CARTESIAN_POINT('Ctrl Pts',(-1.83150452424359,2.85584491763664,-33.9632608626042));
#29868=CARTESIAN_POINT('Ctrl Pts',(-2.11437066166908,2.65738925318995,-33.9447401392526));
#29869=CARTESIAN_POINT('Ctrl Pts',(-2.27089458589667,2.52493804283488,-33.9340762232955));
#29870=CARTESIAN_POINT('Ctrl Pts',(-2.47774434496852,2.31501709533584,-33.918068483271));
#29871=CARTESIAN_POINT('Ctrl Pts',(-2.53838805005272,2.24835601688879,-33.913089983142));
#29872=CARTESIAN_POINT('Ctrl Pts',(-2.61412830695887,2.15812585139271,-33.9063641739515));
#29873=CARTESIAN_POINT('Ctrl Pts',(-2.63169457216682,2.13666973791777,-33.9047656902064));
#29874=CARTESIAN_POINT('Ctrl Pts',(-2.66039688509124,2.10072068920883,-33.9020843802752));
#29875=CARTESIAN_POINT('Ctrl Pts',(-2.67168291330316,2.08634834074651,-33.9010115727456));
#29876=CARTESIAN_POINT('Ctrl Pts',(-2.69487819497183,2.05631313302973,-33.8987664425462));
#29877=CARTESIAN_POINT('Ctrl Pts',(-2.70676812006585,2.0406367851908,-33.8975930315553));
#29878=CARTESIAN_POINT('Ctrl Pts',(-2.73913920649202,1.99717622962009,-33.8943375632345));
#29879=CARTESIAN_POINT('Ctrl Pts',(-2.75933297341615,1.96918202013568,-33.8922380276508));
#29880=CARTESIAN_POINT('Ctrl Pts',(-2.90427141219207,1.76164908418293,-33.8766830481539));
#29881=CARTESIAN_POINT('Ctrl Pts',(-3.01180706092764,1.5707347405806,-33.862462698946));
#29882=CARTESIAN_POINT('Ctrl Pts',(-3.17838338482558,1.19400785940032,-33.8359956404397));
#29883=CARTESIAN_POINT('Ctrl Pts',(-3.24130113660487,1.01082189572249,-33.8237566009576));
#29884=CARTESIAN_POINT('Ctrl Pts',(-3.30105900602259,0.772134059237047,
-33.8088007363692));
#29885=CARTESIAN_POINT('Ctrl Pts',(-3.3126630524489,0.720725697539464,-33.8056339120265));
#29886=CARTESIAN_POINT('Ctrl Pts',(-3.32967030175316,0.636255361438118,
-33.8005164773026));
#29887=CARTESIAN_POINT('Ctrl Pts',(-3.33579016482181,0.603348405979583,
-33.7985439698615));
#29888=CARTESIAN_POINT('Ctrl Pts',(-3.34674838592617,0.539149758655512,
-33.7947351132573));
#29889=CARTESIAN_POINT('Ctrl Pts',(-3.35163765731479,0.507870390737447,
-33.7928973667653));
#29890=CARTESIAN_POINT('Ctrl Pts',(-3.36236980150594,0.432285853419744,
-33.7884976425721));
#29891=CARTESIAN_POINT('Ctrl Pts',(-3.36777624898775,0.387924142197492,
-33.7859492800458));
#29892=CARTESIAN_POINT('Ctrl Pts',(-3.38400763646391,0.228557513167015,
-33.776902692303));
#29893=CARTESIAN_POINT('Ctrl Pts',(-3.38983092727204,0.113119094727432,
-33.7705541994048));
#29894=CARTESIAN_POINT('Ctrl Pts',(-3.38958757092891,-0.230649292059321,
-33.7519739261274));
#29895=CARTESIAN_POINT('Ctrl Pts',(-3.36637334460148,-0.458287124936508,
-33.7401275512925));
#29896=CARTESIAN_POINT('Ctrl Pts',(-3.30112254656824,-0.776040945303472,
-33.7225654538627));
#29897=CARTESIAN_POINT('Ctrl Pts',(-3.27778502338376,-0.869351485472063,
-33.7172710373615));
#29898=CARTESIAN_POINT('Ctrl Pts',(-3.24231509939374,-0.989259157956663,
-33.7101442169138));
#29899=CARTESIAN_POINT('Ctrl Pts',(-3.23376027829352,-1.01687522807927,
-33.7084800290812));
#29900=CARTESIAN_POINT('Ctrl Pts',(-3.21971606485589,-1.06024128279909,
-33.7058257648327));
#29901=CARTESIAN_POINT('Ctrl Pts',(-3.21446167112142,-1.0760665663484,-33.7048484835209));
#29902=CARTESIAN_POINT('Ctrl Pts',(-3.20304920165912,-1.10960925254065,
-33.702757327867));
#29903=CARTESIAN_POINT('Ctrl Pts',(-3.19686044851894,-1.12731544459897,
-33.7016416492259));
#29904=CARTESIAN_POINT('Ctrl Pts',(-3.18033780316556,-1.17335680068938,
-33.6987113216133));
#29905=CARTESIAN_POINT('Ctrl Pts',(-3.1697722962889,-1.20160649849822,-33.6968842906415));
#29906=CARTESIAN_POINT('Ctrl Pts',(-3.11349267381627,-1.34617538055025,
-33.6873976541616));
#29907=CARTESIAN_POINT('Ctrl Pts',(-3.06175103806851,-1.46003422783873,
-33.6794705559301));
#29908=CARTESIAN_POINT('Ctrl Pts',(-2.87251916865601,-1.82191101057061,
-33.6532892840511));
#29909=CARTESIAN_POINT('Ctrl Pts',(-2.71018547359303,-2.05564329151342,
-33.6348981444548));
#29910=CARTESIAN_POINT('Ctrl Pts',(-2.48126986182878,-2.31023186044375,
-33.6139858574241));
#29911=CARTESIAN_POINT('Ctrl Pts',(-2.44076904396329,-2.35298076765167,
-33.6104337927574));
#29912=CARTESIAN_POINT('Ctrl Pts',(-2.37466077365739,-2.41921376989797,
-33.6048618921935));
#29913=CARTESIAN_POINT('Ctrl Pts',(-2.34977201870952,-2.44339531139193,
-33.6028121834748));
#29914=CARTESIAN_POINT('Ctrl Pts',(-2.30157152496064,-2.48880841323714,
-33.5989313170498));
#29915=CARTESIAN_POINT('Ctrl Pts',(-2.27832642819208,-2.51010509478455,
-33.5970975199136));
#29916=CARTESIAN_POINT('Ctrl Pts',(-2.22367282168149,-2.55879280491719,
-33.5928703978457));
#29917=CARTESIAN_POINT('Ctrl Pts',(-2.19204924390185,-2.58593537502077,
-33.5904873124589));
#29918=CARTESIAN_POINT('Ctrl Pts',(-2.08301725361847,-2.67607995535169,
-33.5824711351141));
#29919=CARTESIAN_POINT('Ctrl Pts',(-2.00332771654797,-2.73624656227071,
-33.5769470788099));
#29920=CARTESIAN_POINT('Ctrl Pts',(-1.78674439549559,-2.88522787384046,
-33.562634828032));
#29921=CARTESIAN_POINT('Ctrl Pts',(-1.6458973334152,-2.96783087167764,-33.554023574467));
#29922=CARTESIAN_POINT('Ctrl Pts',(-1.34952063081701,-3.11403645803161,
-33.5364725832783));
#29923=CARTESIAN_POINT('Ctrl Pts',(-1.19412464909152,-3.17686709673405,
-33.5275510093057));
#29924=CARTESIAN_POINT('Ctrl Pts',(-0.998751741711168,-3.23949508585984,
-33.515990352926));
#29925=CARTESIAN_POINT('Ctrl Pts',(-0.962572696906014,-3.25042874250805,
-33.513835225288));
#29926=CARTESIAN_POINT('Ctrl Pts',(-0.906432122661093,-3.2663755177457,
-33.5104583875593));
#29927=CARTESIAN_POINT('Ctrl Pts',(-0.886594028074614,-3.27181588702464,
-33.5092588996264));
#29928=CARTESIAN_POINT('Ctrl Pts',(-0.849387287517357,-3.28165618210674,
-33.5069955184983));
#29929=CARTESIAN_POINT('Ctrl Pts',(-0.832031386866415,-3.28609947777207,
-33.5059339799804));
#29930=CARTESIAN_POINT('Ctrl Pts',(-0.789819624934591,-3.29655030526925,
-33.5033391217881));
#29931=CARTESIAN_POINT('Ctrl Pts',(-0.76492979701057,-3.3024144613338,-33.5017982804914));
#29932=CARTESIAN_POINT('Ctrl Pts',(-0.67160076930187,-3.32329154645115,
-33.4959863355616));
#29933=CARTESIAN_POINT('Ctrl Pts',(-0.602771362054284,-3.33646214517497,
-33.4916316908523));
#29934=CARTESIAN_POINT('Ctrl Pts',(-0.410140706734968,-3.36716738381519,
-33.4793417682405));
#29935=CARTESIAN_POINT('Ctrl Pts',(-0.285703800938918,-3.38000037518403,
-33.4712889483607));
#29936=CARTESIAN_POINT('Ctrl Pts',(0.0665665797099702,-3.396734914986,-33.4485737223653));
#29937=CARTESIAN_POINT('Ctrl Pts',(0.294522395735952,-3.38460092837313,
-33.4340140258785));
#29938=CARTESIAN_POINT('Ctrl Pts',(0.575199971240628,-3.34106569254644,
-33.4166991185306));
#29939=CARTESIAN_POINT('Ctrl Pts',(0.630615251683416,-3.33105087573173,
-33.4133075510693));
#29940=CARTESIAN_POINT('Ctrl Pts',(0.719237411589568,-3.31274377463789,
-33.4079247835941));
#29941=CARTESIAN_POINT('Ctrl Pts',(0.752611236702497,-3.30532150090951,
-33.4059071432027));
#29942=CARTESIAN_POINT('Ctrl Pts',(0.816690848854646,-3.29004941168908,
-33.4020497998382));
#29943=CARTESIAN_POINT('Ctrl Pts',(0.847409901580814,-3.28227141351291,
-33.4002080723699));
#29944=CARTESIAN_POINT('Ctrl Pts',(0.91940460470855,-3.26296436272826,-33.3959070518673));
#29945=CARTESIAN_POINT('Ctrl Pts',(0.960580090632091,-3.25108095591568,
-33.3934592015028));
#29946=CARTESIAN_POINT('Ctrl Pts',(1.10542587100572,-3.20628564171881,-33.3848799033921));
#29947=CARTESIAN_POINT('Ctrl Pts',(1.20772978215323,-3.16916798519504,-33.3788808702972));
#29948=CARTESIAN_POINT('Ctrl Pts',(1.47335019931879,-3.05806115134583,-33.3632659170203));
#29949=CARTESIAN_POINT('Ctrl Pts',(1.63288022594376,-2.97593723923242,-33.3538572650203));
#29950=CARTESIAN_POINT('Ctrl Pts',(1.90415739098513,-2.8078781740471,-33.3368540579961));
#29951=CARTESIAN_POINT('Ctrl Pts',(2.01845030156449,-2.72687488923117,-33.3293232744458));
#29952=CARTESIAN_POINT('Ctrl Pts',(2.15652736667546,-2.61556774086048,-33.3193255694748));
#29953=CARTESIAN_POINT('Ctrl Pts',(2.18526380609547,-2.59160698193444,-33.3171913811095));
#29954=CARTESIAN_POINT('Ctrl Pts',(2.22911452090418,-2.55379587401048,-33.3138404866312));
#29955=CARTESIAN_POINT('Ctrl Pts',(2.24451044594963,-2.54027512785831,-33.3126454715545));
#29956=CARTESIAN_POINT('Ctrl Pts',(2.27315414420973,-2.51465646419266,-33.3103851040725));
#29957=CARTESIAN_POINT('Ctrl Pts',(2.28642991286373,-2.50259167544523,-33.3093220091149));
#29958=CARTESIAN_POINT('Ctrl Pts',(2.31851470370448,-2.47296518647542,-33.306715698344));
#29959=CARTESIAN_POINT('Ctrl Pts',(2.33722044479533,-2.45529382139935,-33.3051647933528));
#29960=CARTESIAN_POINT('Ctrl Pts',(2.4070397709563,-2.38781447267138,-33.2992624748821));
#29961=CARTESIAN_POINT('Ctrl Pts',(2.45677446713755,-2.33661212705251,-33.2948242886297));
#29962=CARTESIAN_POINT('Ctrl Pts',(2.59179809789646,-2.18852467634677,-33.2821899273249));
#29963=CARTESIAN_POINT('Ctrl Pts',(2.67322413028724,-2.08828349997284,-33.2738694674998));
#29964=CARTESIAN_POINT('Ctrl Pts',(2.8782347061422,-1.80420118401244,-33.2513065257479));
#29965=CARTESIAN_POINT('Ctrl Pts',(2.98986834418226,-1.61247939164622,-33.237172282167));
#29966=CARTESIAN_POINT('Ctrl Pts',(3.10560602388813,-1.35971515142524,-33.2202205180091));
#29967=CARTESIAN_POINT('Ctrl Pts',(3.12789592060347,-1.30762446913768,-33.2168073740174));
#29968=CARTESIAN_POINT('Ctrl Pts',(3.16155325642045,-1.22317598918447,-33.2113991563452));
#29969=CARTESIAN_POINT('Ctrl Pts',(3.17375297204456,-1.19116358837664,-33.2093771900424));
#29970=CARTESIAN_POINT('Ctrl Pts',(3.1962907946282,-1.12921771651209,-33.2055168403932));
#29971=CARTESIAN_POINT('Ctrl Pts',(3.2066987779171,-1.09931366857137,-33.2036763474485));
#29972=CARTESIAN_POINT('Ctrl Pts',(3.23014923994992,-1.02876743916606,-33.1993861642674));
#29973=CARTESIAN_POINT('Ctrl Pts',(3.24284627148427,-0.988015610180735,
-33.1969477404765));
#29974=CARTESIAN_POINT('Ctrl Pts',(3.28477606706078,-0.843911027164396,
-33.1884535800894));
#29975=CARTESIAN_POINT('Ctrl Pts',(3.30986512477057,-0.739415557750358,
-33.1825265577575));
#29976=CARTESIAN_POINT('Ctrl Pts',(3.36500111904763,-0.449778692293402,
-33.1665274462738));
#29977=CARTESIAN_POINT('Ctrl Pts',(3.38471977495014,-0.263071598775227,
-33.1566990097192));
#29978=CARTESIAN_POINT('Ctrl Pts',(3.39215679905814,0.0699119802708021,
-33.1389325557749));
#29979=CARTESIAN_POINT('Ctrl Pts',(3.38602152600385,0.215557880546048,-33.131072877132));
#29980=CARTESIAN_POINT('Ctrl Pts',(3.36723869527788,0.391247663705663,-33.121032235086));
#29981=CARTESIAN_POINT('Ctrl Pts',(3.3635097464359,0.422105681653361,-33.1192473959467));
#29982=CARTESIAN_POINT('Ctrl Pts',(3.35682505184185,0.471688227620651,-33.1163390002505));
#29983=CARTESIAN_POINT('Ctrl Pts',(3.35413556856925,0.490447512835545,-33.1152292470669));
#29984=CARTESIAN_POINT('Ctrl Pts',(3.34846539057391,0.527766932086595,-33.1130010853458));
#29985=CARTESIAN_POINT('Ctrl Pts',(3.34548732531331,0.546326753637205,-33.1118828406793));
#29986=CARTESIAN_POINT('Ctrl Pts',(3.33729690947443,0.594790556610575,-33.1089380387386));
#29987=CARTESIAN_POINT('Ctrl Pts',(3.33183706087192,0.624650405556525,-33.1070988865434));
#29988=CARTESIAN_POINT('Ctrl Pts',(3.30107365063774,0.78099734309863,-33.0973526706085));
#29989=CARTESIAN_POINT('Ctrl Pts',(3.26896802608414,0.906027782546418,-33.0891609153821));
#29990=CARTESIAN_POINT('Ctrl Pts',(3.1417404640823,1.30540294946159,-33.0622696173468));
#29991=CARTESIAN_POINT('Ctrl Pts',(3.0185010387914,1.56949562350026,-33.043466177757));
#29992=CARTESIAN_POINT('Ctrl Pts',(2.83472248995926,1.85945267099938,-33.0225942797385));
#29993=CARTESIAN_POINT('Ctrl Pts',(2.80529273004858,1.90356218744007,-33.0194072893487));
#29994=CARTESIAN_POINT('Ctrl Pts',(2.75557897934114,1.97441484738668,-33.0142660396197));
#29995=CARTESIAN_POINT('Ctrl Pts',(2.73591214558279,2.00157796568216,-33.0122894878802));
#29996=CARTESIAN_POINT('Ctrl Pts',(2.69670702001363,2.05406892021864,-33.0084574360071));
#29997=CARTESIAN_POINT('Ctrl Pts',(2.6772069704642,2.07942078953108,-33.0066007637849));
#29998=CARTESIAN_POINT('Ctrl Pts',(2.62957850237576,2.1395614046487,-33.0021796531248));
#29999=CARTESIAN_POINT('Ctrl Pts',(2.60111415750851,2.1740771621632,-32.9996286159414));
#30000=CARTESIAN_POINT('Ctrl Pts',(2.49037179336167,2.30307345995335,-32.9900279240602));
#30001=CARTESIAN_POINT('Ctrl Pts',(2.40355888159715,2.39353461554367,-32.9831598837663));
#30002=CARTESIAN_POINT('Ctrl Pts',(2.11138770723128,2.66601645534111,-32.9616270865751));
#30003=CARTESIAN_POINT('Ctrl Pts',(1.8889150198122,2.82799830735902,-32.9475453066251));
#30004=CARTESIAN_POINT('Ctrl Pts',(1.60267083293559,2.98742549060242,-32.9293403696739));
#30005=CARTESIAN_POINT('Ctrl Pts',(1.55534470717127,3.01233581598341,-32.9263250338815));
#30006=CARTESIAN_POINT('Ctrl Pts',(1.48688924114406,3.04632442547569,-32.9219281338846));
#30007=CARTESIAN_POINT('Ctrl Pts',(1.46622397861806,3.05632447598448,-32.9205962941572));
#30008=CARTESIAN_POINT('Ctrl Pts',(1.42945722054536,3.07365744608497,-32.9182160557564));
#30009=CARTESIAN_POINT('Ctrl Pts',(1.41339738655488,3.08107543640678,-32.9171726594546));
#30010=CARTESIAN_POINT('Ctrl Pts',(1.37722681499142,3.09744020020741,-32.9148139476308));
#30011=CARTESIAN_POINT('Ctrl Pts',(1.35708660065256,3.1063170145883,-32.9134948557009));
#30012=CARTESIAN_POINT('Ctrl Pts',(1.29414286192117,3.13333055459123,-32.90935778409));
#30013=CARTESIAN_POINT('Ctrl Pts',(1.25105327837817,3.15078265804886,-32.9065049328919));
#30014=CARTESIAN_POINT('Ctrl Pts',(1.14541285191986,3.19106045729588,-32.8994835351815));
#30015=CARTESIAN_POINT('Ctrl Pts',(1.08252257160822,3.21293969093737,-32.8952809260689));
#30016=CARTESIAN_POINT('Ctrl Pts',(0.777370039512734,3.30912431481032,-32.8749017878759));
#30017=CARTESIAN_POINT('Ctrl Pts',(0.527896504186848,3.35796886294455,-32.8583562129981));
#30018=CARTESIAN_POINT('Ctrl Pts',(0.17990431218647,3.38632571147815,-32.8365393294357));
#30019=CARTESIAN_POINT('Ctrl Pts',(0.0842079902564654,3.39005590231105,
-32.830658542228));
#30020=CARTESIAN_POINT('Ctrl Pts',(-0.0495985192761317,3.38960095676014,
-32.8226064202216));
#30021=CARTESIAN_POINT('Ctrl Pts',(-0.087668078497511,3.38883005523327,
-32.8203345422437));
#30022=CARTESIAN_POINT('Ctrl Pts',(-0.157433144747235,3.38624085355091,
-32.8162046717881));
#30023=CARTESIAN_POINT('Ctrl Pts',(-0.1891311919983,3.38461841379444,-32.8143409386869));
#30024=CARTESIAN_POINT('Ctrl Pts',(-0.25405906147528,3.38038012074537,-32.8105478928362));
#30025=CARTESIAN_POINT('Ctrl Pts',(-0.287282511437232,3.37771885157417,
-32.8086201810603));
#30026=CARTESIAN_POINT('Ctrl Pts',(-0.372205990094181,3.36965418544892,
-32.8037233990268));
#30027=CARTESIAN_POINT('Ctrl Pts',(-0.42383169661312,3.36355076122683,-32.8007759079591));
#30028=CARTESIAN_POINT('Ctrl Pts',(-0.673641776112479,3.32817379114229,
-32.7866261091439));
#30029=CARTESIAN_POINT('Ctrl Pts',(-0.869110742142148,3.28255858320625,
-32.7759302171727));
#30030=CARTESIAN_POINT('Ctrl Pts',(-1.26049061512538,3.15378716126089,-32.7540579221479));
#30031=CARTESIAN_POINT('Ctrl Pts',(-1.45489817716245,3.06895119036221,-32.7429292510127));
#30032=CARTESIAN_POINT('Ctrl Pts',(-1.67100262171976,2.94947485907622,-32.7289697065074));
#30033=CARTESIAN_POINT('Ctrl Pts',(-1.70163241128534,2.93191040756535,-32.7269507652376));
#30034=CARTESIAN_POINT('Ctrl Pts',(-1.74903570035984,2.90373428665369,-32.7237538429069));
#30035=CARTESIAN_POINT('Ctrl Pts',(-1.76600063746828,2.89344783859725,-32.7225949434459));
#30036=CARTESIAN_POINT('Ctrl Pts',(-1.79834455594705,2.8734461530914,-32.7203551105036));
#30037=CARTESIAN_POINT('Ctrl Pts',(-1.81373722503326,2.86375507991179,-32.7192756141966));
#30038=CARTESIAN_POINT('Ctrl Pts',(-1.85200492281088,2.83922985079057,-32.7165591055902));
#30039=CARTESIAN_POINT('Ctrl Pts',(-1.87478013897929,2.82424285554802,-32.7149128092817));
#30040=CARTESIAN_POINT('Ctrl Pts',(-1.96798067435477,2.76128910996908,-32.7080610152107));
#30041=CARTESIAN_POINT('Ctrl Pts',(-2.03676150607504,2.71095294159866,-32.7027309399712));
#30042=CARTESIAN_POINT('Ctrl Pts',(-2.24534396095765,2.54588390676022,-32.6858615489026));
#30043=CARTESIAN_POINT('Ctrl Pts',(-2.3779150878297,2.42252233708731,-32.6741084802996));
#30044=CARTESIAN_POINT('Ctrl Pts',(-2.61379999917827,2.16491184293108,-32.6517737266632));
#30045=CARTESIAN_POINT('Ctrl Pts',(-2.71817304432898,2.03232424853033,-32.6411967970714));
#30046=CARTESIAN_POINT('Ctrl Pts',(-2.8393777943812,1.85221424424317,-32.6280489941279));
#30047=CARTESIAN_POINT('Ctrl Pts',(-2.86562505852472,1.81134128587344,-32.6251385359313));
#30048=CARTESIAN_POINT('Ctrl Pts',(-2.90634038473951,1.74483678140426,-32.6205166987396));
#30049=CARTESIAN_POINT('Ctrl Pts',(-2.92136814978037,1.7195575128752,-32.6187854777751));
#30050=CARTESIAN_POINT('Ctrl Pts',(-2.95209327289725,1.66630696386272,-32.6151906042328));
#30051=CARTESIAN_POINT('Ctrl Pts',(-2.96772648642255,1.63830192397688,-32.6133293418135));
#30052=CARTESIAN_POINT('Ctrl Pts',(-3.00445897765211,1.57024837133797,-32.608874096377));
#30053=CARTESIAN_POINT('Ctrl Pts',(-3.02515840316091,1.52999039336254,-32.6062940755834));
#30054=CARTESIAN_POINT('Ctrl Pts',(-3.10241675143629,1.37202979350173,-32.5963696053623));
#30055=CARTESIAN_POINT('Ctrl Pts',(-3.15296491172492,1.25150804308817,-32.5892242917128));
#30056=CARTESIAN_POINT('Ctrl Pts',(-3.25034058446021,0.975660823085285,
-32.5734851217536));
#30057=CARTESIAN_POINT('Ctrl Pts',(-3.29323273681335,0.819296151041877,
-32.564979006293));
#30058=CARTESIAN_POINT('Ctrl Pts',(-3.32508144317155,0.658969485091512,
-32.5562530931637));
#30059=CARTESIAN_POINT('Ctrl Pts',(-3.32537743267149,0.657474194383888,
-32.5561717093476));
#30060=CARTESIAN_POINT('Ctrl Pts',(-3.33982528833165,0.584226641344357,
-32.5521849965956));
#30061=CARTESIAN_POINT('Ctrl Pts',(-3.35165186773748,0.512037809713025,
-32.5482521781375));
#30062=CARTESIAN_POINT('Ctrl Pts',(-3.37093460479456,0.364579209396957,
-32.5401177403836));
#30063=CARTESIAN_POINT('Ctrl Pts',(-3.37822501044656,0.289330795697706,
-32.5359138068072));
#30064=CARTESIAN_POINT('Ctrl Pts',(-3.38465642193842,0.187616451665435,
-32.5300873279099));
#30065=CARTESIAN_POINT('Ctrl Pts',(-3.38601220147362,0.161308114618323,
-32.5285673520936));
#30066=CARTESIAN_POINT('Ctrl Pts',(-3.38777324823923,0.117120526173392,
-32.5259887268538));
#30067=CARTESIAN_POINT('Ctrl Pts',(-3.38834392234425,0.0992484370684867,
-32.5249387123237));
#30068=CARTESIAN_POINT('Ctrl Pts',(-3.38911919979665,0.0669619443574267,
-32.5230278783059));
#30069=CARTESIAN_POINT('Ctrl Pts',(-3.38937330428478,0.0525494048286926,
-32.5221699614643));
#30070=CARTESIAN_POINT('Ctrl Pts',(-3.38967720194844,0.025538900972615,
-32.5205534547019));
#30071=CARTESIAN_POINT('Ctrl Pts',(-3.38974870430922,0.0129413635074798,
-32.5197959849455));
#30072=CARTESIAN_POINT('Ctrl Pts',(-3.38974998254981,0.000343952908442827,
-32.5190351755825));
#30073=CARTESIAN_POINT('',(-3.38974872454211,-0.00294057224222385,-30.0160178032104));
#30074=CARTESIAN_POINT('Ctrl Pts',(-3.38974998234963,0.000345920085544606,
-32.5190352943883));
#30075=CARTESIAN_POINT('Ctrl Pts',(-3.38975151971354,-0.0147190602479393,
-32.5181254587716));
#30076=CARTESIAN_POINT('Ctrl Pts',(-3.38965262764753,-0.0297836515172151,
-32.5172108597942));
#30077=CARTESIAN_POINT('Ctrl Pts',(-3.38910134638758,-0.0714486137903887,
-32.5146689626663));
#30078=CARTESIAN_POINT('Ctrl Pts',(-3.38843622082854,-0.0980445619635314,
-32.5130324841435));
#30079=CARTESIAN_POINT('Ctrl Pts',(-3.38310214657387,-0.24302633539895,
-32.5040452157681));
#30080=CARTESIAN_POINT('Ctrl Pts',(-3.37254214438138,-0.361106114222097,
-32.4964868766424));
#30081=CARTESIAN_POINT('Ctrl Pts',(-3.31992162810586,-0.730236373057563,
-32.4725274243699));
#30082=CARTESIAN_POINT('Ctrl Pts',(-3.25577428233754,-0.977288287365443,
-32.4560766797842));
#30083=CARTESIAN_POINT('Ctrl Pts',(-3.14088421989889,-1.27656623872225,
-32.4363955308566));
#30084=CARTESIAN_POINT('Ctrl Pts',(-3.11539122277617,-1.33757746549877,
-32.4323913716381));
#30085=CARTESIAN_POINT('Ctrl Pts',(-3.07323823294502,-1.43070464592318,
-32.426289868579));
#30086=CARTESIAN_POINT('Ctrl Pts',(-3.05782253215433,-1.46336274807284,
-32.4241521218584));
#30087=CARTESIAN_POINT('Ctrl Pts',(-3.02808668173032,-1.52383538469427,
-32.420195677516));
#30088=CARTESIAN_POINT('Ctrl Pts',(-3.01389780054778,-1.55170982325741,
-32.4183727837166));
#30089=CARTESIAN_POINT('Ctrl Pts',(-2.98103854325281,-1.6141110811488,-32.4142918379305));
#30090=CARTESIAN_POINT('Ctrl Pts',(-2.96215004564179,-1.64851832480108,
-32.4120415954188));
#30091=CARTESIAN_POINT('Ctrl Pts',(-2.90109981451286,-1.75528851497847,
-32.4050514933619));
#30092=CARTESIAN_POINT('Ctrl Pts',(-2.85685035878308,-1.82642421983521,
-32.4003844402938));
#30093=CARTESIAN_POINT('Ctrl Pts',(-2.66269852626281,-2.11419371528011,
-32.3813320629483));
#30094=CARTESIAN_POINT('Ctrl Pts',(-2.49045186970781,-2.31461078277455,
-32.3677164724198));
#30095=CARTESIAN_POINT('Ctrl Pts',(-2.24337340630939,-2.54223262717457,
-32.3495979173992));
#30096=CARTESIAN_POINT('Ctrl Pts',(-2.18844024476452,-2.58967164110989,
-32.3456386241792));
#30097=CARTESIAN_POINT('Ctrl Pts',(-2.0936412999557,-2.66636633690654,-32.3388403996283));
#30098=CARTESIAN_POINT('Ctrl Pts',(-2.05458039961716,-2.69657972356982,
-32.336048410294));
#30099=CARTESIAN_POINT('Ctrl Pts',(-1.99676715231779,-2.73931251908909,
-32.3319068937879));
#30100=CARTESIAN_POINT('Ctrl Pts',(-1.97852624161241,-2.75251630138135,
-32.3305988955317));
#30101=CARTESIAN_POINT('Ctrl Pts',(-1.94573637166981,-2.77575708617915,
-32.3282427403961));
#30102=CARTESIAN_POINT('Ctrl Pts',(-1.93123837070507,-2.78586355586294,
-32.3271991307333));
#30103=CARTESIAN_POINT('Ctrl Pts',(-1.89786797103962,-2.80874018489604,
-32.3247927102158));
#30104=CARTESIAN_POINT('Ctrl Pts',(-1.87894531895663,-2.82143379993151,
-32.323425287011));
#30105=CARTESIAN_POINT('Ctrl Pts',(-1.81729893291112,-2.86189199647878,
-32.318964980714));
#30106=CARTESIAN_POINT('Ctrl Pts',(-1.77407850648132,-2.88888319078675,
-32.315829462847));
#30107=CARTESIAN_POINT('Ctrl Pts',(-1.4918076705427,-3.05643827710386,-32.2953771169475));
#30108=CARTESIAN_POINT('Ctrl Pts',(-1.23687917387077,-3.16819295326867,
-32.2771270209124));
#30109=CARTESIAN_POINT('Ctrl Pts',(-0.850753381473515,-3.28365985675345,
-32.2516615987019));
#30110=CARTESIAN_POINT('Ctrl Pts',(-0.728411976184832,-3.31294809311484,
-32.2438700378893));
#30111=CARTESIAN_POINT('Ctrl Pts',(-0.560656866619073,-3.34336265233418,
-32.2335828126538));
#30112=CARTESIAN_POINT('Ctrl Pts',(-0.516443766568526,-3.35047699128768,
-32.2309076030414));
#30113=CARTESIAN_POINT('Ctrl Pts',(-0.440424128754461,-3.36116868443577,
-32.2263674332771));
#30114=CARTESIAN_POINT('Ctrl Pts',(-0.408684962785469,-3.36517533621465,
-32.2244895101848));
#30115=CARTESIAN_POINT('Ctrl Pts',(-0.343581202104071,-3.37245913042291,
-32.2206719825815));
#30116=CARTESIAN_POINT('Ctrl Pts',(-0.310215131144468,-3.37569182795055,
-32.2187339399547));
#30117=CARTESIAN_POINT('Ctrl Pts',(-0.224031479536461,-3.38275313537361,
-32.213772409949));
#30118=CARTESIAN_POINT('Ctrl Pts',(-0.171161347240629,-3.38584008708192,
-32.2107716907595));
#30119=CARTESIAN_POINT('Ctrl Pts',(0.152403171726233,-3.39713327359408,
-32.192629532053));
#30120=CARTESIAN_POINT('Ctrl Pts',(0.423194586134779,-3.37411556981751,
-32.1784944292937));
#30121=CARTESIAN_POINT('Ctrl Pts',(0.832448089137162,-3.28923784710404,
-32.156205297257));
#30122=CARTESIAN_POINT('Ctrl Pts',(0.974410596902226,-3.25001088267025,
-32.1482686350341));
#30123=CARTESIAN_POINT('Ctrl Pts',(1.14268809315137,-3.19149386898141,-32.1381440005817));
#30124=CARTESIAN_POINT('Ctrl Pts',(1.17187332846928,-3.18089326320842,-32.1363609225856));
#30125=CARTESIAN_POINT('Ctrl Pts',(1.2186235246861,-3.16318204707204,-32.1334546956653));
#30126=CARTESIAN_POINT('Ctrl Pts',(1.23628229264225,-3.15632222898905,-32.1323453129663));
#30127=CARTESIAN_POINT('Ctrl Pts',(1.27135219907536,-3.1423593414256,-32.1301171321725));
#30128=CARTESIAN_POINT('Ctrl Pts',(1.28876355065354,-3.13525869979164,-32.1289984872903));
#30129=CARTESIAN_POINT('Ctrl Pts',(1.33415312945107,-3.11630610314004,-32.1260514332473));
#30130=CARTESIAN_POINT('Ctrl Pts',(1.36203211367256,-3.10422239592704,-32.1242103959884));
#30131=CARTESIAN_POINT('Ctrl Pts',(1.50044861992926,-3.04200440081785,-32.1149279386334));
#30132=CARTESIAN_POINT('Ctrl Pts',(1.60839185426979,-2.98633679156353,-32.1072358396914));
#30133=CARTESIAN_POINT('Ctrl Pts',(1.89121686555835,-2.82069285590838,-32.086233579308));
#30134=CARTESIAN_POINT('Ctrl Pts',(2.05944080312321,-2.70031919651049,-32.0728324592527));
#30135=CARTESIAN_POINT('Ctrl Pts',(2.30078306400376,-2.49187677696339,-32.0527815041129));
#30136=CARTESIAN_POINT('Ctrl Pts',(2.38218971825948,-2.41417250712736,-32.0458398222432));
#30137=CARTESIAN_POINT('Ctrl Pts',(2.48938838697,-2.30113577159368,-32.0364544963012));
#30138=CARTESIAN_POINT('Ctrl Pts',(2.51858351714032,-2.2691447081807,-32.0338704792926));
#30139=CARTESIAN_POINT('Ctrl Pts',(2.56811024884799,-2.21274108673938,-32.0294354746061));
#30140=CARTESIAN_POINT('Ctrl Pts',(2.58872602650768,-2.18858653663426,-32.0275730486659));
#30141=CARTESIAN_POINT('Ctrl Pts',(2.63071460277566,-2.1379669255012,-32.0237438125809));
#30142=CARTESIAN_POINT('Ctrl Pts',(2.65203462269421,-2.11146261552585,-32.021779218035));
#30143=CARTESIAN_POINT('Ctrl Pts',(2.70704039947975,-2.0409335290338,-32.0166528116558));
#30144=CARTESIAN_POINT('Ctrl Pts',(2.74005214706653,-1.9963947773594,-32.0135168930657));
#30145=CARTESIAN_POINT('Ctrl Pts',(2.90905725893796,-1.75628223338974,-31.9970972469591));
#30146=CARTESIAN_POINT('Ctrl Pts',(3.02524537975443,-1.54759234531545,-31.9845509433189));
#30147=CARTESIAN_POINT('Ctrl Pts',(3.16517969934154,-1.21908522433469,-31.965579495503));
#30148=CARTESIAN_POINT('Ctrl Pts',(3.205972530853,-1.10737005535036,-31.9592385609194));
#30149=CARTESIAN_POINT('Ctrl Pts',(3.25455517536627,-0.948932646057613,
-31.9501262309488));
#30150=CARTESIAN_POINT('Ctrl Pts',(3.26736618886803,-0.903836477129002,
-31.9475191588104));
#30151=CARTESIAN_POINT('Ctrl Pts',(3.28835846768625,-0.823650830252975,
-31.942837139873));
#30152=CARTESIAN_POINT('Ctrl Pts',(3.29692331742208,-0.788668830872896,
-31.940779141611));
#30153=CARTESIAN_POINT('Ctrl Pts',(3.30937183520242,-0.734072585114871,
-31.9375341131935));
#30154=CARTESIAN_POINT('Ctrl Pts',(3.31364228905111,-0.714548277460725,
-31.9363671122508));
#30155=CARTESIAN_POINT('Ctrl Pts',(3.32141282648714,-0.677453212267713,
-31.9341355646797));
#30156=CARTESIAN_POINT('Ctrl Pts',(3.32494666421573,-0.659890629650698,
-31.9330728304017));
#30157=CARTESIAN_POINT('Ctrl Pts',(3.33258300824863,-0.620319869497174,
-31.9306654097903));
#30158=CARTESIAN_POINT('Ctrl Pts',(3.33660701655666,-0.598297423062006,
-31.9293166849474));
#30159=CARTESIAN_POINT('Ctrl Pts',(3.35062524030221,-0.517034646906688,
-31.9243110963898));
#30160=CARTESIAN_POINT('Ctrl Pts',(3.35926169643006,-0.457574364224408,
-31.9205924114407));
#30161=CARTESIAN_POINT('Ctrl Pts',(3.39743511407486,-0.134635786069528,
-31.9002004799878));
#30162=CARTESIAN_POINT('Ctrl Pts',(3.39756389851286,0.1313917637633,-31.8827908067997));
#30163=CARTESIAN_POINT('Ctrl Pts',(3.35225191822044,0.517863932089777,-31.8582184823072));
#30164=CARTESIAN_POINT('Ctrl Pts',(3.33106915431097,0.640124794758583,-31.850537157987));
#30165=CARTESIAN_POINT('Ctrl Pts',(3.29322028354437,0.804421689542251,-31.8403658271591));
#30166=CARTESIAN_POINT('Ctrl Pts',(3.28235135109967,0.847681532885321,-31.8377016180511));
#30167=CARTESIAN_POINT('Ctrl Pts',(3.26223363223903,0.921552051855528,-31.8331741912953));
#30168=CARTESIAN_POINT('Ctrl Pts',(3.25339990815082,0.952268657884555,-31.8312981964903));
#30169=CARTESIAN_POINT('Ctrl Pts',(3.23439814928035,1.01498811684034,-31.8274796076031));
#30170=CARTESIAN_POINT('Ctrl Pts',(3.22418635551133,1.04697408130729,-31.8255386502022));
#30171=CARTESIAN_POINT('Ctrl Pts',(3.19656176751911,1.12926117191592,-31.8205589283141));
#30172=CARTESIAN_POINT('Ctrl Pts',(3.17843613728034,1.17931424088149,-31.8175432698798));
#30173=CARTESIAN_POINT('Ctrl Pts',(3.06606107300469,1.46819220847407,-31.8001782209697));
#30174=CARTESIAN_POINT('Ctrl Pts',(2.94610490198888,1.69611166540161,-31.7867171792342));
#30175=CARTESIAN_POINT('Ctrl Pts',(2.71865546621671,2.03002560661381,-31.7652171753579));
#30176=CARTESIAN_POINT('Ctrl Pts',(2.627915131404,2.14619332135222,-31.757316805065));
#30177=CARTESIAN_POINT('Ctrl Pts',(2.50426879268441,2.28484754334589,-31.7468520104919));
#30178=CARTESIAN_POINT('Ctrl Pts',(2.47812974048097,2.31317167783212,-31.744654557653));
#30179=CARTESIAN_POINT('Ctrl Pts',(2.43735725880367,2.35586817983901,-31.7412380095916));
#30180=CARTESIAN_POINT('Ctrl Pts',(2.42306607845527,2.37056449416151,-31.7400424866073));
#30181=CARTESIAN_POINT('Ctrl Pts',(2.3960218696451,2.39787530923101,-31.7377817819865));
#30182=CARTESIAN_POINT('Ctrl Pts',(2.38330065572409,2.41051959691851,-31.7367188688881));
#30183=CARTESIAN_POINT('Ctrl Pts',(2.35499716151906,2.43820888754345,-31.7343558485799));
#30184=CARTESIAN_POINT('Ctrl Pts',(2.33936989640805,2.45320660461194,-31.7330524615085));
#30185=CARTESIAN_POINT('Ctrl Pts',(2.28458935125208,2.50478089936443,-31.7284914248393));
#30186=CARTESIAN_POINT('Ctrl Pts',(2.24471508978919,2.54057658310158,-31.725185388131));
#30187=CARTESIAN_POINT('Ctrl Pts',(1.99711839932039,2.75246749035028,-31.704825440136));
#30188=CARTESIAN_POINT('Ctrl Pts',(1.76964422816903,2.90395081557588,-31.6869201017299));
#30189=CARTESIAN_POINT('Ctrl Pts',(1.41486497211439,3.08288678069223,-31.6618189514095));
#30190=CARTESIAN_POINT('Ctrl Pts',(1.30020588933392,3.1329704842609,-31.654070958215));
#30191=CARTESIAN_POINT('Ctrl Pts',(1.14113539300481,3.19221141665818,-31.6438294989835));
#30192=CARTESIAN_POINT('Ctrl Pts',(1.09893419962264,3.20698419445037,-31.6411586085529));
#30193=CARTESIAN_POINT('Ctrl Pts',(1.02606713926823,3.23088437154998,-31.6366234440141));
#30194=CARTESIAN_POINT('Ctrl Pts',(0.995542485260382,3.24042016726061,-31.6347462799687));
#30195=CARTESIAN_POINT('Ctrl Pts',(0.932733427338256,3.25907017390353,-31.6309283468252));
#30196=CARTESIAN_POINT('Ctrl Pts',(0.900439463139534,3.26813998084528,-31.6289891688546));
#30197=CARTESIAN_POINT('Ctrl Pts',(0.816726664639992,3.2903157508031,-31.624020548206));
#30198=CARTESIAN_POINT('Ctrl Pts',(0.765124283453533,3.30269669230534,-31.6210140052148));
#30199=CARTESIAN_POINT('Ctrl Pts',(0.4297043246537,3.37488994330375,-31.6017898870362));
#30200=CARTESIAN_POINT('Ctrl Pts',(0.139512299108629,3.39927465568513,-31.5867512803949));
#30201=CARTESIAN_POINT('Ctrl Pts',(-0.279219414748744,3.38069633815382,
-31.5643070827361));
#30202=CARTESIAN_POINT('Ctrl Pts',(-0.40774617734941,3.36761161432466,-31.5572936131331));
#30203=CARTESIAN_POINT('Ctrl Pts',(-0.565179005201581,3.34243914711843,
-31.5482249953726));
#30204=CARTESIAN_POINT('Ctrl Pts',(-0.595090835820295,3.33724340164118,
-31.546480284736));
#30205=CARTESIAN_POINT('Ctrl Pts',(-0.643403867305303,3.32818117059328,
-31.5436212676159));
#30206=CARTESIAN_POINT('Ctrl Pts',(-0.661850424346191,3.32456198972908,
-31.542519923956));
#30207=CARTESIAN_POINT('Ctrl Pts',(-0.698830184186938,3.31698666663779,
-31.5402907814393));
#30208=CARTESIAN_POINT('Ctrl Pts',(-0.717362173257835,3.31302816883222,
-31.5391629042066));
#30209=CARTESIAN_POINT('Ctrl Pts',(-0.766195590686987,3.30216825295493,
-31.5361641317044));
#30210=CARTESIAN_POINT('Ctrl Pts',(-0.796436324362887,3.29500529393247,
-31.5342798378231));
#30211=CARTESIAN_POINT('Ctrl Pts',(-0.966538458874326,3.25223573177051,
-31.5235426059));
#30212=CARTESIAN_POINT('Ctrl Pts',(-1.10410178664264,3.20814367359347,-31.5143353183145));
#30213=CARTESIAN_POINT('Ctrl Pts',(-1.4137763253231,3.08660436933167,-31.4929471636992));
#30214=CARTESIAN_POINT('Ctrl Pts',(-1.58310081161304,3.00328010318528,-31.4807663393065));
#30215=CARTESIAN_POINT('Ctrl Pts',(-1.83694710054287,2.85089871606752,-31.4621868410934));
#30216=CARTESIAN_POINT('Ctrl Pts',(-1.92657626219327,2.79111191646911,-31.4555516579836));
#30217=CARTESIAN_POINT('Ctrl Pts',(-2.04757908680858,2.70178633571687,-31.4464964842643));
#30218=CARTESIAN_POINT('Ctrl Pts',(-2.08146204766934,2.67577007855744,-31.4439491146149));
#30219=CARTESIAN_POINT('Ctrl Pts',(-2.13959288511099,2.62936305968285,-31.4395560183774));
#30220=CARTESIAN_POINT('Ctrl Pts',(-2.1640628729233,2.60926039257545,-31.437699457054));
#30221=CARTESIAN_POINT('Ctrl Pts',(-2.2143989852583,2.56671281344454,-31.4338634098585));
#30222=CARTESIAN_POINT('Ctrl Pts',(-2.24021398478587,2.54421283666147,-31.43188642674));
#30223=CARTESIAN_POINT('Ctrl Pts',(-2.30776730045797,2.48350884524459,-31.4266834914391));
#30224=CARTESIAN_POINT('Ctrl Pts',(-2.34889843289533,2.44464368757765,-31.423484932569));
#30225=CARTESIAN_POINT('Ctrl Pts',(-2.54717917518094,2.24765963631828,-31.4078699265141));
#30226=CARTESIAN_POINT('Ctrl Pts',(-2.68943915218223,2.07533677068973,-31.3960814686697));
#30227=CARTESIAN_POINT('Ctrl Pts',(-2.88514301046738,1.78402392867721,-31.3774518676823));
#30228=CARTESIAN_POINT('Ctrl Pts',(-2.95044718856002,1.67381286684701,-31.3706453191104));
#30229=CARTESIAN_POINT('Ctrl Pts',(-3.04205500627029,1.49711477012226,-31.3597219688441));
#30230=CARTESIAN_POINT('Ctrl Pts',(-3.07275806088825,1.4330414655169,-31.3557581511853));
#30231=CARTESIAN_POINT('Ctrl Pts',(-3.11179268219523,1.34454879119662,-31.3502185318787));
#30232=CARTESIAN_POINT('Ctrl Pts',(-3.12189375193288,1.32092560914252,-31.3487335402309));
#30233=CARTESIAN_POINT('Ctrl Pts',(-3.13858774022151,1.28062237411466,-31.3461858765785));
#30234=CARTESIAN_POINT('Ctrl Pts',(-3.1453184926567,1.26400088530767,-31.3451310915843));
#30235=CARTESIAN_POINT('Ctrl Pts',(-3.15946450275532,1.22825477427803,-31.3428527810384));
#30236=CARTESIAN_POINT('Ctrl Pts',(-3.16683821919544,1.20911595026986,-31.3416271758218));
#30237=CARTESIAN_POINT('Ctrl Pts',(-3.18720438822845,1.15479009275808,-31.3381343733759));
#30238=CARTESIAN_POINT('Ctrl Pts',(-3.19978675257161,1.11945364383098,-31.3358460998761));
#30239=CARTESIAN_POINT('Ctrl Pts',(-3.25740035908007,0.948737477520367,
-31.3247368281054));
#30240=CARTESIAN_POINT('Ctrl Pts',(-3.29443792279989,0.810822123735642,
-31.3156054528134));
#30241=CARTESIAN_POINT('Ctrl Pts',(-3.34674789599764,0.551790708433814,
-31.2985999385216));
#30242=CARTESIAN_POINT('Ctrl Pts',(-3.36438901312496,0.431372879284578,
-31.2907501180964));
#30243=CARTESIAN_POINT('Ctrl Pts',(-3.38493988534087,0.20779045872944,-31.2764460155949));
#30244=CARTESIAN_POINT('Ctrl Pts',(-3.38968826149535,0.104933788933924,
-31.2699692516742));
#30245=CARTESIAN_POINT('Ctrl Pts',(-3.38979385698205,-0.0728188464554172,
-31.2589960814788));
#30246=CARTESIAN_POINT('Ctrl Pts',(-3.38736030023665,-0.147636275167262,
-31.2544439856543));
#30247=CARTESIAN_POINT('Ctrl Pts',(-3.3799777540892,-0.259958664242163,
-31.2477087911456));
#30248=CARTESIAN_POINT('Ctrl Pts',(-3.3768754011307,-0.297558098380861,
-31.2454707990118));
#30249=CARTESIAN_POINT('Ctrl Pts',(-3.3700604981018,-0.366157697312476,
-31.2414162325367));
#30250=CARTESIAN_POINT('Ctrl Pts',(-3.3665461481857,-0.397172944746368,
-31.2395938076593));
#30251=CARTESIAN_POINT('Ctrl Pts',(-3.35788342164304,-0.465210476368273,
-31.2356177905748));
#30252=CARTESIAN_POINT('Ctrl Pts',(-3.35255004886927,-0.502205324968264,
-31.233470124624));
#30253=CARTESIAN_POINT('Ctrl Pts',(-3.33501390700637,-0.611064454422087,
-31.227187101642));
#30254=CARTESIAN_POINT('Ctrl Pts',(-3.32110365733512,-0.682633908516753,
-31.2231040606011));
#30255=CARTESIAN_POINT('Ctrl Pts',(-3.28287462343786,-0.850263589851162,
-31.2136076618927));
#30256=CARTESIAN_POINT('Ctrl Pts',(-3.25663117512684,-0.945816613963547,
-31.2082480238829));
#30257=CARTESIAN_POINT('Ctrl Pts',(-3.18734777525435,-1.16072630669105,
-31.1961568670839));
#30258=CARTESIAN_POINT('Ctrl Pts',(-3.14171992980308,-1.27908853430591,
-31.1894721588661));
#30259=CARTESIAN_POINT('Ctrl Pts',(-3.03017314661259,-1.52620404824792,
-31.1750364905036));
#30260=CARTESIAN_POINT('Ctrl Pts',(-2.96243489678285,-1.65385008477966,
-31.1672810596357));
#30261=CARTESIAN_POINT('Ctrl Pts',(-2.86708023764613,-1.80877519681317,
-31.1570278564257));
#30262=CARTESIAN_POINT('Ctrl Pts',(-2.84685603117243,-1.84044214728108,
-31.1548849091984));
#30263=CARTESIAN_POINT('Ctrl Pts',(-2.81477756377269,-1.88887626923582,
-31.1515231625217));
#30264=CARTESIAN_POINT('Ctrl Pts',(-2.80328972537393,-1.90588377483582,
-31.1503262756566));
#30265=CARTESIAN_POINT('Ctrl Pts',(-2.78147809194234,-1.93755158959592,
-31.1480646615379));
#30266=CARTESIAN_POINT('Ctrl Pts',(-2.77119133144748,-1.952235919978,-31.1470022325769));
#30267=CARTESIAN_POINT('Ctrl Pts',(-2.74589752158615,-1.9877400555362,-31.1444007790509));
#30268=CARTESIAN_POINT('Ctrl Pts',(-2.73076978621036,-2.00847205979082,
-31.1428541362297));
#30269=CARTESIAN_POINT('Ctrl Pts',(-2.67302123364847,-2.08575576116977,
-31.1369902723998));
#30270=CARTESIAN_POINT('Ctrl Pts',(-2.62886948022658,-2.14113602896012,
-31.1325876610165));
#30271=CARTESIAN_POINT('Ctrl Pts',(-2.50057659895951,-2.29210164758648,
-31.1201008439151));
#30272=CARTESIAN_POINT('Ctrl Pts',(-2.41273708626509,-2.3843889440527,-31.11189525565));
#30273=CARTESIAN_POINT('Ctrl Pts',(-2.15660742127133,-2.62480849445823,
-31.0892696180546));
#30274=CARTESIAN_POINT('Ctrl Pts',(-1.97848156117016,-2.76155976973937,
-31.0749557831196));
#30275=CARTESIAN_POINT('Ctrl Pts',(-1.74012771650372,-2.90956270561394,
-31.0578493421647));
#30276=CARTESIAN_POINT('Ctrl Pts',(-1.69137096811816,-2.93817365481448,
-31.0544441629388));
#30277=CARTESIAN_POINT('Ctrl Pts',(-1.61197293424524,-2.98213346563277,
-31.0490453406497));
#30278=CARTESIAN_POINT('Ctrl Pts',(-1.58177641138783,-2.99825953843388,
-31.0470249721748));
#30279=CARTESIAN_POINT('Ctrl Pts',(-1.52318100968024,-3.02841999715123,
-31.0431657423445));
#30280=CARTESIAN_POINT('Ctrl Pts',(-1.49481965507596,-3.04251908216918,
-31.0413248026946));
#30281=CARTESIAN_POINT('Ctrl Pts',(-1.42772787918613,-3.07470730768495,
-31.0370306620228));
#30282=CARTESIAN_POINT('Ctrl Pts',(-1.3888442303788,-3.09246566025329,-31.0345887918594));
#30283=CARTESIAN_POINT('Ctrl Pts',(-1.25065984687188,-3.15244290847438,
-31.0260636256352));
#30284=CARTESIAN_POINT('Ctrl Pts',(-1.14968624739726,-3.19065366171112,
-31.0201103846451));
#30285=CARTESIAN_POINT('Ctrl Pts',(-0.867134331467032,-3.28241815109112,
-31.0039929771783));
#30286=CARTESIAN_POINT('Ctrl Pts',(-0.682640247903144,-3.32568702675918,
-30.9940776699118));
#30287=CARTESIAN_POINT('Ctrl Pts',(-0.353777072665913,-3.3742806976672,
-30.9763369476531));
#30288=CARTESIAN_POINT('Ctrl Pts',(-0.210884370300202,-3.38621442189802,
-30.9685988550972));
#30289=CARTESIAN_POINT('Ctrl Pts',(-0.0366170520661458,-3.38969462241773,
-30.9586938126423));
#30290=CARTESIAN_POINT('Ctrl Pts',(-0.00554678726381804,-3.38988783451179,
-30.9569096196713));
#30291=CARTESIAN_POINT('Ctrl Pts',(0.0444688304589123,-3.38951126902333,
-30.9540020189534));
#30292=CARTESIAN_POINT('Ctrl Pts',(0.0634150740758199,-3.38920973245243,
-30.952892400916));
#30293=CARTESIAN_POINT('Ctrl Pts',(0.101151720335835,-3.38829261295725,
-30.950664219388));
#30294=CARTESIAN_POINT('Ctrl Pts',(0.119941480844943,-3.38767951582361,
-30.9495458157444));
#30295=CARTESIAN_POINT('Ctrl Pts',(0.169065348107693,-3.3856674489129,-30.9466001496575));
#30296=CARTESIAN_POINT('Ctrl Pts',(0.199386880875708,-3.38401712455632,
-30.9447602798778));
#30297=CARTESIAN_POINT('Ctrl Pts',(0.358621538985245,-3.37320292966175,
-30.9349982333533));
#30298=CARTESIAN_POINT('Ctrl Pts',(0.486945130178296,-3.35707998583838,
-30.9267903019519));
#30299=CARTESIAN_POINT('Ctrl Pts',(0.898948223787798,-3.28119397567878,
-30.8999118934604));
#30300=CARTESIAN_POINT('Ctrl Pts',(1.17602920784825,-3.1923896776265,-30.8811395999651));
#30301=CARTESIAN_POINT('Ctrl Pts',(1.48654697431218,-3.04686791706524,-30.8602883492586));
#30302=CARTESIAN_POINT('Ctrl Pts',(1.53410575535585,-3.02320128617517,-30.8570953911699));
#30303=CARTESIAN_POINT('Ctrl Pts',(1.61076928485538,-2.98277607231283,-30.8519470839224));
#30304=CARTESIAN_POINT('Ctrl Pts',(1.64021452933924,-2.96668623292598,-30.8499693252217));
#30305=CARTESIAN_POINT('Ctrl Pts',(1.69724219777491,-2.93441581226866,-30.8461366071284));
#30306=CARTESIAN_POINT('Ctrl Pts',(1.72484405320441,-2.91827694557501,-30.8442804495745));
#30307=CARTESIAN_POINT('Ctrl Pts',(1.79045444548963,-2.87865827583648,-30.8398632985484));
#30308=CARTESIAN_POINT('Ctrl Pts',(1.82823571109384,-2.85481260980144,-30.8373156410031));
#30309=CARTESIAN_POINT('Ctrl Pts',(1.96963375714398,-2.7616104762695,-30.8277515771831));
#30310=CARTESIAN_POINT('Ctrl Pts',(2.06987222650949,-2.68730026220169,-30.8209148612623));
#30311=CARTESIAN_POINT('Ctrl Pts',(2.37343823670961,-2.43517017810186,-30.7996416203131));
#30312=CARTESIAN_POINT('Ctrl Pts',(2.55971696357321,-2.23854577817081,-30.7857669976423));
#30313=CARTESIAN_POINT('Ctrl Pts',(2.75383891590257,-1.97733759359598,-30.7677347445065));
#30314=CARTESIAN_POINT('Ctrl Pts',(2.78588022888441,-1.93193255319577,-30.7646099781548));
#30315=CARTESIAN_POINT('Ctrl Pts',(2.82901226379223,-1.86750566617952,-30.760159203402));
#30316=CARTESIAN_POINT('Ctrl Pts',(2.84105706949321,-1.84913019440083,-30.7588879068001));
#30317=CARTESIAN_POINT('Ctrl Pts',(2.86264322671582,-1.81548969573245,-30.7565546544792));
#30318=CARTESIAN_POINT('Ctrl Pts',(2.87224336388092,-1.80026307194904,-30.7554963608487));
#30319=CARTESIAN_POINT('Ctrl Pts',(2.89241085282885,-1.76770375759864,-30.7532275169567));
#30320=CARTESIAN_POINT('Ctrl Pts',(2.9029443526255,-1.75035172354173,-30.7520151004813));
#30321=CARTESIAN_POINT('Ctrl Pts',(2.9325160771017,-1.70063644909779,-30.748534468944));
#30322=CARTESIAN_POINT('Ctrl Pts',(2.95117274399542,-1.66805097637427,-30.7462448436943));
#30323=CARTESIAN_POINT('Ctrl Pts',(3.03594077366381,-1.51412125799535,-30.7354139611759));
#30324=CARTESIAN_POINT('Ctrl Pts',(3.09512937938103,-1.38912485332063,-30.7265810616998));
#30325=CARTESIAN_POINT('Ctrl Pts',(3.24763652493694,-1.00854290486759,-30.7002075809962));
#30326=CARTESIAN_POINT('Ctrl Pts',(3.31804926228116,-0.744914686325395,
-30.6826943261426));
#30327=CARTESIAN_POINT('Ctrl Pts',(3.36337438075651,-0.425118351672462,
-30.6630892474786));
#30328=CARTESIAN_POINT('Ctrl Pts',(3.36939727275887,-0.374399891633058,
-30.6600235459955));
#30329=CARTESIAN_POINT('Ctrl Pts',(3.37743624900858,-0.29056542973385,-30.6550255082604));
#30330=CARTESIAN_POINT('Ctrl Pts',(3.38011626918766,-0.257522829622696,
-30.6530732210642));
#30331=CARTESIAN_POINT('Ctrl Pts',(3.38444456660954,-0.192296929617676,
-30.6492525912571));
#30332=CARTESIAN_POINT('Ctrl Pts',(3.3861194827012,-0.160118975755224,-30.6473836293678));
#30333=CARTESIAN_POINT('Ctrl Pts',(3.38907579492038,-0.0818362454576772,
-30.6428728641016));
#30334=CARTESIAN_POINT('Ctrl Pts',(3.38987556491014,-0.0357191256188062,
-30.6402459422375));
#30335=CARTESIAN_POINT('Ctrl Pts',(3.38930442140298,0.150408905845254,-30.629750063403));
#30336=CARTESIAN_POINT('Ctrl Pts',(3.3802012615131,0.290262323944762,-30.622113549099));
#30337=CARTESIAN_POINT('Ctrl Pts',(3.33566807784563,0.63917773754255,-30.6032417664708));
#30338=CARTESIAN_POINT('Ctrl Pts',(3.289248366481,0.8462076556394,-30.5922233648316));
#30339=CARTESIAN_POINT('Ctrl Pts',(3.19707720214389,1.12986473755841,-30.5760045100455));
#30340=CARTESIAN_POINT('Ctrl Pts',(3.16718736854465,1.21112298518536,-30.5712169438975));
#30341=CARTESIAN_POINT('Ctrl Pts',(3.12353346545864,1.317092038145,-30.564676904615));
#30342=CARTESIAN_POINT('Ctrl Pts',(3.11252184696708,1.3429074390276,-30.5630597173948));
#30343=CARTESIAN_POINT('Ctrl Pts',(3.09451938455987,1.38370080854579,-30.5604615088903));
#30344=CARTESIAN_POINT('Ctrl Pts',(3.08773709048788,1.3987700981898,-30.5594923380764));
#30345=CARTESIAN_POINT('Ctrl Pts',(3.07293157488553,1.43103340071639,-30.5573958955008));
#30346=CARTESIAN_POINT('Ctrl Pts',(3.06487369573038,1.4482107060445,-30.5562665474254));
#30347=CARTESIAN_POINT('Ctrl Pts',(3.04319024312234,1.49344263707125,-30.5532594900161));
#30348=CARTESIAN_POINT('Ctrl Pts',(3.02932124395607,1.52137780228847,-30.5513682562254));
#30349=CARTESIAN_POINT('Ctrl Pts',(2.94563728794847,1.68425317340055,-30.5401570101325));
#30350=CARTESIAN_POINT('Ctrl Pts',(2.86720422054698,1.81455772225659,-30.5304443542113));
#30351=CARTESIAN_POINT('Ctrl Pts',(2.62669602784828,2.15939238426101,-30.5033952975243));
#30352=CARTESIAN_POINT('Ctrl Pts',(2.44743232508606,2.36064138573899,-30.4861048516039));
#30353=CARTESIAN_POINT('Ctrl Pts',(2.20765789863874,2.57280197556173,-30.4666632546015));
#30354=CARTESIAN_POINT('Ctrl Pts',(2.16826854625577,2.60608429426852,-30.4635669205954));
#30355=CARTESIAN_POINT('Ctrl Pts',(2.10225677930828,2.65932824886272,-30.4585327183357));
#30356=CARTESIAN_POINT('Ctrl Pts',(2.07607369131353,2.67981873389785,-30.4565743160044));
#30357=CARTESIAN_POINT('Ctrl Pts',(2.02398217569842,2.71936299408918,-30.452751098815));
#30358=CARTESIAN_POINT('Ctrl Pts',(1.99809572754697,2.73843979449582,-30.4508855211496));
#30359=CARTESIAN_POINT('Ctrl Pts',(1.9347327171463,2.78375771747031,-30.4463989360582));
#30360=CARTESIAN_POINT('Ctrl Pts',(1.89698829102849,2.80961446114797,-30.4437924085016));
#30361=CARTESIAN_POINT('Ctrl Pts',(1.74519873107027,2.90914383004763,-30.4335530735329));
#30362=CARTESIAN_POINT('Ctrl Pts',(1.62729121329034,2.97670368884181,-30.4261373697569));
#30363=CARTESIAN_POINT('Ctrl Pts',(1.38411138919737,3.09726327145284,-30.4115570565399));
#30364=CARTESIAN_POINT('Ctrl Pts',(1.25907495134038,3.15016426924282,-30.4044048234716));
#30365=CARTESIAN_POINT('Ctrl Pts',(0.990894153168696,3.24510222204355,-30.3892677287199));
#30366=CARTESIAN_POINT('Ctrl Pts',(0.847475427105129,3.28547363548857,-30.3812851836906));
#30367=CARTESIAN_POINT('Ctrl Pts',(0.664923058647628,3.32411035450556,-30.3707706846519));
#30368=CARTESIAN_POINT('Ctrl Pts',(0.627836088364567,3.33131414360195,-30.3686163806658));
#30369=CARTESIAN_POINT('Ctrl Pts',(0.570385047073269,3.34148005983637,-30.3652405548998));
#30370=CARTESIAN_POINT('Ctrl Pts',(0.550100349700086,3.34487931781875,-30.3640412337996));
#30371=CARTESIAN_POINT('Ctrl Pts',(0.512088254238199,3.35089417237066,-30.3617778965681));
#30372=CARTESIAN_POINT('Ctrl Pts',(0.494369121350027,3.35355412229385,-30.3607162304572));
#30373=CARTESIAN_POINT('Ctrl Pts',(0.451304085638983,3.35967022682391,-30.3581207033446));
#30374=CARTESIAN_POINT('Ctrl Pts',(0.425938912102345,3.36298013188903,-30.3565793125276));
#30375=CARTESIAN_POINT('Ctrl Pts',(0.330901913095462,3.37428911865159,-30.3507629405616));
#30376=CARTESIAN_POINT('Ctrl Pts',(0.261028423953723,3.3804120985929,-30.3464042718121));
#30377=CARTESIAN_POINT('Ctrl Pts',(0.0660205524847508,3.39141874390945,
-30.3340979306516));
#30378=CARTESIAN_POINT('Ctrl Pts',(-0.0592694319147097,3.3915430929957,
-30.3260324125525));
#30379=CARTESIAN_POINT('Ctrl Pts',(-0.411268998308128,3.37237935504958,
-30.3033269244206));
#30380=CARTESIAN_POINT('Ctrl Pts',(-0.636476659751925,3.33721586636319,
-30.288789981977));
#30381=CARTESIAN_POINT('Ctrl Pts',(-0.910985651576816,3.26552942853779,
-30.2714942813932));
#30382=CARTESIAN_POINT('Ctrl Pts',(-0.965119870503428,3.24994176958631,
-30.2681014264206));
#30383=CARTESIAN_POINT('Ctrl Pts',(-1.0514536739844,3.22273475516236,-30.262717071615));
#30384=CARTESIAN_POINT('Ctrl Pts',(-1.08390781583331,3.21196483555598,-30.2606991069521));
#30385=CARTESIAN_POINT('Ctrl Pts',(-1.14611375329735,3.19027151872824,-30.2568414095638));
#30386=CARTESIAN_POINT('Ctrl Pts',(-1.17588607666498,3.17941836390154,-30.254999647956));
#30387=CARTESIAN_POINT('Ctrl Pts',(-1.24554624105348,3.15291219026105,-30.2506989419629));
#30388=CARTESIAN_POINT('Ctrl Pts',(-1.28529859029521,3.13691703502367,-30.2482514322087));
#30389=CARTESIAN_POINT('Ctrl Pts',(-1.42479366301469,3.07769130386727,-30.2396758498533));
#30390=CARTESIAN_POINT('Ctrl Pts',(-1.52275286718551,3.03042033681127,-30.2336800194438));
#30391=CARTESIAN_POINT('Ctrl Pts',(-1.77551187615951,2.8930923073103,-30.2180790358137));
#30392=CARTESIAN_POINT('Ctrl Pts',(-1.92573392557676,2.79534896820772,-30.2086805884349));
#30393=CARTESIAN_POINT('Ctrl Pts',(-2.17867119322614,2.60066597443253,-30.1916745069931));
#30394=CARTESIAN_POINT('Ctrl Pts',(-2.28437775215542,2.50832274690606,-30.184129774781));
#30395=CARTESIAN_POINT('Ctrl Pts',(-2.41065658131156,2.38338844450821,-30.174116233239));
#30396=CARTESIAN_POINT('Ctrl Pts',(-2.43682187083831,2.35662991597437,-30.1719814985218));
#30397=CARTESIAN_POINT('Ctrl Pts',(-2.47662025365248,2.3145576532787,-30.168629911429));
#30398=CARTESIAN_POINT('Ctrl Pts',(-2.490567177018,2.29954345505224,-30.1674347630228));
#30399=CARTESIAN_POINT('Ctrl Pts',(-2.51646534743088,2.27115146695888,-30.1651743722106));
#30400=CARTESIAN_POINT('Ctrl Pts',(-2.52844785787659,2.25780384554049,-30.1641113909861));
#30401=CARTESIAN_POINT('Ctrl Pts',(-2.55735685659966,2.22508265047021,-30.1615056083016));
#30402=CARTESIAN_POINT('Ctrl Pts',(-2.57416956818621,2.20561053675838,-30.1599551237235));
#30403=CARTESIAN_POINT('Ctrl Pts',(-2.63675296855501,2.13143752162013,-30.1540559373522));
#30404=CARTESIAN_POINT('Ctrl Pts',(-2.6810125056473,2.07549094726914,-30.1496205625073));
#30405=CARTESIAN_POINT('Ctrl Pts',(-2.8002212030882,1.91462364107994,-30.1369977695026));
#30406=CARTESIAN_POINT('Ctrl Pts',(-2.87099762910775,1.80676303771441,-30.1286862764339));
#30407=CARTESIAN_POINT('Ctrl Pts',(-3.04556133080121,1.50447259189867,-30.1062040789973));
#30408=CARTESIAN_POINT('Ctrl Pts',(-3.13684151164966,1.303507574418,-30.092139217259));
#30409=CARTESIAN_POINT('Ctrl Pts',(-3.2265181311771,1.04080522694941,-30.0752034532165));
#30410=CARTESIAN_POINT('Ctrl Pts',(-3.24366755888014,0.986060917945988,
-30.0717461698013));
#30411=CARTESIAN_POINT('Ctrl Pts',(-3.268865766985,0.897833295513708,-30.0662860419803));
#30412=CARTESIAN_POINT('Ctrl Pts',(-3.2778075980432,0.864618707316396,-30.0642553663751));
#30413=CARTESIAN_POINT('Ctrl Pts',(-3.29399433744646,0.800628221617553,
-30.0603890394647));
#30414=CARTESIAN_POINT('Ctrl Pts',(-3.30131721612446,0.76987595206582,-30.0585511056436));
#30415=CARTESIAN_POINT('Ctrl Pts',(-3.317438459156,0.697709997797373,-30.0542828012291));
#30416=CARTESIAN_POINT('Ctrl Pts',(-3.32589337531506,0.656224544131117,
-30.0518633469465));
#30417=CARTESIAN_POINT('Ctrl Pts',(-3.34624000959653,0.545863348588604,
-30.0455094883723));
#30418=CARTESIAN_POINT('Ctrl Pts',(-3.35678289001173,0.476758323617263,
-30.0416156751619));
#30419=CARTESIAN_POINT('Ctrl Pts',(-3.38166259622505,0.271235008702921,
-30.0302304108983));
#30420=CARTESIAN_POINT('Ctrl Pts',(-3.38986683334396,0.134219282446046,
-30.0228978926989));
#30421=CARTESIAN_POINT('Ctrl Pts',(-3.38974874325427,-0.00291892207943553,
-30.0156103845689));
#30422=CARTESIAN_POINT('',(-3.38974953533873,0.00177487207047444,-28.7660178032));
#30423=CARTESIAN_POINT('Ctrl Pts',(-3.38974872454211,-0.00294057224222385,
-30.0160178032104));
#30424=CARTESIAN_POINT('Ctrl Pts',(-3.38963484568422,-0.134214583385583,
-30.0083170754981));
#30425=CARTESIAN_POINT('Ctrl Pts',(-3.38189161080866,-0.265159729420946,
-30.0006163477858));
#30426=CARTESIAN_POINT('Ctrl Pts',(-3.36665492089121,-0.395018614927236,
-29.9929156200736));
#30427=CARTESIAN_POINT('Ctrl Pts',(-3.35111993381036,-0.527419820149826,
-29.9850641309266));
#30428=CARTESIAN_POINT('Ctrl Pts',(-3.32779521844705,-0.658692042817637,
-29.9772126417796));
#30429=CARTESIAN_POINT('Ctrl Pts',(-3.29687322499598,-0.788055836095793,
-29.9693611526326));
#30430=CARTESIAN_POINT('Ctrl Pts',(-3.29214449671142,-0.807838720703128,
-29.9681604681145));
#30431=CARTESIAN_POINT('Ctrl Pts',(-3.28723819018725,-0.827577014639484,
-29.9669597835964));
#30432=CARTESIAN_POINT('Ctrl Pts',(-3.28215509176372,-0.847267971842154,
-29.9657590990783));
#30433=CARTESIAN_POINT('Ctrl Pts',(-3.25631504677856,-0.947367394973932,
-29.9596553923673));
#30434=CARTESIAN_POINT('Ctrl Pts',(-3.22584825566311,-1.04645142692693,
-29.9535516856563));
#30435=CARTESIAN_POINT('Ctrl Pts',(-3.19085081991225,-1.14406123418518,
-29.9474479789452));
#30436=CARTESIAN_POINT('Ctrl Pts',(-3.15589918499894,-1.24154330034387,
-29.9413522601017));
#30437=CARTESIAN_POINT('Ctrl Pts',(-3.11642883628647,-1.33755457844917,
-29.9352565412582));
#30438=CARTESIAN_POINT('Ctrl Pts',(-3.07258634988741,-1.43164876453185,
-29.9291608224147));
#30439=CARTESIAN_POINT('Ctrl Pts',(-3.0287887209982,-1.52564667799801,-29.9230713404156));
#30440=CARTESIAN_POINT('Ctrl Pts',(-2.980628029503,-1.61773101454663,-29.9169818584165));
#30441=CARTESIAN_POINT('Ctrl Pts',(-2.9282995880987,-1.70747374352901,-29.9108923764175));
#30442=CARTESIAN_POINT('Ctrl Pts',(-2.87600805259324,-1.7971531792814,-29.9048071891728));
#30443=CARTESIAN_POINT('Ctrl Pts',(-2.81955482721702,-1.88449392346243,
-29.8987220019282));
#30444=CARTESIAN_POINT('Ctrl Pts',(-2.75918158501452,-1.96909167978963,
-29.8926368146836));
#30445=CARTESIAN_POINT('Ctrl Pts',(-2.69883044215406,-2.05365846950506,
-29.8865538548932));
#30446=CARTESIAN_POINT('Ctrl Pts',(-2.6345623823551,-2.13548391940741,-29.8804708951028));
#30447=CARTESIAN_POINT('Ctrl Pts',(-2.56666246662722,-2.21419259435738,
-29.8743879353125));
#30448=CARTESIAN_POINT('Ctrl Pts',(-2.49876984974142,-2.29289280858715,
-29.8683056294045));
#30449=CARTESIAN_POINT('Ctrl Pts',(-2.42724643247243,-2.36847659050669,
-29.8622233234966));
#30450=CARTESIAN_POINT('Ctrl Pts',(-2.3524170444764,-2.44060220260429,-29.8561410175886));
#30451=CARTESIAN_POINT('Ctrl Pts',(-2.27757635327864,-2.51273870949023,
-29.8500577929303));
#30452=CARTESIAN_POINT('Ctrl Pts',(-2.19942900695891,-2.58141571209807,
-29.8439745682719));
#30453=CARTESIAN_POINT('Ctrl Pts',(-2.11833543487584,-2.64632954256445,
-29.8378913436136));
#30454=CARTESIAN_POINT('Ctrl Pts',(-2.03715807415193,-2.71131044421154,
-29.8318018335603));
#30455=CARTESIAN_POINT('Ctrl Pts',(-1.95302874273048,-2.77252014120312,
-29.8257123235071));
#30456=CARTESIAN_POINT('Ctrl Pts',(-1.86633955206104,-2.82969640401804,
-29.8196228134538));
#30457=CARTESIAN_POINT('Ctrl Pts',(-1.77960360175262,-2.88690350737242,
-29.8135300187547));
#30458=CARTESIAN_POINT('Ctrl Pts',(-1.69030540905641,-2.9400726241836,-29.8074372240555));
#30459=CARTESIAN_POINT('Ctrl Pts',(-1.59886284357325,-2.98898689691689,
-29.8013444293564));
#30460=CARTESIAN_POINT('Ctrl Pts',(-1.507272722582,-3.03798009974503,-29.7952418030716));
#30461=CARTESIAN_POINT('Ctrl Pts',(-1.41353170251924,-3.08270455912023,
-29.7891391767867));
#30462=CARTESIAN_POINT('Ctrl Pts',(-1.31807902546371,-3.12299099344405,
-29.7830365505019));
#30463=CARTESIAN_POINT('Ctrl Pts',(-1.24585108273921,-3.15347527487726,
-29.7784187633914));
#30464=CARTESIAN_POINT('Ctrl Pts',(-1.17264352409538,-3.18141943340367,
-29.773800976281));
#30465=CARTESIAN_POINT('Ctrl Pts',(-1.09865184334181,-3.20676927601935,
-29.7691831891705));
#30466=CARTESIAN_POINT('Ctrl Pts',(-1.00084858134843,-3.24027706059163,
-29.7630793321152));
#30467=CARTESIAN_POINT('Ctrl Pts',(-0.9013471461894,-3.26936255109773,-29.75697547506));
#30468=CARTESIAN_POINT('Ctrl Pts',(-0.800583569394607,-3.29385351995431,
-29.7508716180047));
#30469=CARTESIAN_POINT('Ctrl Pts',(-0.699951809905278,-3.3183124501157,
-29.744775745918));
#30470=CARTESIAN_POINT('Ctrl Pts',(-0.59806160317771,-3.338188707894,-29.7386798738313));
#30471=CARTESIAN_POINT('Ctrl Pts',(-0.495366290736147,-3.35335910700037,
-29.7325840017446));
#30472=CARTESIAN_POINT('Ctrl Pts',(-0.392776003753793,-3.36851399149273,
-29.7264943638448));
#30473=CARTESIAN_POINT('Ctrl Pts',(-0.289382668966533,-3.37897252537377,
-29.7204047259449));
#30474=CARTESIAN_POINT('Ctrl Pts',(-0.185651185774396,-3.38466227262345,
-29.714315088045));
#30475=CARTESIAN_POINT('Ctrl Pts',(-0.081992803451167,-3.39034801023734,
-29.7082297415889));
#30476=CARTESIAN_POINT('Ctrl Pts',(0.0220028278789831,-3.3912716208874,
-29.7021443951327));
#30477=CARTESIAN_POINT('Ctrl Pts',(0.125865117903764,-3.387412439399,-29.6960590486766));
#30478=CARTESIAN_POINT('Ctrl Pts',(0.229689424208958,-3.38355466926083,
-29.6899759277066));
#30479=CARTESIAN_POINT('Ctrl Pts',(0.333380059500198,-3.37491759923433,
-29.6838928067367));
#30480=CARTESIAN_POINT('Ctrl Pts',(0.436466658870567,-3.36153267397394,
-29.6778096857667));
#30481=CARTESIAN_POINT('Ctrl Pts',(0.539542207175188,-3.3481491836012,-29.6717272169181));
#30482=CARTESIAN_POINT('Ctrl Pts',(0.642013424516179,-3.33001890519619,
-29.6656447480695));
#30483=CARTESIAN_POINT('Ctrl Pts',(0.743416201023518,-3.30722503234294,
-29.6595622792208));
#30484=CARTESIAN_POINT('Ctrl Pts',(0.844834320244893,-3.28442771067019,
-29.6534788900663));
#30485=CARTESIAN_POINT('Ctrl Pts',(0.945183260445176,-3.2569654863683,-29.6473955009117));
#30486=CARTESIAN_POINT('Ctrl Pts',(1.04401111103125,-3.22497222663131,-29.6413121117571));
#30487=CARTESIAN_POINT('Ctrl Pts',(1.14294109343841,-3.19294590404958,-29.6352224358361));
#30488=CARTESIAN_POINT('Ctrl Pts',(1.24034643965251,-3.15637932680083,-29.629132759915));
#30489=CARTESIAN_POINT('Ctrl Pts',(1.33579240652075,-3.11545561823331,-29.623043083994));
#30490=CARTESIAN_POINT('Ctrl Pts',(1.43128987071761,-3.07450982951157,-29.616950122423));
#30491=CARTESIAN_POINT('Ctrl Pts',(1.52482546507202,-3.02920241301288,-29.610857160852));
#30492=CARTESIAN_POINT('Ctrl Pts',(1.61598815786518,-2.97976296643533,-29.604764199281));
#30493=CARTESIAN_POINT('Ctrl Pts',(1.70729794924743,-2.93024374519762,-29.5986614062096));
#30494=CARTESIAN_POINT('Ctrl Pts',(1.79622682431919,-2.87657939595367,-29.5925586131381));
#30495=CARTESIAN_POINT('Ctrl Pts',(1.882391716187,-2.81904354158118,-29.5864558200667));
#30496=CARTESIAN_POINT('Ctrl Pts',(1.94756722992035,-2.77552316123222,-29.5818396397987));
#30497=CARTESIAN_POINT('Ctrl Pts',(2.01116192165579,-2.72978862040712,-29.5772234595306));
#30498=CARTESIAN_POINT('Ctrl Pts',(2.0730231287862,-2.6819731859244,-29.5726072792626));
#30499=CARTESIAN_POINT('Ctrl Pts',(2.1548036995478,-2.61876113907625,-29.5665046848489));
#30500=CARTESIAN_POINT('Ctrl Pts',(2.23382774027247,-2.55169894592992,-29.5604020904352));
#30501=CARTESIAN_POINT('Ctrl Pts',(2.30971157540194,-2.48105572306514,-29.5542994960215));
#30502=CARTESIAN_POINT('Ctrl Pts',(2.38549607407754,-2.41050497638105,-29.5482048902669));
#30503=CARTESIAN_POINT('Ctrl Pts',(2.4581482291904,-2.3363828085167,-29.5421102845122));
#30504=CARTESIAN_POINT('Ctrl Pts',(2.52731577703097,-2.25899978434491,-29.5360156787576));
#30505=CARTESIAN_POINT('Ctrl Pts',(2.59641255055622,-2.18169594081092,-29.5299273091869));
#30506=CARTESIAN_POINT('Ctrl Pts',(2.66203152358469,-2.10113819305185,-29.5238389396162));
#30507=CARTESIAN_POINT('Ctrl Pts',(2.72385643947098,-2.01767469123555,-29.5177505700455));
#30508=CARTESIAN_POINT('Ctrl Pts',(2.78563779983912,-1.93426998927392,-29.5116664897179));
#30509=CARTESIAN_POINT('Ctrl Pts',(2.84363016461202,-1.8479639466973,-29.5055824093902));
#30510=CARTESIAN_POINT('Ctrl Pts',(2.89755736718324,-1.75913796115658,-29.4994983290626));
#30511=CARTESIAN_POINT('Ctrl Pts',(2.95146485976785,-1.67034444084495,-29.4934164724205));
#30512=CARTESIAN_POINT('Ctrl Pts',(3.0013099214621,-1.57903317318219,-29.4873346157784));
#30513=CARTESIAN_POINT('Ctrl Pts',(3.04686001700828,-1.48561404787929,-29.4812527591363));
#30514=CARTESIAN_POINT('Ctrl Pts',(3.09240525321185,-1.3922048886485,-29.4751715513145));
#30515=CARTESIAN_POINT('Ctrl Pts',(3.13365624704176,-1.2966887032753,-29.4690903434927));
#30516=CARTESIAN_POINT('Ctrl Pts',(3.17042711307225,-1.19949863826367,-29.4630091356709));
#30517=CARTESIAN_POINT('Ctrl Pts',(3.20720357291047,-1.10229378810835,-29.4569270027388));
#30518=CARTESIAN_POINT('Ctrl Pts',(3.23949839956419,-1.00341495234551,-29.4508448698067));
#30519=CARTESIAN_POINT('Ctrl Pts',(3.26717473184124,-0.903312976834777,
-29.4447627368745));
#30520=CARTESIAN_POINT('Ctrl Pts',(3.29487974043413,-0.803107282527913,
-29.4386743020537));
#30521=CARTESIAN_POINT('Ctrl Pts',(3.31795658401251,-0.701676330474625,
-29.4325858672329));
#30522=CARTESIAN_POINT('Ctrl Pts',(3.33631897631765,-0.599483736862607,
-29.4264974324121));
#30523=CARTESIAN_POINT('Ctrl Pts',(3.3546912977617,-0.497235884412761,-29.4204057053779));
#30524=CARTESIAN_POINT('Ctrl Pts',(3.36834403386814,-0.394225993959921,
-29.4143139783436));
#30525=CARTESIAN_POINT('Ctrl Pts',(3.37724275221989,-0.290923452265745,
-29.4082222513093));
#30526=CARTESIAN_POINT('Ctrl Pts',(3.38615586636746,-0.187453794112863,
-29.4021206694561));
#30527=CARTESIAN_POINT('Ctrl Pts',(3.39029958255419,-0.0836909664586204,
-29.3960190876028));
#30528=CARTESIAN_POINT('Ctrl Pts',(3.38969161732259,0.01989477200076,-29.3899175057496));
#30529=CARTESIAN_POINT('Ctrl Pts',(3.38923040970286,0.0984757983311476,
-29.385288793618));
#30530=CARTESIAN_POINT('Ctrl Pts',(3.3860357536877,0.176954896702791,-29.3806600814864));
#30531=CARTESIAN_POINT('Ctrl Pts',(3.38013519819818,0.255129583548729,-29.3760313693548));
#30532=CARTESIAN_POINT('Ctrl Pts',(3.37235303818692,0.358233083371036,-29.369926625739));
#30533=CARTESIAN_POINT('Ctrl Pts',(3.35983614049466,0.461152792640079,-29.3638218821233));
#30534=CARTESIAN_POINT('Ctrl Pts',(3.34259823615956,0.563419997979316,-29.3577171385075));
#30535=CARTESIAN_POINT('Ctrl Pts',(3.32538289832877,0.665553323162041,-29.3516203867404));
#30536=CARTESIAN_POINT('Ctrl Pts',(3.30345891147442,0.767035424854807,-29.3455236349733));
#30537=CARTESIAN_POINT('Ctrl Pts',(3.27689189940138,0.867401027286458,-29.3394268832063));
#30538=CARTESIAN_POINT('Ctrl Pts',(3.2503520877535,0.967663871189969,-29.3333363735502));
#30539=CARTESIAN_POINT('Ctrl Pts',(3.21917881274537,1.06681207813027,-29.3272458638942));
#30540=CARTESIAN_POINT('Ctrl Pts',(3.1834888927682,1.16438976812815,-29.3211553542382));
#30541=CARTESIAN_POINT('Ctrl Pts',(3.14782421015841,1.26189845813911,-29.3150691513565));
#30542=CARTESIAN_POINT('Ctrl Pts',(3.10764938037095,1.35783843961796,-29.3089829484748));
#30543=CARTESIAN_POINT('Ctrl Pts',(3.06313104016448,1.45176902201448,-29.3028967455931));
#30544=CARTESIAN_POINT('Ctrl Pts',(3.01862904948541,1.54566510805234,-29.2968127778922));
#30545=CARTESIAN_POINT('Ctrl Pts',(2.96978690161386,1.63755287605232,-29.2907288101913));
#30546=CARTESIAN_POINT('Ctrl Pts',(2.91681903096719,1.7270123922797,-29.2846448424904));
#30547=CARTESIAN_POINT('Ctrl Pts',(2.86385693047201,1.81646216307168,-29.2785615375576));
#30548=CARTESIAN_POINT('Ctrl Pts',(2.80677021865848,1.90348384050798,-29.2724782326248));
#30549=CARTESIAN_POINT('Ctrl Pts',(2.74581841907227,1.98768364484479,-29.266394927692));
#30550=CARTESIAN_POINT('Ctrl Pts',(2.68485751476335,2.07189602659319,-29.2603107140608));
#30551=CARTESIAN_POINT('Ctrl Pts',(2.62003062617236,2.15328535166928,-29.2542265004296));
#30552=CARTESIAN_POINT('Ctrl Pts',(2.55163903494482,2.23148903153161,-29.2481422867984));
#30553=CARTESIAN_POINT('Ctrl Pts',(2.48317703270879,2.30977322421528,-29.2420518093033));
#30554=CARTESIAN_POINT('Ctrl Pts',(2.41114328059405,2.38486489977891,-29.2359613318082));
#30555=CARTESIAN_POINT('Ctrl Pts',(2.33587755638856,2.45643666803364,-29.2298708543132));
#30556=CARTESIAN_POINT('Ctrl Pts',(2.26057137087792,2.52804691179879,-29.2237771027026));
#30557=CARTESIAN_POINT('Ctrl Pts',(2.18203007520766,2.59613319908747,-29.2176833510921));
#30558=CARTESIAN_POINT('Ctrl Pts',(2.10062681002168,2.66040825203917,-29.2115895994816));
#30559=CARTESIAN_POINT('Ctrl Pts',(2.01909256895207,2.72478672199555,-29.2054860431722));
#30560=CARTESIAN_POINT('Ctrl Pts',(1.93468750697555,2.78534145861058,-29.1993824868629));
#30561=CARTESIAN_POINT('Ctrl Pts',(1.84781419885469,2.84182824058932,-29.1932789305535));
#30562=CARTESIAN_POINT('Ctrl Pts',(1.78222999385105,2.88447241714279,-29.1886711068513));
#30563=CARTESIAN_POINT('Ctrl Pts',(1.71523965533779,2.92479902033357,-29.1840632831491));
#30564=CARTESIAN_POINT('Ctrl Pts',(1.64702482028717,2.96272076035829,-29.179455459447));
#30565=CARTESIAN_POINT('Ctrl Pts',(1.55664606832032,3.01296378349692,-29.1733504918812));
#30566=CARTESIAN_POINT('Ctrl Pts',(1.4638153391217,3.05915135961099,-29.1672455243155));
#30567=CARTESIAN_POINT('Ctrl Pts',(1.3689316745371,3.10103710602583,-29.1611405567498));
#30568=CARTESIAN_POINT('Ctrl Pts',(1.27417189082164,3.14286816607613,-29.1550435598784));
#30569=CARTESIAN_POINT('Ctrl Pts',(1.17736488808481,3.180408391561,-29.148946563007));
#30570=CARTESIAN_POINT('Ctrl Pts',(1.07893537895798,3.21345662963308,-29.1428495661356));
#30571=CARTESIAN_POINT('Ctrl Pts',(0.980606310713293,3.24647114413776,-29.1367587908511));
#30572=CARTESIAN_POINT('Ctrl Pts',(0.880658431361001,3.27500265116174,-29.1306680155666));
#30573=CARTESIAN_POINT('Ctrl Pts',(0.779536764973355,3.29889792120867,-29.1245772402821));
#30574=CARTESIAN_POINT('Ctrl Pts',(0.678486113565275,3.32277641026123,-29.1184907423825));
#30575=CARTESIAN_POINT('Ctrl Pts',(0.576263728945264,3.34202503917259,-29.1124042444828));
#30576=CARTESIAN_POINT('Ctrl Pts',(0.473329354025469,3.35654053828013,-29.1063177465832));
#30577=CARTESIAN_POINT('Ctrl Pts',(0.370432478015325,3.37105074940306,-29.1002334659898));
#30578=CARTESIAN_POINT('Ctrl Pts',(0.2668245497823,3.38083119818105,-29.0941491853964));
#30579=CARTESIAN_POINT('Ctrl Pts',(0.162974268410279,3.38582995000283,-29.088064904803));
#30580=CARTESIAN_POINT('Ctrl Pts',(0.0591350030289799,3.39082817157853,
-29.0819812696039));
#30581=CARTESIAN_POINT('Ctrl Pts',(-0.0449461376778227,3.39104568435428,
-29.0758976344048));
#30582=CARTESIAN_POINT('Ctrl Pts',(-0.148797494856594,3.38648259526376,
-29.0698139992057));
#30583=CARTESIAN_POINT('Ctrl Pts',(-0.252664652339694,3.38191881192911,
-29.0637294384213));
#30584=CARTESIAN_POINT('Ctrl Pts',(-0.356301530027339,3.37257300040057,
-29.0576448776369));
#30585=CARTESIAN_POINT('Ctrl Pts',(-0.459239547455927,3.35849729798201,
-29.0515603168526));
#30586=CARTESIAN_POINT('Ctrl Pts',(-0.562283938322313,3.34440705010306,
-29.0454694684432));
#30587=CARTESIAN_POINT('Ctrl Pts',(-0.664627602662921,3.32557720835593,
-29.0393786200339));
#30588=CARTESIAN_POINT('Ctrl Pts',(-0.76581017663551,3.30211142087324,-29.0332877716245));
#30589=CARTESIAN_POINT('Ctrl Pts',(-0.867047368978681,3.27863296655449,
-29.0271936353742));
#30590=CARTESIAN_POINT('Ctrl Pts',(-0.967121811170322,3.25051369721142,
-29.0210994991238));
#30591=CARTESIAN_POINT('Ctrl Pts',(-1.06558828489369,3.21790718784699,-29.0150053628735));
#30592=CARTESIAN_POINT('Ctrl Pts',(-1.16421347436755,3.18524812083111,-29.0089014036309));
#30593=CARTESIAN_POINT('Ctrl Pts',(-1.26122511869676,3.14808751814462,-29.0027974443883));
#30594=CARTESIAN_POINT('Ctrl Pts',(-1.3561977631002,3.10662722093624,-28.9966934851457));
#30595=CARTESIAN_POINT('Ctrl Pts',(-1.42784229970525,3.07535080655755,-28.9920888399435));
#30596=CARTESIAN_POINT('Ctrl Pts',(-1.4983269104377,3.04162854815276,-28.9874841947413));
#30597=CARTESIAN_POINT('Ctrl Pts',(-1.567479148493,3.00556387081354,-28.9828795495391));
#30598=CARTESIAN_POINT('Ctrl Pts',(-1.65903176983785,2.95781681531374,-28.9767833283541));
#30599=CARTESIAN_POINT('Ctrl Pts',(-1.74855650684832,2.90580153269723,-28.9706871071691));
#30600=CARTESIAN_POINT('Ctrl Pts',(-1.83562875182568,2.84971439761441,-28.964590885984));
#30601=CARTESIAN_POINT('Ctrl Pts',(-1.92258668196672,2.79370089784063,-28.9585026683658));
#30602=CARTESIAN_POINT('Ctrl Pts',(-2.0070981636955,2.73362640301431,-28.9524144507476));
#30603=CARTESIAN_POINT('Ctrl Pts',(-2.0887621366013,2.66973365697794,-28.9463262331293));
#30604=CARTESIAN_POINT('Ctrl Pts',(-2.17034237264281,2.60590642548871,-28.940244258267));
#30605=CARTESIAN_POINT('Ctrl Pts',(-2.24908056991337,2.53826899052723,-28.9341622834047));
#30606=CARTESIAN_POINT('Ctrl Pts',(-2.32460443485265,2.46710747312787,-28.9280803085424));
#30607=CARTESIAN_POINT('Ctrl Pts',(-2.40007523589183,2.39599595459515,-28.9220026069427));
#30608=CARTESIAN_POINT('Ctrl Pts',(-2.47233588434936,2.32136557020203,-28.915924905343));
#30609=CARTESIAN_POINT('Ctrl Pts',(-2.54104764926716,2.24354226763256,-28.9098472037433));
#30610=CARTESIAN_POINT('Ctrl Pts',(-2.60973440863595,2.16574728647804,-28.9037717139376));
#30611=CARTESIAN_POINT('Ctrl Pts',(-2.6748745677829,2.08476201730779,-28.8976962241318));
#30612=CARTESIAN_POINT('Ctrl Pts',(-2.73616729782295,2.00094817044927,-28.891620734326));
#30613=CARTESIAN_POINT('Ctrl Pts',(-2.79745367670782,1.91714300838496,-28.8855458740627));
#30614=CARTESIAN_POINT('Ctrl Pts',(-2.85489316624182,1.83051019738962,-28.8794710137995));
#30615=CARTESIAN_POINT('Ctrl Pts',(-2.90822674487783,1.74144258098776,-28.8733961535362));
#30616=CARTESIAN_POINT('Ctrl Pts',(-2.96156867966017,1.6523610097369,-28.8673203414819));
#30617=CARTESIAN_POINT('Ctrl Pts',(-3.0108032052869,1.56084424291391,-28.8612445294276));
#30618=CARTESIAN_POINT('Ctrl Pts',(-3.05571643314041,1.46731119491935,-28.8551687173734));
#30619=CARTESIAN_POINT('Ctrl Pts',(-3.10067683507646,1.37367990558394,-28.8490865236611));
#30620=CARTESIAN_POINT('Ctrl Pts',(-3.14130668936545,1.27802849296878,-28.8430043299488));
#30621=CARTESIAN_POINT('Ctrl Pts',(-3.17743963820953,1.18079736112294,-28.8369221362365));
#30622=CARTESIAN_POINT('Ctrl Pts',(-3.21359235251758,1.08351304185413,-28.8308366154396));
#30623=CARTESIAN_POINT('Ctrl Pts',(-3.24524313126079,0.984647690411331,
-28.8247510946426));
#30624=CARTESIAN_POINT('Ctrl Pts',(-3.27227564826182,0.884656512038806,
-28.8186655738456));
#30625=CARTESIAN_POINT('Ctrl Pts',(-3.2993524765141,0.784501429793518,-28.8125700777644));
#30626=CARTESIAN_POINT('Ctrl Pts',(-3.32179582826501,0.683217252858073,
-28.8064745816832));
#30627=CARTESIAN_POINT('Ctrl Pts',(-3.33954056054869,0.581269220714567,
-28.800379085602));
#30628=CARTESIAN_POINT('Ctrl Pts',(-3.35319900700356,0.502797947327609,
-28.7956872702785));
#30629=CARTESIAN_POINT('Ctrl Pts',(-3.36407473000155,0.423933574638009,
-28.7909954549549));
#30630=CARTESIAN_POINT('Ctrl Pts',(-3.37215904810011,0.344888992019939,
-28.7863036396313));
#30631=CARTESIAN_POINT('Ctrl Pts',(-3.3838103417463,0.230968234326469,-28.7795416941708));
#30632=CARTESIAN_POINT('Ctrl Pts',(-3.38968948999923,0.116452751436606,
-28.7727797487102));
#30633=CARTESIAN_POINT('Ctrl Pts',(-3.38974953533829,0.00177487291182191,
-28.7660178032496));
#30634=CARTESIAN_POINT('',(2.57323442701465,2.20655152809232,-28.));
#30635=CARTESIAN_POINT('Ctrl Pts',(-3.38974953533873,0.00177487207047244,
-28.7660178032));
#30636=CARTESIAN_POINT('Ctrl Pts',(-3.38980310654502,-0.100538401451488,
-28.75998493283));
#30637=CARTESIAN_POINT('Ctrl Pts',(-3.38522025555718,-0.203029763549593,
-28.75395206246));
#30638=CARTESIAN_POINT('Ctrl Pts',(-3.37597896934322,-0.305239350432197,
-28.7479191920901));
#30639=CARTESIAN_POINT('Ctrl Pts',(-3.36674870944206,-0.407326985148261,
-28.7418935198865));
#30640=CARTESIAN_POINT('Ctrl Pts',(-3.35287109906797,-0.509133079755363,
-28.7358678476829));
#30641=CARTESIAN_POINT('Ctrl Pts',(-3.33437615323607,-0.610197288776856,
-28.7298421754793));
#30642=CARTESIAN_POINT('Ctrl Pts',(-3.31589815767161,-0.711168874365579,
-28.7238220256901));
#30643=CARTESIAN_POINT('Ctrl Pts',(-3.29281131851551,-0.811399497129672,
-28.717801875901));
#30644=CARTESIAN_POINT('Ctrl Pts',(-3.26519740258242,-0.91043450322856,
-28.7117817261118));
#30645=CARTESIAN_POINT('Ctrl Pts',(-3.2375970288672,-1.00942094129262,-28.7057645286811));
#30646=CARTESIAN_POINT('Ctrl Pts',(-3.20547410556064,-1.1072125061738,-28.6997473312505));
#30647=CARTESIAN_POINT('Ctrl Pts',(-3.16896118880233,-1.20336613146812,
-28.6937301338198));
#30648=CARTESIAN_POINT('Ctrl Pts',(-3.13245620321812,-1.29949887069771,
-28.6877142434182));
#30649=CARTESIAN_POINT('Ctrl Pts',(-3.09156327463266,-1.39399396796392,
-28.6816983530165));
#30650=CARTESIAN_POINT('Ctrl Pts',(-3.04646403832871,-1.48642588973348,
-28.6756824626148));
#30651=CARTESIAN_POINT('Ctrl Pts',(-3.00136227726844,-1.57886298604915,
-28.6696662354301));
#30652=CARTESIAN_POINT('Ctrl Pts',(-2.95205393406501,-1.66923628426913,
-28.6636500082454));
#30653=CARTESIAN_POINT('Ctrl Pts',(-2.89876730066561,-1.75714347709337,
-28.6576337810607));
#30654=CARTESIAN_POINT('Ctrl Pts',(-2.84543109922401,-1.84513244253425,
-28.6516119574894));
#30655=CARTESIAN_POINT('Ctrl Pts',(-2.78810944516356,-1.93065034629345,
-28.6455901339181));
#30656=CARTESIAN_POINT('Ctrl Pts',(-2.72707469177338,-2.01332279776223,
-28.6395683103468));
#30657=CARTESIAN_POINT('Ctrl Pts',(-2.66601051922395,-2.09603509790542,
-28.6335435842162));
#30658=CARTESIAN_POINT('Ctrl Pts',(-2.60122996006742,-2.17589887487336,
-28.6275188580857));
#30659=CARTESIAN_POINT('Ctrl Pts',(-2.53304517815146,-2.25257345894504,
-28.6214941319551));
#30660=CARTESIAN_POINT('Ctrl Pts',(-2.46475386927682,-2.32936783382664,
-28.6154599932293));
#30661=CARTESIAN_POINT('Ctrl Pts',(-2.39304802168692,-2.40296275122096,
-28.6094258545036));
#30662=CARTESIAN_POINT('Ctrl Pts',(-2.31827612471118,-2.47305496746314,
-28.6033917157778));
#30663=CARTESIAN_POINT('Ctrl Pts',(-2.26183713073789,-2.52596166543485,
-28.5988370537597));
#30664=CARTESIAN_POINT('Ctrl Pts',(-2.20365202008319,-2.57687349208777,
-28.5942823917416));
#30665=CARTESIAN_POINT('Ctrl Pts',(-2.14388196705614,-2.62567613650875,
-28.5897277297235));
#30666=CARTESIAN_POINT('Ctrl Pts',(-2.06370305261451,-2.6911427515339,-28.5836178496453));
#30667=CARTESIAN_POINT('Ctrl Pts',(-1.98039165559376,-2.75304047990566,
-28.5775079695672));
#30668=CARTESIAN_POINT('Ctrl Pts',(-1.89429830396667,-2.81105656259155,
-28.571398089489));
#30669=CARTESIAN_POINT('Ctrl Pts',(-1.8083158140953,-2.86899793840791,-28.5652960770571));
#30670=CARTESIAN_POINT('Ctrl Pts',(-1.71955884270337,-2.92306737006823,
-28.5591940646251));
#30671=CARTESIAN_POINT('Ctrl Pts',(-1.62841107528683,-2.97299216823442,
-28.5530920521932));
#30672=CARTESIAN_POINT('Ctrl Pts',(-1.53735482696757,-3.02286683821218,
-28.5469961666329));
#30673=CARTESIAN_POINT('Ctrl Pts',(-1.44391292853432,-3.0686049468868,-28.5409002810726));
#30674=CARTESIAN_POINT('Ctrl Pts',(-1.34849742419764,-3.10997745320321,
-28.5348043955122));
#30675=CARTESIAN_POINT('Ctrl Pts',(-1.2531470092126,-3.15132173654233,-28.5287126683667));
#30676=CARTESIAN_POINT('Ctrl Pts',(-1.1558260557273,-3.18830617072937,-28.5226209412211));
#30677=CARTESIAN_POINT('Ctrl Pts',(-1.05696983234893,-3.2207483347825,-28.5165292140755));
#30678=CARTESIAN_POINT('Ctrl Pts',(-0.95814844390792,-3.25317906687199,
-28.5104396335316));
#30679=CARTESIAN_POINT('Ctrl Pts',(-0.857793265508878,-3.28107057744885,
-28.5043500529876));
#30680=CARTESIAN_POINT('Ctrl Pts',(-0.756357358928734,-3.30428942559431,
-28.4982604724437));
#30681=CARTESIAN_POINT('Ctrl Pts',(-0.654931144185521,-3.32750605526213,
-28.4921714737374));
#30682=CARTESIAN_POINT('Ctrl Pts',(-0.552424822165616,-3.3460508153024,
-28.486082475031));
#30683=CARTESIAN_POINT('Ctrl Pts',(-0.449303478872774,-3.35984098528083,
-28.4799934763247));
#30684=CARTESIAN_POINT('Ctrl Pts',(-0.346165504000262,-3.37363337936052,
-28.4739034955746));
#30685=CARTESIAN_POINT('Ctrl Pts',(-0.242412733307144,-3.38266960316241,
-28.4678135148245));
#30686=CARTESIAN_POINT('Ctrl Pts',(-0.138516342137413,-3.38691870074569,
-28.4617235340745));
#30687=CARTESIAN_POINT('Ctrl Pts',(-0.0345117887296656,-3.39117222188882,
-28.4556272132972));
#30688=CARTESIAN_POINT('Ctrl Pts',(0.0696362570227238,-3.39062864685194,
-28.4495308925199));
#30689=CARTESIAN_POINT('Ctrl Pts',(0.173455666763486,-3.38530917261151,
-28.4434345717426));
#30690=CARTESIAN_POINT('Ctrl Pts',(0.277331697530255,-3.37998679723642,
-28.4373349261541));
#30691=CARTESIAN_POINT('Ctrl Pts',(0.380878310944875,-3.36988337545165,
-28.4312352805656));
#30692=CARTESIAN_POINT('Ctrl Pts',(0.48362951546565,-3.35507191491784,-28.4251356349771));
#30693=CARTESIAN_POINT('Ctrl Pts',(0.586546240260744,-3.34023659483881,
-28.419026163567));
#30694=CARTESIAN_POINT('Ctrl Pts',(0.688664577673534,-3.32067816601063,
-28.4129166921568));
#30695=CARTESIAN_POINT('Ctrl Pts',(0.789529504308436,-3.29652062398015,
-28.4068072207467));
#30696=CARTESIAN_POINT('Ctrl Pts',(0.864677904805932,-3.27852228992977,
-28.4022554204363));
#30697=CARTESIAN_POINT('Ctrl Pts',(0.939130799015132,-3.25797212364141,
-28.397703620126));
#30698=CARTESIAN_POINT('Ctrl Pts',(1.01270679071419,-3.23493895128507,-28.3931518198157));
#30699=CARTESIAN_POINT('Ctrl Pts',(1.11040033392321,-3.20435571119722,-28.3871079801062));
#30700=CARTESIAN_POINT('Ctrl Pts',(1.20688947698545,-3.16928585797825,-28.3810641403967));
#30701=CARTESIAN_POINT('Ctrl Pts',(1.30172715649947,-3.12984208428026,-28.3750203006872));
#30702=CARTESIAN_POINT('Ctrl Pts',(1.39643905301889,-3.09045062476793,-28.3689844769083));
#30703=CARTESIAN_POINT('Ctrl Pts',(1.48950343902635,-3.04669693812566,-28.3629486531294));
#30704=CARTESIAN_POINT('Ctrl Pts',(1.58048776448782,-2.99874365173222,-28.3569128293505));
#30705=CARTESIAN_POINT('Ctrl Pts',(1.67137870739474,-2.95083958261175,-28.3508832004919));
#30706=CARTESIAN_POINT('Ctrl Pts',(1.76019344897887,-2.89874468315972,-28.3448535716333));
#30707=CARTESIAN_POINT('Ctrl Pts',(1.84651973715302,-2.84266950643305,-28.3388239427747));
#30708=CARTESIAN_POINT('Ctrl Pts',(1.93278872440559,-2.78663155080522,-28.3327983162113));
#30709=CARTESIAN_POINT('Ctrl Pts',(2.01657217530537,-2.7266188048023,-28.3267726896479));
#30710=CARTESIAN_POINT('Ctrl Pts',(2.09748356663111,-2.66288710804879,-28.3207470630846));
#30711=CARTESIAN_POINT('Ctrl Pts',(2.17836758470594,-2.59917697245864,-28.3147234750597));
#30712=CARTESIAN_POINT('Ctrl Pts',(2.25638113037952,-2.53175065501087,-28.3086998870348));
#30713=CARTESIAN_POINT('Ctrl Pts',(2.33116853732715,-2.4609059943598,-28.3026762990099));
#30714=CARTESIAN_POINT('Ctrl Pts',(2.40595093707213,-2.39006607693472,-28.2966531142793));
#30715=CARTESIAN_POINT('Ctrl Pts',(2.47750731023465,-2.3158085714327,-28.2906299295486));
#30716=CARTESIAN_POINT('Ctrl Pts',(2.54551760259735,-2.2384693871856,-28.2846067448179));
#30717=CARTESIAN_POINT('Ctrl Pts',(2.61354179761439,-2.16111439327339,-28.2785823288286));
#30718=CARTESIAN_POINT('Ctrl Pts',(2.67801818359024,-2.08067679727522,-28.2725579128393));
#30719=CARTESIAN_POINT('Ctrl Pts',(2.73866656138667,-1.99752610196776,-28.2665334968501));
#30720=CARTESIAN_POINT('Ctrl Pts',(2.79938665850301,-1.91427707738036,-28.2605019567293));
#30721=CARTESIAN_POINT('Ctrl Pts',(2.85626945081757,-1.8283089007561,-28.2544704166086));
#30722=CARTESIAN_POINT('Ctrl Pts',(2.90907777540975,-1.74002056284317,-28.2484388764879));
#30723=CARTESIAN_POINT('Ctrl Pts',(2.96191806166619,-1.65167878937371,-28.242403685843));
#30724=CARTESIAN_POINT('Ctrl Pts',(3.01067876566425,-1.56101444423797,-28.2363684951982));
#30725=CARTESIAN_POINT('Ctrl Pts',(3.05516949359125,-1.46844966816347,-28.2303333045534));
#30726=CARTESIAN_POINT('Ctrl Pts',(3.09974159863611,-1.37571558367249,-28.2242870750598));
#30727=CARTESIAN_POINT('Ctrl Pts',(3.14002795762882,-1.28107452736866,-28.2182408455661));
#30728=CARTESIAN_POINT('Ctrl Pts',(3.175886884025,-1.18496732544741,-28.2121946160724));
#30729=CARTESIAN_POINT('Ctrl Pts',(3.20676398053332,-1.10221216105455,-28.2069883806842));
#30730=CARTESIAN_POINT('Ctrl Pts',(3.23435916229513,-1.01837035387577,-28.201782145296));
#30731=CARTESIAN_POINT('Ctrl Pts',(3.25861234957539,-0.933729413531954,
-28.1965759099078));
#30732=CARTESIAN_POINT('Ctrl Pts',(3.28780567586033,-0.83184793461674,-28.190309214869));
#30733=CARTESIAN_POINT('Ctrl Pts',(3.31225712048596,-0.728455522703703,
-28.1840425198302));
#30734=CARTESIAN_POINT('Ctrl Pts',(3.33181715661598,-0.624018827744321,
-28.1777758247914));
#30735=CARTESIAN_POINT('Ctrl Pts',(3.35134888363776,-0.519733283308555,
-28.171518199498));
#30736=CARTESIAN_POINT('Ctrl Pts',(3.36600321919982,-0.414406853895198,
-28.1652605742047));
#30737=CARTESIAN_POINT('Ctrl Pts',(3.37568072894995,-0.308520143095911,
-28.1590029489113));
#30738=CARTESIAN_POINT('Ctrl Pts',(3.38534642513137,-0.202762690749069,
-28.1527529624515));
#30739=CARTESIAN_POINT('Ctrl Pts',(3.39004735322447,-0.0964467143875391,
-28.1465029759917));
#30740=CARTESIAN_POINT('Ctrl Pts',(3.38973542977069,0.00993874525860727,
-28.1402529895319));
#30741=CARTESIAN_POINT('Ctrl Pts',(3.38942386891304,0.116200536886331,-28.134010268383));
#30742=CARTESIAN_POINT('Ctrl Pts',(3.38411106704277,0.222531252864325,-28.1277675472341));
#30743=CARTESIAN_POINT('Ctrl Pts',(3.37380092760016,0.328439284228145,-28.1215248260852));
#30744=CARTESIAN_POINT('Ctrl Pts',(3.36349780134744,0.434275274555289,-28.1152863513764));
#30745=CARTESIAN_POINT('Ctrl Pts',(3.34820414192129,0.539688756021538,-28.1090478766675));
#30746=CARTESIAN_POINT('Ctrl Pts',(3.32797584730017,0.644190827540035,-28.1028094019586));
#30747=CARTESIAN_POINT('Ctrl Pts',(3.30775716445643,0.748643243332921,-28.0965738915545));
#30748=CARTESIAN_POINT('Ctrl Pts',(3.28260859040427,0.852184719762061,-28.0903383811504));
#30749=CARTESIAN_POINT('Ctrl Pts',(3.25263743906703,0.954334717213748,-28.0841028707463));
#30750=CARTESIAN_POINT('Ctrl Pts',(3.2226743873289,1.05645710898496,-28.0778690454672));
#30751=CARTESIAN_POINT('Ctrl Pts',(3.18789146676026,1.15718838780062,-28.071635220188));
#30752=CARTESIAN_POINT('Ctrl Pts',(3.14844620259218,1.25606192995524,-28.0654013949088));
#30753=CARTESIAN_POINT('Ctrl Pts',(3.10899302898307,1.35495529792337,-28.0591663196425));
#30754=CARTESIAN_POINT('Ctrl Pts',(3.0648757872674,1.45198981188523,-28.0529312443762));
#30755=CARTESIAN_POINT('Ctrl Pts',(3.01630056916356,1.54671779551526,-28.0466961691099));
#30756=CARTESIAN_POINT('Ctrl Pts',(2.96772117818811,1.64145391678686,-28.0404605582172));
#30757=CARTESIAN_POINT('Ctrl Pts',(2.91468323604366,1.73388276038755,-28.0342249473245));
#30758=CARTESIAN_POINT('Ctrl Pts',(2.85743883369826,1.82358119483974,-28.0279893364318));
#30759=CARTESIAN_POINT('Ctrl Pts',(2.80015690628584,1.91333842874876,-28.0217496379478));
#30760=CARTESIAN_POINT('Ctrl Pts',(2.73866323120876,2.00036134475808,-28.0155099394639));
#30761=CARTESIAN_POINT('Ctrl Pts',(2.67325324860397,2.08425577397025,-28.00927024098));
#30762=CARTESIAN_POINT('Ctrl Pts',(2.64086032113565,2.12580273748017,-28.0061801606533));
#30763=CARTESIAN_POINT('Ctrl Pts',(2.60750755147691,2.16658292429367,-28.0030900803267));
#30764=CARTESIAN_POINT('Ctrl Pts',(2.57323442701465,2.20655152809233,-28.));
#30765=CARTESIAN_POINT('',(-2.57363857939818,2.20608012663486,-28.0000033383279));
#30766=CARTESIAN_POINT('Origin',(0.,0.,-28.));
#30767=CARTESIAN_POINT('',(-3.38974897692414,0.00263361762172135,-29.1089821967504));
#30768=CARTESIAN_POINT('Ctrl Pts',(-2.57363857939818,2.20608012663486,-28.0000033383279));
#30769=CARTESIAN_POINT('Ctrl Pts',(-2.50673445663565,2.28413124970314,-28.0060715002323));
#30770=CARTESIAN_POINT('Ctrl Pts',(-2.43615914058954,2.35927292180629,-28.0121396621368));
#30771=CARTESIAN_POINT('Ctrl Pts',(-2.36219674153845,2.43113792631457,-28.0182078240412));
#30772=CARTESIAN_POINT('Ctrl Pts',(-2.28833018792174,2.50290980333291,-28.0242681224147));
#30773=CARTESIAN_POINT('Ctrl Pts',(-2.21108558311393,2.57141315314271,-28.0303284207882));
#30774=CARTESIAN_POINT('Ctrl Pts',(-2.13078697233906,2.63631408239044,-28.0363887191617));
#30775=CARTESIAN_POINT('Ctrl Pts',(-2.04690586672721,2.70411054422213,-28.0427193956579));
#30776=CARTESIAN_POINT('Ctrl Pts',(-1.95969221025354,2.76797529752797,-28.049050072154));
#30777=CARTESIAN_POINT('Ctrl Pts',(-1.86955832191721,2.82757082023601,-28.0553807486502));
#30778=CARTESIAN_POINT('Ctrl Pts',(-1.78341967391273,2.88452473455106,-28.0614308139963));
#30779=CARTESIAN_POINT('Ctrl Pts',(-1.69461455007407,2.9375795375758,-28.0674808793424));
#30780=CARTESIAN_POINT('Ctrl Pts',(-1.60353534230482,2.98648279226239,-28.0735309446885));
#30781=CARTESIAN_POINT('Ctrl Pts',(-1.51248509611952,3.03537049657529,-28.0795790862203));
#30782=CARTESIAN_POINT('Ctrl Pts',(-1.41916258411661,3.0801090712017,-28.0856272277522));
#30783=CARTESIAN_POINT('Ctrl Pts',(-1.32398618142917,3.12049125201219,-28.0916753692841));
#30784=CARTESIAN_POINT('Ctrl Pts',(-1.22881467326578,3.16087135613613,-28.0977231997853));
#30785=CARTESIAN_POINT('Ctrl Pts',(-1.13178986282324,3.19689534332487,-28.1037710302866));
#30786=CARTESIAN_POINT('Ctrl Pts',(-1.03335064130715,3.22840386485491,-28.1098188607879));
#30787=CARTESIAN_POINT('Ctrl Pts',(-0.934890242212077,3.25991916492497,
-28.1158679923804));
#30788=CARTESIAN_POINT('Ctrl Pts',(-0.83501524001308,3.28691693803133,-28.1219171239729));
#30789=CARTESIAN_POINT('Ctrl Pts',(-0.734179284391769,3.30928781475259,
-28.1279662555654));
#30790=CARTESIAN_POINT('Ctrl Pts',(-0.633238313295393,3.33168198959438,
-28.1340216870181));
#30791=CARTESIAN_POINT('Ctrl Pts',(-0.531334814649758,3.34943955747195,
-28.1400771184709));
#30792=CARTESIAN_POINT('Ctrl Pts',(-0.428932011686522,3.36250240027432,
-28.1461325499236));
#30793=CARTESIAN_POINT('Ctrl Pts',(-0.326466514805168,3.37557324052181,
-28.1521916886843));
#30794=CARTESIAN_POINT('Ctrl Pts',(-0.223501535989294,3.38394359936853,
-28.158250827445));
#30795=CARTESIAN_POINT('Ctrl Pts',(-0.120502826735627,3.38760743464303,
-28.1643099662056));
#30796=CARTESIAN_POINT('Ctrl Pts',(-0.0173532184998645,3.39127663764512,
-28.1703779819501));
#30797=CARTESIAN_POINT('Ctrl Pts',(0.0858297871031276,3.39022556151545,
-28.1764459976945));
#30798=CARTESIAN_POINT('Ctrl Pts',(0.188583218928551,3.38450017462528,-28.182514013439));
#30799=CARTESIAN_POINT('Ctrl Pts',(0.221383298329125,3.38267256515997,-28.1844509939825));
#30800=CARTESIAN_POINT('Ctrl Pts',(0.254139669302539,3.380369055138,-28.186387974526));
#30801=CARTESIAN_POINT('Ctrl Pts',(0.286837486178399,3.37759223693785,-28.1883249550694));
#30802=CARTESIAN_POINT('Ctrl Pts',(0.390033927538939,3.36882841770038,-28.1944381919204));
#30803=CARTESIAN_POINT('Ctrl Pts',(0.492994991660657,3.35531667111484,-28.2005514287714));
#30804=CARTESIAN_POINT('Ctrl Pts',(0.595250891976339,3.33707678037251,-28.2066646656224));
#30805=CARTESIAN_POINT('Ctrl Pts',(0.697376283909894,3.31886016905586,-28.2127701001984));
#30806=CARTESIAN_POINT('Ctrl Pts',(0.798797885574264,3.29592748602308,-28.2188755347744));
#30807=CARTESIAN_POINT('Ctrl Pts',(0.899050041752592,3.26835036140936,-28.2249809693504));
#30808=CARTESIAN_POINT('Ctrl Pts',(0.999202596477312,3.24080063492652,-28.2310803381202));
#30809=CARTESIAN_POINT('Ctrl Pts',(1.0981876078073,3.20861575589782,-28.2371797068899));
#30810=CARTESIAN_POINT('Ctrl Pts',(1.19554948127657,3.17191842586144,-28.2432790756596));
#30811=CARTESIAN_POINT('Ctrl Pts',(1.29284624534107,3.1352456366564,-28.2493743655609));
#30812=CARTESIAN_POINT('Ctrl Pts',(1.38852163272792,3.09406654720112,-28.2554696554622));
#30813=CARTESIAN_POINT('Ctrl Pts',(1.4821358524182,3.04855348935796,-28.2615649453636));
#30814=CARTESIAN_POINT('Ctrl Pts',(1.57571783758205,3.00305610319236,-28.2676581364514));
#30815=CARTESIAN_POINT('Ctrl Pts',(1.66723968318424,2.95322790092455,-28.2737513275393));
#30816=CARTESIAN_POINT('Ctrl Pts',(1.75628294273086,2.89928875546618,-28.2798445186272));
#30817=CARTESIAN_POINT('Ctrl Pts',(1.8453183444163,2.84535437001233,-28.2859371720051));
#30818=CARTESIAN_POINT('Ctrl Pts',(1.93187523087929,2.78730998353031,-28.292029825383));
#30819=CARTESIAN_POINT('Ctrl Pts',(2.01556184633548,2.72542024394344,-28.2981224787608));
#30820=CARTESIAN_POINT('Ctrl Pts',(2.0992625071243,2.66352011724778,-28.3042161546839));
#30821=CARTESIAN_POINT('Ctrl Pts',(2.18009159727073,2.59777360818453,-28.3103098306069));
#30822=CARTESIAN_POINT('Ctrl Pts',(2.25768903275896,2.52848675967661,-28.31640350653));
#30823=CARTESIAN_POINT('Ctrl Pts',(2.33536774186066,2.4591273418562,-28.3225035648168));
#30824=CARTESIAN_POINT('Ctrl Pts',(2.40980771871058,2.38622046367609,-28.3286036231036));
#30825=CARTESIAN_POINT('Ctrl Pts',(2.48068450226313,2.31011027068656,-28.3347036813904));
#30826=CARTESIAN_POINT('Ctrl Pts',(2.5516002534467,2.23395823276884,-28.3408070934527));
#30827=CARTESIAN_POINT('Ctrl Pts',(2.6189486333138,2.15459969637648,-28.3469105055151));
#30828=CARTESIAN_POINT('Ctrl Pts',(2.68244565252103,2.07241173123756,-28.3530139175774));
#30829=CARTESIAN_POINT('Ctrl Pts',(2.74604501148576,1.99009130166916,-28.3591271666639));
#30830=CARTESIAN_POINT('Ctrl Pts',(2.80578036520327,1.90493268242848,-28.3652404157503));
#30831=CARTESIAN_POINT('Ctrl Pts',(2.86141108945429,1.8173419159993,-28.3713536648368));
#30832=CARTESIAN_POINT('Ctrl Pts',(2.90250437960307,1.75264038950135,-28.3758693982169));
#30833=CARTESIAN_POINT('Ctrl Pts',(2.94135890813768,1.68661236036022,-28.380385131597));
#30834=CARTESIAN_POINT('Ctrl Pts',(2.97789427619774,1.61942914086685,-28.3849008649772));
#30835=CARTESIAN_POINT('Ctrl Pts',(3.0272200738309,1.52872618466213,-28.3909974821102));
#30836=CARTESIAN_POINT('Ctrl Pts',(3.07248261068612,1.4356120533336,-28.3970940992431));
#30837=CARTESIAN_POINT('Ctrl Pts',(3.1134388129218,1.34048641197592,-28.4031907163761));
#30838=CARTESIAN_POINT('Ctrl Pts',(3.15434073453724,1.24548684380211,-28.4092792534591));
#30839=CARTESIAN_POINT('Ctrl Pts',(3.19094749939381,1.14848145556161,-28.4153677905421));
#30840=CARTESIAN_POINT('Ctrl Pts',(3.22306142240295,1.04989529474032,-28.4214563276251));
#30841=CARTESIAN_POINT('Ctrl Pts',(3.25514201628678,0.951411450615359,-28.4275385457787));
#30842=CARTESIAN_POINT('Ctrl Pts',(3.28273890800558,0.851350501379768,-28.4336207639322));
#30843=CARTESIAN_POINT('Ctrl Pts',(3.30570246866219,0.750157484252925,-28.4397029820857));
#30844=CARTESIAN_POINT('Ctrl Pts',(3.32864946020359,0.649037481881261,-28.4457808116788));
#30845=CARTESIAN_POINT('Ctrl Pts',(3.34696967410669,0.546787452627108,-28.4518586412719));
#30846=CARTESIAN_POINT('Ctrl Pts',(3.36056354374999,0.443866794115685,-28.4579364708651));
#30847=CARTESIAN_POINT('Ctrl Pts',(3.37415230825051,0.340984787192796,-28.4640120179449));
#30848=CARTESIAN_POINT('Ctrl Pts',(3.38301819993575,0.237433075937281,-28.4700875650247));
#30849=CARTESIAN_POINT('Ctrl Pts',(3.38711305058994,0.133679635783901,-28.4761631121046));
#30850=CARTESIAN_POINT('Ctrl Pts',(3.39120742930755,0.029938153342284,-28.4822379589701));
#30851=CARTESIAN_POINT('Ctrl Pts',(3.39053184347868,-0.0740045835416433,
-28.4883128058357));
#30852=CARTESIAN_POINT('Ctrl Pts',(3.385090187282,-0.177678041600797,-28.4943876527012));
#30853=CARTESIAN_POINT('Ctrl Pts',(3.37964774181468,-0.281366536702726,
-28.5004633806769));
#30854=CARTESIAN_POINT('Ctrl Pts',(3.36943787517377,-0.384785247373206,
-28.5065391086526));
#30855=CARTESIAN_POINT('Ctrl Pts',(3.35451648540345,-0.487467139052987,
-28.5126148366283));
#30856=CARTESIAN_POINT('Ctrl Pts',(3.33957969096815,-0.590255038293975,
-28.5186968371131));
#30857=CARTESIAN_POINT('Ctrl Pts',(3.31992172138404,-0.692304174517732,
-28.5247788375979));
#30858=CARTESIAN_POINT('Ctrl Pts',(3.29564991575129,-0.793156160732879,
-28.5308608380827));
#30859=CARTESIAN_POINT('Ctrl Pts',(3.27136507514973,-0.894062308657929,
-28.5369461048547));
#30860=CARTESIAN_POINT('Ctrl Pts',(3.24246158248668,-0.993769614335579,
-28.5430313716267));
#30861=CARTESIAN_POINT('Ctrl Pts',(3.20909657001154,-1.09183527459054,-28.5491166383986));
#30862=CARTESIAN_POINT('Ctrl Pts',(3.17567739682191,-1.19006012274419,-28.5552117832546));
#30863=CARTESIAN_POINT('Ctrl Pts',(3.13778239326417,-1.28663760299493,-28.5613069281106));
#30864=CARTESIAN_POINT('Ctrl Pts',(3.09561678262821,-1.38114510374927,-28.5674020729665));
#30865=CARTESIAN_POINT('Ctrl Pts',(3.06316098297479,-1.45388960961474,-28.5720936402727));
#30866=CARTESIAN_POINT('Ctrl Pts',(3.02817595905214,-1.52540811904442,-28.5767852075789));
#30867=CARTESIAN_POINT('Ctrl Pts',(2.99077316820085,-1.59551901238119,-28.581476774885));
#30868=CARTESIAN_POINT('Ctrl Pts',(2.94210189656725,-1.68675248069739,-28.5875817884829));
#30869=CARTESIAN_POINT('Ctrl Pts',(2.88917087800472,-1.77590930521859,-28.5936868020808));
#30870=CARTESIAN_POINT('Ctrl Pts',(2.83218164326374,-1.8625660262283,-28.5997918156787));
#30871=CARTESIAN_POINT('Ctrl Pts',(2.77526691130241,-1.94910945976154,-28.6058888481116));
#30872=CARTESIAN_POINT('Ctrl Pts',(2.71430474357666,-2.03315893378495,-28.6119858805445));
#30873=CARTESIAN_POINT('Ctrl Pts',(2.64954277448203,-2.11431505426463,-28.6180829129774));
#30874=CARTESIAN_POINT('Ctrl Pts',(2.5848470010219,-2.19538822203358,-28.6241737134051));
#30875=CARTESIAN_POINT('Ctrl Pts',(2.51635941472635,-2.2735735851106,-28.6302645138328));
#30876=CARTESIAN_POINT('Ctrl Pts',(2.4443707131458,-2.34850098556826,-28.6363553142605));
#30877=CARTESIAN_POINT('Ctrl Pts',(2.37243275292753,-2.4233755733166,-28.6424418215769));
#30878=CARTESIAN_POINT('Ctrl Pts',(2.29699888006311,-2.49499645796672,-28.6485283288932));
#30879=CARTESIAN_POINT('Ctrl Pts',(2.21839926144782,-2.5630274636273,-28.6546148362095));
#30880=CARTESIAN_POINT('Ctrl Pts',(2.13982840118596,-2.63103357782224,-28.6606991165694));
#30881=CARTESIAN_POINT('Ctrl Pts',(2.05809441998022,-2.69545214433512,-28.6667833969293));
#30882=CARTESIAN_POINT('Ctrl Pts',(1.97356286039723,-2.75598525006225,-28.6728676772892));
#30883=CARTESIAN_POINT('Ctrl Pts',(1.88904040141231,-2.81651183884509,-28.6789513026205));
#30884=CARTESIAN_POINT('Ctrl Pts',(1.80172131031927,-2.87315354999893,-28.6850349279518));
#30885=CARTESIAN_POINT('Ctrl Pts',(1.7120018516603,-2.92565458016009,-28.691118553283));
#30886=CARTESIAN_POINT('Ctrl Pts',(1.62226888471389,-2.97816351494993,-28.6972030945735));
#30887=CARTESIAN_POINT('Ctrl Pts',(1.53013520090068,-3.02653031436172,-28.7032876358639));
#30888=CARTESIAN_POINT('Ctrl Pts',(1.43602270857422,-3.07054455153465,-28.7093721771543));
#30889=CARTESIAN_POINT('Ctrl Pts',(1.34181319140568,-3.11460416498342,-28.7154629912747));
#30890=CARTESIAN_POINT('Ctrl Pts',(1.24562117938076,-3.15430207369077,-28.721553805395));
#30891=CARTESIAN_POINT('Ctrl Pts',(1.14788962550167,-3.18947557917687,-28.7276446195154));
#30892=CARTESIAN_POINT('Ctrl Pts',(1.05010544842518,-3.22466802370823,-28.7337387132123));
#30893=CARTESIAN_POINT('Ctrl Pts',(0.95078048645369,-3.25533108624429,-28.7398328069092));
#30894=CARTESIAN_POINT('Ctrl Pts',(0.85037205886202,-3.28135222492295,-28.7459269006062));
#30895=CARTESIAN_POINT('Ctrl Pts',(0.749801999855192,-3.30741525085718,
-28.7520308042066));
#30896=CARTESIAN_POINT('Ctrl Pts',(0.648145409439338,-3.3288213380325,-28.7581347078071));
#30897=CARTESIAN_POINT('Ctrl Pts',(0.545869191877263,-3.34550921204221,
-28.7642386114075));
#30898=CARTESIAN_POINT('Ctrl Pts',(0.46871358417293,-3.35809828789193,-28.768843302536));
#30899=CARTESIAN_POINT('Ctrl Pts',(0.391205542683911,-3.36800331474502,
-28.7734479936644));
#30900=CARTESIAN_POINT('Ctrl Pts',(0.313546054131859,-3.37521761290118,
-28.7780526847929));
#30901=CARTESIAN_POINT('Ctrl Pts',(0.210589936480036,-3.38478188049539,
-28.7841572977695));
#30902=CARTESIAN_POINT('Ctrl Pts',(0.107023913160425,-3.3896470357455,-28.7902619107461));
#30903=CARTESIAN_POINT('Ctrl Pts',(0.00331242799393805,-3.38974838156474,
-28.7963665237228));
#30904=CARTESIAN_POINT('Ctrl Pts',(-0.100263724207063,-3.38984959513797,
-28.8024631707988));
#30905=CARTESIAN_POINT('Ctrl Pts',(-0.203984537165262,-3.38519935749678,
-28.8085598178749));
#30906=CARTESIAN_POINT('Ctrl Pts',(-0.307380297863563,-3.37578471099466,
-28.814656464951));
#30907=CARTESIAN_POINT('Ctrl Pts',(-0.410670634049429,-3.36637966386596,
-28.8207468957563));
#30908=CARTESIAN_POINT('Ctrl Pts',(-0.513636153762811,-3.35221990668589,
-28.8268373265616));
#30909=CARTESIAN_POINT('Ctrl Pts',(-0.615807865942744,-3.33334452685933,
-28.8329277573669));
#30910=CARTESIAN_POINT('Ctrl Pts',(-0.717907984141793,-3.31448237342933,
-28.8390139204724));
#30911=CARTESIAN_POINT('Ctrl Pts',(-0.819214982005358,-3.29091124581986,
-28.845100083578));
#30912=CARTESIAN_POINT('Ctrl Pts',(-0.919266529428289,-3.26272188676462,
-28.8511862466836));
#30913=CARTESIAN_POINT('Ctrl Pts',(-1.01928172655826,-3.23454276934468,
-28.8572701985909));
#30914=CARTESIAN_POINT('Ctrl Pts',(-1.11804196899672,-3.20174887103431,
-28.8633541504982));
#30915=CARTESIAN_POINT('Ctrl Pts',(-1.21509741758321,-3.1644815259822,-28.8694381024054));
#30916=CARTESIAN_POINT('Ctrl Pts',(-1.31214267549895,-3.1272180939432,-28.8755214155073));
#30917=CARTESIAN_POINT('Ctrl Pts',(-1.40748309668015,-3.0854823023973,-28.8816047286091));
#30918=CARTESIAN_POINT('Ctrl Pts',(-1.50068710632903,-3.03946430664974,
-28.8876880417109));
#30919=CARTESIAN_POINT('Ctrl Pts',(-1.59390540550658,-2.99343925567493,
-28.893772287473));
#30920=CARTESIAN_POINT('Ctrl Pts',(-1.68498625925461,-2.94313088526703,
-28.8998565332351));
#30921=CARTESIAN_POINT('Ctrl Pts',(-1.77352187946848,-2.88877572780349,
-28.9059407789971));
#30922=CARTESIAN_POINT('Ctrl Pts',(-1.86214918643835,-2.83436428058847,
-28.9120313255538));
#30923=CARTESIAN_POINT('Ctrl Pts',(-1.94822563128211,-2.77589790111196,
-28.9181218721105));
#30924=CARTESIAN_POINT('Ctrl Pts',(-2.03137170533589,-2.71365695275965,
-28.9242124186671));
#30925=CARTESIAN_POINT('Ctrl Pts',(-2.11456275778207,-2.65138233477434,
-28.9303062599433));
#30926=CARTESIAN_POINT('Ctrl Pts',(-2.1948199518761,-2.58532935213631,-28.9364001012195));
#30927=CARTESIAN_POINT('Ctrl Pts',(-2.27179776314108,-2.51581795563335,
-28.9424939424957));
#30928=CARTESIAN_POINT('Ctrl Pts',(-2.34889984238038,-2.4461943444507,-28.9485976212731));
#30929=CARTESIAN_POINT('Ctrl Pts',(-2.42271165960536,-2.37310146742926,
-28.9547013000505));
#30930=CARTESIAN_POINT('Ctrl Pts',(-2.49292523092322,-2.29689548206409,
-28.9608049788279));
#30931=CARTESIAN_POINT('Ctrl Pts',(-2.54593181238301,-2.23936502612564,
-28.9654128507855));
#30932=CARTESIAN_POINT('Ctrl Pts',(-2.59688844964165,-2.18006108216403,
-28.9700207227431));
#30933=CARTESIAN_POINT('Ctrl Pts',(-2.64567876781292,-2.11914815905918,
-28.9746285947007));
#30934=CARTESIAN_POINT('Ctrl Pts',(-2.71006976820936,-2.03875835627035,
-28.9807098316381));
#30935=CARTESIAN_POINT('Ctrl Pts',(-2.77090798108598,-1.95528801259203,
-28.9867910685754));
#30936=CARTESIAN_POINT('Ctrl Pts',(-2.82788370594505,-1.86908501897331,
-28.9928723055128));
#30937=CARTESIAN_POINT('Ctrl Pts',(-2.8847877197454,-1.78299052257781,-28.9989458884547));
#30938=CARTESIAN_POINT('Ctrl Pts',(-2.93783866950888,-1.69417056537816,
-29.0050194713966));
#30939=CARTESIAN_POINT('Ctrl Pts',(-2.98676680436591,-1.60300627535822,
-29.0110930543385));
#30940=CARTESIAN_POINT('Ctrl Pts',(-3.03564623865997,-1.51193272560992,
-29.0171605919466));
#30941=CARTESIAN_POINT('Ctrl Pts',(-3.08041081135924,-1.41851985753198,
-29.0232281295547));
#30942=CARTESIAN_POINT('Ctrl Pts',(-3.12083437687428,-1.32317718186935,
-29.0292956671628));
#30943=CARTESIAN_POINT('Ctrl Pts',(-3.16122834708118,-1.2279043094472,-29.0353587625441));
#30944=CARTESIAN_POINT('Ctrl Pts',(-3.19728746135202,-1.13070483348132,
-29.0414218579254));
#30945=CARTESIAN_POINT('Ctrl Pts',(-3.22883222812558,-1.03201138807553,
-29.0474849533067));
#30946=CARTESIAN_POINT('Ctrl Pts',(-3.2603656937663,-0.933353300285324,
-29.0535458765417));
#30947=CARTESIAN_POINT('Ctrl Pts',(-3.28738789269004,-0.833202715478359,
-29.0596067997768));
#30948=CARTESIAN_POINT('Ctrl Pts',(-3.30976834383676,-0.732009953918703,
-29.0656677230119));
#30949=CARTESIAN_POINT('Ctrl Pts',(-3.33214418542468,-0.630838034386813,
-29.0717273979172));
#30950=CARTESIAN_POINT('Ctrl Pts',(-3.34988009184918,-0.528624786183428,
-29.0777870728226));
#30951=CARTESIAN_POINT('Ctrl Pts',(-3.36289636616285,-0.425832235685285,
-29.0838467477279));
#30952=CARTESIAN_POINT('Ctrl Pts',(-3.37591654326618,-0.323008863947966,
-29.0899082395615));
#30953=CARTESIAN_POINT('Ctrl Pts',(-3.38421421094914,-0.21960627064758,
-29.0959697313952));
#30954=CARTESIAN_POINT('Ctrl Pts',(-3.38776144183851,-0.116092530734182,
-29.1020312232288));
#30955=CARTESIAN_POINT('Ctrl Pts',(-3.38911736260653,-0.0765246440921415,
-29.1043482144027));
#30956=CARTESIAN_POINT('Ctrl Pts',(-3.38977972350901,-0.0369405421840939,
-29.1066652055765));
#30957=CARTESIAN_POINT('Ctrl Pts',(-3.38974897692414,0.00263361762172143,
-29.1089821967504));
#30958=CARTESIAN_POINT('',(-3.39460607963399,-0.000821927281527217,-30.3588436183143));
#30959=CARTESIAN_POINT('Ctrl Pts',(-3.38720500183428,0.00265191974547864,
-29.1089833849163));
#30960=CARTESIAN_POINT('Ctrl Pts',(-3.38984895601398,0.356633419419809,
-29.1297237581471));
#30961=CARTESIAN_POINT('Ctrl Pts',(-3.17696557429075,1.82585356689937,-29.2159894346803));
#30962=CARTESIAN_POINT('Ctrl Pts',(-1.06501084932491,3.84917142339401,-29.3677804145163));
#30963=CARTESIAN_POINT('Ctrl Pts',(2.62793364271971,3.00741003307344,-29.5643563244242));
#30964=CARTESIAN_POINT('Ctrl Pts',(3.95722561382568,-0.539375665666434,
-29.760932234332));
#30965=CARTESIAN_POINT('Ctrl Pts',(1.72720904884221,-3.6010077302552,-29.9575081442399));
#30966=CARTESIAN_POINT('Ctrl Pts',(-2.05632687273503,-3.42374860859984,
-30.1540840541477));
#30967=CARTESIAN_POINT('Ctrl Pts',(-3.37294674464125,-1.2066374231571,-30.2879087383179));
#30968=CARTESIAN_POINT('Ctrl Pts',(-3.39500475544003,-0.0479003925669444,
-30.3562081191854));
#30969=CARTESIAN_POINT('Ctrl Pts',(-3.39484736595381,-0.000830500879896085,
-30.3589821967504));
#30970=CARTESIAN_POINT('',(-3.38974868975108,0.00294214148269599,-32.8590963092955));
#30971=CARTESIAN_POINT('Ctrl Pts',(-3.38974993779964,-0.000649374565975133,
-30.3560545810355));
#30972=CARTESIAN_POINT('Ctrl Pts',(-3.38975358586039,0.0183935851200709,
-30.3572180084951));
#30973=CARTESIAN_POINT('Ctrl Pts',(-3.38959676423955,0.0374358997996179,
-30.3583882915823));
#30974=CARTESIAN_POINT('Ctrl Pts',(-3.38462768886899,0.335646200792595,
-30.3768133563173));
#30975=CARTESIAN_POINT('Ctrl Pts',(-3.34550345502142,0.613167531655111,
-30.3951989018399));
#30976=CARTESIAN_POINT('Ctrl Pts',(-3.2368976225608,1.01582230935899,-30.4216545317372));
#30977=CARTESIAN_POINT('Ctrl Pts',(-3.19291972730513,1.146591548526,-30.4302298245411));
#30978=CARTESIAN_POINT('Ctrl Pts',(-3.12382888221506,1.3168932102243,-30.4413320949894));
#30979=CARTESIAN_POINT('Ctrl Pts',(-3.10569832986211,1.35909999813467,-30.4440788642434));
#30980=CARTESIAN_POINT('Ctrl Pts',(-3.0734127628179,1.43023600271374,-30.4487022476129));
#30981=CARTESIAN_POINT('Ctrl Pts',(-3.05969352188649,1.4593548890198,-30.4505930464342));
#30982=CARTESIAN_POINT('Ctrl Pts',(-3.03098586910261,1.51810137848072,-30.4544057042695));
#30983=CARTESIAN_POINT('Ctrl Pts',(-3.01597274606492,1.54771303606426,-30.4563264647083));
#30984=CARTESIAN_POINT('Ctrl Pts',(-2.97665228767898,1.62252254202551,-30.4611793210982));
#30985=CARTESIAN_POINT('Ctrl Pts',(-2.95174878348213,1.66739849703661,-30.4640906333652));
#30986=CARTESIAN_POINT('Ctrl Pts',(-2.78939052236961,1.94492102040908,-30.4821331493347));
#30987=CARTESIAN_POINT('Ctrl Pts',(-2.62555401588435,2.16099346467813,-30.4962539515895));
#30988=CARTESIAN_POINT('Ctrl Pts',(-2.33298752888244,2.46380283459002,-30.5186929928453));
#30989=CARTESIAN_POINT('Ctrl Pts',(-2.22107088977081,2.56514913547031,-30.5268171500487));
#30990=CARTESIAN_POINT('Ctrl Pts',(-2.07835396388052,2.67802552438949,-30.5371561463535));
#30991=CARTESIAN_POINT('Ctrl Pts',(-2.05365093403885,2.69701568481328,-30.538945216027));
#30992=CARTESIAN_POINT('Ctrl Pts',(-2.01349493299563,2.72701356530531,-30.5418588296425));
#30993=CARTESIAN_POINT('Ctrl Pts',(-1.99820466793537,2.738237188038,-30.5429694810873));
#30994=CARTESIAN_POINT('Ctrl Pts',(-1.96941452280078,2.75900067700612,-30.5450646591374));
#30995=CARTESIAN_POINT('Ctrl Pts',(-1.95593743238517,2.76857129763282,-30.5460470446206));
#30996=CARTESIAN_POINT('Ctrl Pts',(-1.91937028056145,2.79413883664745,-30.5487156445718));
#30997=CARTESIAN_POINT('Ctrl Pts',(-1.89615093553784,2.80994762051065,-30.5504134536519));
#30998=CARTESIAN_POINT('Ctrl Pts',(-1.80036158778415,2.87343748353246,-30.5574223402428));
#30999=CARTESIAN_POINT('Ctrl Pts',(-1.72617317817206,2.9186073214435,-30.5628609836103));
#31000=CARTESIAN_POINT('Ctrl Pts',(-1.46565050443106,3.0638179648495,-30.581796064727));
#31001=CARTESIAN_POINT('Ctrl Pts',(-1.27173459714899,3.14925519353807,-30.5955804791992));
#31002=CARTESIAN_POINT('Ctrl Pts',(-0.938337451312478,3.26029350107068,
-30.6178862033972));
#31003=CARTESIAN_POINT('Ctrl Pts',(-0.802936044667959,3.29625428266166,
-30.6265990125933));
#31004=CARTESIAN_POINT('Ctrl Pts',(-0.620469483723358,3.33279899196888,
-30.637842705927));
#31005=CARTESIAN_POINT('Ctrl Pts',(-0.575072468011883,3.34093152726245,
-30.6406008571791));
#31006=CARTESIAN_POINT('Ctrl Pts',(-0.497698837645476,3.35316849685697,
-30.6452375052567));
#31007=CARTESIAN_POINT('Ctrl Pts',(-0.465804848341566,3.35774761570437,
-30.6471303836792));
#31008=CARTESIAN_POINT('Ctrl Pts',(-0.40097205263779,3.36611428938134,-30.6509425186538));
#31009=CARTESIAN_POINT('Ctrl Pts',(-0.368033252906537,3.36987472073429,
-30.6528607471546));
#31010=CARTESIAN_POINT('Ctrl Pts',(-0.284220177121389,3.37819958997654,
-30.6576976179));
#31011=CARTESIAN_POINT('Ctrl Pts',(-0.233287316671325,3.38209860725056,
-30.6605957628569));
#31012=CARTESIAN_POINT('Ctrl Pts',(0.0891574235648245,3.39946320171763,
-30.6787199088143));
#31013=CARTESIAN_POINT('Ctrl Pts',(0.361364906557596,3.381378977075,-30.6929200469411));
#31014=CARTESIAN_POINT('Ctrl Pts',(0.764319050930901,3.30534781892006,-30.7147773763137));
#31015=CARTESIAN_POINT('Ctrl Pts',(0.898429361952221,3.27144092983636,-30.7222198250094));
#31016=CARTESIAN_POINT('Ctrl Pts',(1.06585770564544,3.21803705276973,-30.7321297064945));
#31017=CARTESIAN_POINT('Ctrl Pts',(1.10143906864696,3.20603288459186,-30.7342725361819));
#31018=CARTESIAN_POINT('Ctrl Pts',(1.15593638274237,3.18663274114377,-30.7376219526686));
#31019=CARTESIAN_POINT('Ctrl Pts',(1.17499858567686,3.17965335004513,-30.7388063847505));
#31020=CARTESIAN_POINT('Ctrl Pts',(1.21084365028319,3.1661627799261,-30.7410599935874));
#31021=CARTESIAN_POINT('Ctrl Pts',(1.22763912509836,3.15968846819308,-30.7421271463286));
#31022=CARTESIAN_POINT('Ctrl Pts',(1.26481807522904,3.14501557903992,-30.744513497048));
#31023=CARTESIAN_POINT('Ctrl Pts',(1.28517494309795,3.1367519931313,-30.7458362356472));
#31024=CARTESIAN_POINT('Ctrl Pts',(1.35672408599625,3.10689422763244,-30.7505388243012));
#31025=CARTESIAN_POINT('Ctrl Pts',(1.40746202492807,3.08424089864925,-30.7539708610622));
#31026=CARTESIAN_POINT('Ctrl Pts',(1.70128762465155,2.94429450830231,-30.7743295317852));
#31027=CARTESIAN_POINT('Ctrl Pts',(1.93022654619818,2.79955124171538,-30.7920683964197));
#31028=CARTESIAN_POINT('Ctrl Pts',(2.23628508126793,2.55048585564335,-30.8169926153582));
#31029=CARTESIAN_POINT('Ctrl Pts',(2.32857919049858,2.4665104081326,-30.8247187570141));
#31030=CARTESIAN_POINT('Ctrl Pts',(2.44737772359241,2.34579258475137,-30.8349372444732));
#31031=CARTESIAN_POINT('Ctrl Pts',(2.47807946608571,2.31333590653276,-30.8376059556947));
#31032=CARTESIAN_POINT('Ctrl Pts',(2.52963885632384,2.2566245769547,-30.8421385967796));
#31033=CARTESIAN_POINT('Ctrl Pts',(2.55081065844471,2.23266484569021,-30.8440153797736));
#31034=CARTESIAN_POINT('Ctrl Pts',(2.59349955623754,2.18295460770493,-30.8478335258827));
#31035=CARTESIAN_POINT('Ctrl Pts',(2.61497966247934,2.15717691641315,-30.8497732830369));
#31036=CARTESIAN_POINT('Ctrl Pts',(2.66946478974455,2.08978077420758,-30.8547455137727));
#31037=CARTESIAN_POINT('Ctrl Pts',(2.70188131644235,2.04769717653687,-30.8577550206317));
#31038=CARTESIAN_POINT('Ctrl Pts',(2.88563712258405,1.79717730281712,-30.8751621516245));
#31039=CARTESIAN_POINT('Ctrl Pts',(3.0138089091122,1.57280440756817,-30.8886641721784));
#31040=CARTESIAN_POINT('Ctrl Pts',(3.17317778296728,1.20120034184514,-30.9101828213359));
#31041=CARTESIAN_POINT('Ctrl Pts',(3.22219382509087,1.0627317264624,-30.9180571031675));
#31042=CARTESIAN_POINT('Ctrl Pts',(3.27254393858055,0.884501223844759,-30.9284902939929));
#31043=CARTESIAN_POINT('Ctrl Pts',(3.28237481676887,0.847290710213697,-30.9306847139773));
#31044=CARTESIAN_POINT('Ctrl Pts',(3.29646496063004,0.790027594424019,-30.934097537345));
#31045=CARTESIAN_POINT('Ctrl Pts',(3.3011797000572,0.770089201540251,-30.9352924482041));
#31046=CARTESIAN_POINT('Ctrl Pts',(3.30968325137306,0.732614286937175,-30.9375527490426));
#31047=CARTESIAN_POINT('Ctrl Pts',(3.31351403276588,0.715088537662129,-30.9386158838828));
#31048=CARTESIAN_POINT('Ctrl Pts',(3.32166593970426,0.676321162212311,-30.9409801464701));
#31049=CARTESIAN_POINT('Ctrl Pts',(3.32592275572679,0.655066942645862,-30.9422845680587));
#31050=CARTESIAN_POINT('Ctrl Pts',(3.34001226484938,0.581037841138695,-30.9468529935358));
#31051=CARTESIAN_POINT('Ctrl Pts',(3.34879448592506,0.528073613371486,-30.9501655784687));
#31052=CARTESIAN_POINT('Ctrl Pts',(3.38452860039689,0.275539848205004,-30.9661010284483));
#31053=CARTESIAN_POINT('Ctrl Pts',(3.39491817418889,0.0740432031104546,
-30.9792051319548));
#31054=CARTESIAN_POINT('Ctrl Pts',(3.38163810647879,-0.279671140503619,
-31.0019063365813));
#31055=CARTESIAN_POINT('Ctrl Pts',(3.36562139752001,-0.431617184740064,
-31.011564881812));
#31056=CARTESIAN_POINT('Ctrl Pts',(3.32793447347453,-0.647865681019166,
-31.0250482061445));
#31057=CARTESIAN_POINT('Ctrl Pts',(3.31450435326363,-0.713400046439247,
-31.0291007808305));
#31058=CARTESIAN_POINT('Ctrl Pts',(3.290816242993,-0.813786298513853,-31.0352586647297));
#31059=CARTESIAN_POINT('Ctrl Pts',(3.28192333621835,-0.848939957908778,
-31.0374055805387));
#31060=CARTESIAN_POINT('Ctrl Pts',(3.26431562386488,-0.914125753838241,
-31.0413705777434));
#31061=CARTESIAN_POINT('Ctrl Pts',(3.25574607288868,-0.944192772074268,
-31.0431930101717));
#31062=CARTESIAN_POINT('Ctrl Pts',(3.23554107049048,-1.01153522880078,-31.0472622047982));
#31063=CARTESIAN_POINT('Ctrl Pts',(3.22367494195662,-1.04873713834653,-31.0495013597448));
#31064=CARTESIAN_POINT('Ctrl Pts',(3.18473935515363,-1.16389384009055,-31.0564119852642));
#31065=CARTESIAN_POINT('Ctrl Pts',(3.15546384164881,-1.24107333208645,-31.0610131287288));
#31066=CARTESIAN_POINT('Ctrl Pts',(3.02033272395213,-1.561523262308,-31.0801133717575));
#31067=CARTESIAN_POINT('Ctrl Pts',(2.88894199897272,-1.79297903821589,-31.0938220249885));
#31068=CARTESIAN_POINT('Ctrl Pts',(2.66873258781607,-2.09276426137196,-31.1138838507305));
#31069=CARTESIAN_POINT('Ctrl Pts',(2.60152728493106,-2.17574074135049,-31.1197370653941));
#31070=CARTESIAN_POINT('Ctrl Pts',(2.51118570885472,-2.27710263487643,-31.1274739734095));
#31071=CARTESIAN_POINT('Ctrl Pts',(2.49156666228204,-2.29855291897373,-31.129146974005));
#31072=CARTESIAN_POINT('Ctrl Pts',(2.45899196872442,-2.33326102979367,-31.1319183014254));
#31073=CARTESIAN_POINT('Ctrl Pts',(2.44619864511566,-2.34667013097372,-31.133005133312));
#31074=CARTESIAN_POINT('Ctrl Pts',(2.42155200053846,-2.37208252938787,-31.13509748181));
#31075=CARTESIAN_POINT('Ctrl Pts',(2.40971787143615,-2.38410347319309,-31.1361014268424));
#31076=CARTESIAN_POINT('Ctrl Pts',(2.37661642666656,-2.41722922550645,-31.1389063488815));
#31077=CARTESIAN_POINT('Ctrl Pts',(2.35515876809471,-2.43814064632731,-31.1407209612995));
#31078=CARTESIAN_POINT('Ctrl Pts',(2.25366893908093,-2.53445698889195,-31.1492748622876));
#31079=CARTESIAN_POINT('Ctrl Pts',(2.17028077094357,-2.60621819292162,-31.1562192221584));
#31080=CARTESIAN_POINT('Ctrl Pts',(1.91336028027547,-2.80642414761847,-31.1770409533759));
#31081=CARTESIAN_POINT('Ctrl Pts',(1.73086873725762,-2.9225106954594,-31.1910779954124));
#31082=CARTESIAN_POINT('Ctrl Pts',(1.43637285272958,-3.07252245211751,-31.2118770165785));
#31083=CARTESIAN_POINT('Ctrl Pts',(1.33158442983635,-3.11936668329667,-31.2189621857435));
#31084=CARTESIAN_POINT('Ctrl Pts',(1.18398532194336,-3.17655193541285,-31.2285011635569));
#31085=CARTESIAN_POINT('Ctrl Pts',(1.1430565847263,-3.19150831877507,-31.2311016341303));
#31086=CARTESIAN_POINT('Ctrl Pts',(1.07178142141577,-3.21600692490374,-31.2355555292295));
#31087=CARTESIAN_POINT('Ctrl Pts',(1.04156880579328,-3.22591854841439,-31.237420664576));
#31088=CARTESIAN_POINT('Ctrl Pts',(0.978849006700675,-3.24552152358349,
-31.2412472727363));
#31089=CARTESIAN_POINT('Ctrl Pts',(0.946326761894156,-3.25515300986888,
-31.2432066539072));
#31090=CARTESIAN_POINT('Ctrl Pts',(0.860754032928103,-3.27910451233216,
-31.2483007943268));
#31091=CARTESIAN_POINT('Ctrl Pts',(0.807489367090337,-3.29262589731823,
-31.2514102832812));
#31092=CARTESIAN_POINT('Ctrl Pts',(0.492708646638066,-3.36443516720367,
-31.2694722150127));
#31093=CARTESIAN_POINT('Ctrl Pts',(0.225363753175854,-3.39284610137639,
-31.2834540394444));
#31094=CARTESIAN_POINT('Ctrl Pts',(-0.177568226748785,-3.38778802702845,
-31.3049473012839));
#31095=CARTESIAN_POINT('Ctrl Pts',(-0.312354514032439,-3.37802700749997,
-31.3122280911118));
#31096=CARTESIAN_POINT('Ctrl Pts',(-0.483051111407701,-3.35536133102859,
-31.3219419687302));
#31097=CARTESIAN_POINT('Ctrl Pts',(-0.519831307236549,-3.34986017823292,
-31.324064799933));
#31098=CARTESIAN_POINT('Ctrl Pts',(-0.57646385365794,-3.34043464134589,
-31.3273896225132));
#31099=CARTESIAN_POINT('Ctrl Pts',(-0.596385091183429,-3.33693556216593,
-31.3285699686353));
#31100=CARTESIAN_POINT('Ctrl Pts',(-0.633999875348368,-3.32998111020143,
-31.3308211221208));
#31101=CARTESIAN_POINT('Ctrl Pts',(-0.651699041172491,-3.3265625409341,
-31.331889997046));
#31102=CARTESIAN_POINT('Ctrl Pts',(-0.695153995144886,-3.31780918677776,
-31.3345369701652));
#31103=CARTESIAN_POINT('Ctrl Pts',(-0.720876260432146,-3.3123155345849,
-31.3361233488398));
#31104=CARTESIAN_POINT('Ctrl Pts',(-0.815382451359608,-3.29097837628167,
-31.3420176290571));
#31105=CARTESIAN_POINT('Ctrl Pts',(-0.883726996536045,-3.2732877148343,
-31.3464088891587));
#31106=CARTESIAN_POINT('Ctrl Pts',(-1.15069441629301,-3.19521432818874,
-31.3639480880346));
#31107=CARTESIAN_POINT('Ctrl Pts',(-1.34414885486117,-3.1187748856563,-31.3774813509711));
#31108=CARTESIAN_POINT('Ctrl Pts',(-1.67265408044434,-2.95269397310375,
-31.4009737300191));
#31109=CARTESIAN_POINT('Ctrl Pts',(-1.8105999990087,-2.87017634948374,-31.4110255271459));
#31110=CARTESIAN_POINT('Ctrl Pts',(-1.98123214383969,-2.75088953250633,
-31.4236232491918));
#31111=CARTESIAN_POINT('Ctrl Pts',(-2.01969365205259,-2.72277651001239,
-31.4264757348992));
#31112=CARTESIAN_POINT('Ctrl Pts',(-2.08337439829182,-2.67413762220135,
-31.4312227803155));
#31113=CARTESIAN_POINT('Ctrl Pts',(-2.10891313394441,-2.65404340741461,
-31.4331333760073));
#31114=CARTESIAN_POINT('Ctrl Pts',(-2.15964403504852,-2.61293295846624,
-31.4369440892849));
#31115=CARTESIAN_POINT('Ctrl Pts',(-2.18482791607657,-2.59191205289224,
-31.4388437315206));
#31116=CARTESIAN_POINT('Ctrl Pts',(-2.2470661261945,-2.53841021860493,-31.4435612846616));
#31117=CARTESIAN_POINT('Ctrl Pts',(-2.28372541499067,-2.50548023100485,
-31.4463608035753));
#31118=CARTESIAN_POINT('Ctrl Pts',(-2.45952312509443,-2.34050069784782,
-31.4599145126943));
#31119=CARTESIAN_POINT('Ctrl Pts',(-2.58800306304386,-2.19760047538392,
-31.4702014995828));
#31120=CARTESIAN_POINT('Ctrl Pts',(-2.80117968844916,-1.91570047109187,
-31.4889814926882));
#31121=CARTESIAN_POINT('Ctrl Pts',(-2.88929913646434,-1.78001725553925,
-31.4974854665794));
#31122=CARTESIAN_POINT('Ctrl Pts',(-3.0063804044293,-1.56798722171135,-31.5107048219017));
#31123=CARTESIAN_POINT('Ctrl Pts',(-3.04282476609623,-1.49603563394987,
-31.5151816000568));
#31124=CARTESIAN_POINT('Ctrl Pts',(-3.08791348911589,-1.39853968837005,
-31.5213230846099));
#31125=CARTESIAN_POINT('Ctrl Pts',(-3.09887121004895,-1.3740888266969,-31.5228694658023));
#31126=CARTESIAN_POINT('Ctrl Pts',(-3.11674643476429,-1.33290082348334,
-31.5254887807842));
#31127=CARTESIAN_POINT('Ctrl Pts',(-3.12382196957048,-1.31623297210885,
-31.5265527020305));
#31128=CARTESIAN_POINT('Ctrl Pts',(-3.13843874201812,-1.28101840006851,
-31.5288100932665));
#31129=CARTESIAN_POINT('Ctrl Pts',(-3.14594967364051,-1.2624604887601,-31.5300050893711));
#31130=CARTESIAN_POINT('Ctrl Pts',(-3.16657198964786,-1.21018014684543,
-31.5333843687216));
#31131=CARTESIAN_POINT('Ctrl Pts',(-3.17930811826689,-1.17631365587963,
-31.5355882500344));
#31132=CARTESIAN_POINT('Ctrl Pts',(-3.25903044485002,-0.953566054130738,
-31.5501507697102));
#31133=CARTESIAN_POINT('Ctrl Pts',(-3.30969138629977,-0.759276356119579,
-31.5631406951041));
#31134=CARTESIAN_POINT('Ctrl Pts',(-3.37397414946623,-0.376681038970963,
-31.5881030590623));
#31135=CARTESIAN_POINT('Ctrl Pts',(-3.38964994078012,-0.18941699283998,
-31.6000439579888));
#31136=CARTESIAN_POINT('Ctrl Pts',(-3.38978312762711,0.0615147941664754,
-31.6154282675448));
#31137=CARTESIAN_POINT('Ctrl Pts',(-3.38804286396248,0.124820145480946,
-31.6192598203274));
#31138=CARTESIAN_POINT('Ctrl Pts',(-3.38253750698137,0.2239094912087,-31.6251815825254));
#31139=CARTESIAN_POINT('Ctrl Pts',(-3.37997471952741,0.259743122505757,
-31.6273075993727));
#31140=CARTESIAN_POINT('Ctrl Pts',(-3.3741402368697,0.326410161288458,-31.6312357700132));
#31141=CARTESIAN_POINT('Ctrl Pts',(-3.37101422179426,0.357252209755165,
-31.6330421747588));
#31142=CARTESIAN_POINT('Ctrl Pts',(-3.36295968665067,0.427149187713094,
-31.6371131890979));
#31143=CARTESIAN_POINT('Ctrl Pts',(-3.35777304254378,0.46617020530461,-31.6393696396726));
#31144=CARTESIAN_POINT('Ctrl Pts',(-3.33932622318197,0.588587283645547,
-31.6464045742842));
#31145=CARTESIAN_POINT('Ctrl Pts',(-3.32362880756328,0.671585956597162,
-31.651108833398));
#31146=CARTESIAN_POINT('Ctrl Pts',(-3.27739247631794,0.874266210733162,
-31.6625141662718));
#31147=CARTESIAN_POINT('Ctrl Pts',(-3.24338325313892,0.993030929851279,
-31.6691230888089));
#31148=CARTESIAN_POINT('Ctrl Pts',(-3.1379873819616,1.29724452423116,-31.6862442555137));
#31149=CARTESIAN_POINT('Ctrl Pts',(-3.05666034620139,1.47872372431097,-31.6966421048332));
#31150=CARTESIAN_POINT('Ctrl Pts',(-2.93219055899067,1.70173554570051,-31.7107787541576));
#31151=CARTESIAN_POINT('Ctrl Pts',(-2.90320223456133,1.75073167176077,-31.7139771063007));
#31152=CARTESIAN_POINT('Ctrl Pts',(-2.86123199463675,1.81775902758378,-31.7185152066177));
#31153=CARTESIAN_POINT('Ctrl Pts',(-2.849284439942,1.83642983382003,-31.7197973638296));
#31154=CARTESIAN_POINT('Ctrl Pts',(-2.82728133788243,1.87008311138499,-31.7221438584359));
#31155=CARTESIAN_POINT('Ctrl Pts',(-2.81728748102431,1.88510526156291,-31.7232043707742));
#31156=CARTESIAN_POINT('Ctrl Pts',(-2.79586161058957,1.91676034651899,-31.7254682511059));
#31157=CARTESIAN_POINT('Ctrl Pts',(-2.78440038023395,1.93337188589797,-31.726673343539));
#31158=CARTESIAN_POINT('Ctrl Pts',(-2.7515255730235,1.98012092380728,-31.7301111764313));
#31159=CARTESIAN_POINT('Ctrl Pts',(-2.72976691925459,2.01001098979437,-31.7323645531217));
#31160=CARTESIAN_POINT('Ctrl Pts',(-2.6274154052913,2.14588454376703,-31.7428434427406));
#31161=CARTESIAN_POINT('Ctrl Pts',(-2.5411158452899,2.24741117268509,-31.7513412359955));
#31162=CARTESIAN_POINT('Ctrl Pts',(-2.26819701550289,2.5326142250237,-31.7767190618677));
#31163=CARTESIAN_POINT('Ctrl Pts',(-2.0660095510784,2.70009185771265,-31.7936126499004));
#31164=CARTESIAN_POINT('Ctrl Pts',(-1.79665773550346,2.87505919633643,-31.8132402997515));
#31165=CARTESIAN_POINT('Ctrl Pts',(-1.74592067088237,2.90614969928204,-31.8168308718305));
#31166=CARTESIAN_POINT('Ctrl Pts',(-1.66423033155405,2.95329561085724,-31.8224480814199));
#31167=CARTESIAN_POINT('Ctrl Pts',(-1.63380441738222,2.97023581925327,-31.8245054388823));
#31168=CARTESIAN_POINT('Ctrl Pts',(-1.5753745936035,3.00159818893879,-31.8283923021979));
#31169=CARTESIAN_POINT('Ctrl Pts',(-1.54742032582661,3.01610464522101,-31.8302245892822));
#31170=CARTESIAN_POINT('Ctrl Pts',(-1.48224308591919,3.04878268597412,-31.8344360829827));
#31171=CARTESIAN_POINT('Ctrl Pts',(-1.4448807483035,3.06666598550343,-31.836805305535));
#31172=CARTESIAN_POINT('Ctrl Pts',(-1.31805167502983,3.12453945903911,-31.8447070252748));
#31173=CARTESIAN_POINT('Ctrl Pts',(-1.22717814192728,3.16133565592759,-31.8501349281128));
#31174=CARTESIAN_POINT('Ctrl Pts',(-0.986111908821109,3.24698288881799,
-31.8640751206751));
#31175=CARTESIAN_POINT('Ctrl Pts',(-0.833878446965317,3.28937138779607,
-31.8724232977448));
#31176=CARTESIAN_POINT('Ctrl Pts',(-0.506442979825628,3.35634170408778,
-31.890164647432));
#31177=CARTESIAN_POINT('Ctrl Pts',(-0.331164349304396,3.37814030561119,
-31.8995398491931));
#31178=CARTESIAN_POINT('Ctrl Pts',(-0.117553032608832,3.38791853982606,
-31.9115987182643));
#31179=CARTESIAN_POINT('Ctrl Pts',(-0.0800755107179769,3.38901142207123,
-31.913738332117));
#31180=CARTESIAN_POINT('Ctrl Pts',(-0.0223027143843366,3.38973734361808,
-31.9170837959744));
#31181=CARTESIAN_POINT('Ctrl Pts',(-0.00201488321266023,3.38981010751676,
-31.9182675736157));
#31182=CARTESIAN_POINT('Ctrl Pts',(0.0362765871823664,3.38960370143624,
-31.9205207864142));
#31183=CARTESIAN_POINT('Ctrl Pts',(0.0542792560688647,3.38936320699878,
-31.921588212222));
#31184=CARTESIAN_POINT('Ctrl Pts',(0.098436095638436,3.38842145000747,-31.9242252253323));
#31185=CARTESIAN_POINT('Ctrl Pts',(0.124585379097539,3.38756077128252,-31.9258029486986));
#31186=CARTESIAN_POINT('Ctrl Pts',(0.225616488988718,3.38306409652593,-31.9319543071364));
#31187=CARTESIAN_POINT('Ctrl Pts',(0.300375523299408,3.37724716842197,-31.9366239480884));
#31188=CARTESIAN_POINT('Ctrl Pts',(0.514852363709143,3.35338165008466,-31.9502518840086));
#31189=CARTESIAN_POINT('Ctrl Pts',(0.653718906426079,3.32909758153468,-31.9593545271832));
#31190=CARTESIAN_POINT('Ctrl Pts',(0.989310970128799,3.24859945502809,-31.9815659663391));
#31191=CARTESIAN_POINT('Ctrl Pts',(1.18326424187125,3.18308668880355,-31.9945659487405));
#31192=CARTESIAN_POINT('Ctrl Pts',(1.42227296697476,3.07746505795901,-32.0105037632757));
#31193=CARTESIAN_POINT('Ctrl Pts',(1.47380227550438,3.05312282948597,-32.0139374851677));
#31194=CARTESIAN_POINT('Ctrl Pts',(1.55534919393424,3.01205443055906,-32.0193699712372));
#31195=CARTESIAN_POINT('Ctrl Pts',(1.58576711087045,2.99615183304998,-32.0213960619647));
#31196=CARTESIAN_POINT('Ctrl Pts',(1.64375118639079,2.96470708365515,-32.0252593338896));
#31197=CARTESIAN_POINT('Ctrl Pts',(1.67135138484922,2.94923561315491,-32.0270987050851));
#31198=CARTESIAN_POINT('Ctrl Pts',(1.73552636554924,2.91207163013642,-32.0313788423397));
#31199=CARTESIAN_POINT('Ctrl Pts',(1.77191801240698,2.89007261667187,-32.0338085054089));
#31200=CARTESIAN_POINT('Ctrl Pts',(1.89768126572133,2.8107790876379,-32.0422245505969));
#31201=CARTESIAN_POINT('Ctrl Pts',(1.98477085140624,2.74997467757229,-32.0480855612713));
#31202=CARTESIAN_POINT('Ctrl Pts',(2.21393355248003,2.57341004853675,-32.0637920611664));
#31203=CARTESIAN_POINT('Ctrl Pts',(2.34970155506746,2.45007046090556,-32.0734064596452));
#31204=CARTESIAN_POINT('Ctrl Pts',(2.57014801469695,2.21454176109213,-32.0905967447949));
#31205=CARTESIAN_POINT('Ctrl Pts',(2.65906876710816,2.10694149250063,-32.0981020864618));
#31206=CARTESIAN_POINT('Ctrl Pts',(2.76310286252025,1.96394148972013,-32.1080709398795));
#31207=CARTESIAN_POINT('Ctrl Pts',(2.78460059642656,1.93333982615192,-32.1102041800757));
#31208=CARTESIAN_POINT('Ctrl Pts',(2.81708420911127,1.88543398810376,-32.1135539007433));
#31209=CARTESIAN_POINT('Ctrl Pts',(2.82842741694695,1.86837444469237,-32.1147487141164));
#31210=CARTESIAN_POINT('Ctrl Pts',(2.84941285908234,1.83618443932647,-32.117008950484));
#31211=CARTESIAN_POINT('Ctrl Pts',(2.85909067812979,1.8210786295864,-32.1180721204738));
#31212=CARTESIAN_POINT('Ctrl Pts',(2.8823611629749,1.78411371815477,-32.1206789683108));
#31213=CARTESIAN_POINT('Ctrl Pts',(2.89582542962505,1.76217553789551,-32.1222303431389));
#31214=CARTESIAN_POINT('Ctrl Pts',(2.94570527484293,1.67878753559441,-32.1281369079505));
#31215=CARTESIAN_POINT('Ctrl Pts',(2.98042331006988,1.61634855318705,-32.132579024001));
#31216=CARTESIAN_POINT('Ctrl Pts',(3.07234527818099,1.43798535665711,-32.1452297597084));
#31217=CARTESIAN_POINT('Ctrl Pts',(3.12492931626678,1.31981883226846,-32.1535629874766));
#31218=CARTESIAN_POINT('Ctrl Pts',(3.24880426378119,0.992228474152067,-32.176119208664));
#31219=CARTESIAN_POINT('Ctrl Pts',(3.3065788698723,0.778336777817994,-32.1902337703155));
#31220=CARTESIAN_POINT('Ctrl Pts',(3.35248530657016,0.504438051843582,-32.2071684646287));
#31221=CARTESIAN_POINT('Ctrl Pts',(3.36044900439171,0.448328609347779,-32.2105823844214));
#31222=CARTESIAN_POINT('Ctrl Pts',(3.37096480876573,0.358015257199794,-32.2159915193428));
#31223=CARTESIAN_POINT('Ctrl Pts',(3.37441095293715,0.323928256234341,-32.218013643369));
#31224=CARTESIAN_POINT('Ctrl Pts',(3.3800465500495,0.258249420312573,-32.2218741079838));
#31225=CARTESIAN_POINT('Ctrl Pts',(3.38231122830191,0.226667813291584,-32.2237145611959));
#31226=CARTESIAN_POINT('Ctrl Pts',(3.3865887272523,0.152456024550003,-32.2280043714101));
#31227=CARTESIAN_POINT('Ctrl Pts',(3.3882396699065,0.109809910105548,-32.2304424681138));
#31228=CARTESIAN_POINT('Ctrl Pts',(3.39121134650218,-0.0401882388950468,
-32.2389336755888));
#31229=CARTESIAN_POINT('Ctrl Pts',(3.38823803065253,-0.147564949478124,
-32.2448581995395));
#31230=CARTESIAN_POINT('Ctrl Pts',(3.36610672161663,-0.441358165040796,
-32.2608460982377));
#31231=CARTESIAN_POINT('Ctrl Pts',(3.33659166492752,-0.62660097884051,-32.2706663102546));
#31232=CARTESIAN_POINT('Ctrl Pts',(3.25714029832741,-0.950114912834011,
-32.2884352569169));
#31233=CARTESIAN_POINT('Ctrl Pts',(3.2132478738,-1.08936260214783,-32.2963064735893));
#31234=CARTESIAN_POINT('Ctrl Pts',(3.14929521940141,-1.25431688309618,-32.3063599861259));
#31235=CARTESIAN_POINT('Ctrl Pts',(3.13766154034045,-1.28314112082145,-32.3081448760513));
#31236=CARTESIAN_POINT('Ctrl Pts',(3.11829954372731,-1.32927505674184,-32.3110533355167));
#31237=CARTESIAN_POINT('Ctrl Pts',(3.1108192804485,-1.34668763553904,-32.3121631006307));
#31238=CARTESIAN_POINT('Ctrl Pts',(3.09562955989563,-1.38124437711319,-32.3143912659401));
#31239=CARTESIAN_POINT('Ctrl Pts',(3.08792272816441,-1.39838892493502,-32.315509501979));
#31240=CARTESIAN_POINT('Ctrl Pts',(3.06739895524313,-1.44304888086376,-32.318454249752));
#31241=CARTESIAN_POINT('Ctrl Pts',(3.05435455372184,-1.47045725694347,-32.320293355575));
#31242=CARTESIAN_POINT('Ctrl Pts',(2.98395928949409,-1.61338983658263,-32.3300384998974));
#31243=CARTESIAN_POINT('Ctrl Pts',(2.92042174311111,-1.72573777021295,-32.3382291574329));
#31244=CARTESIAN_POINT('Ctrl Pts',(2.69361283367331,-2.07823914721996,-32.3651213095349));
#31245=CARTESIAN_POINT('Ctrl Pts',(2.50585382551528,-2.30116920387337,-32.3839268416348));
#31246=CARTESIAN_POINT('Ctrl Pts',(2.25290887969975,-2.53330154638374,-32.4048001253975));
#31247=CARTESIAN_POINT('Ctrl Pts',(2.21301573554108,-2.568224478344,-32.407986713381));
#31248=CARTESIAN_POINT('Ctrl Pts',(2.14657718375927,-2.62368744553067,-32.4131274901556));
#31249=CARTESIAN_POINT('Ctrl Pts',(2.12051815003745,-2.64479343486468,-32.4151039633982));
#31250=CARTESIAN_POINT('Ctrl Pts',(2.06900042786337,-2.6852681727254,-32.4189359783705));
#31251=CARTESIAN_POINT('Ctrl Pts',(2.04357237033501,-2.70467003514258,-32.4207926903968));
#31252=CARTESIAN_POINT('Ctrl Pts',(1.98192580392429,-2.75034117936147,-32.425214084892));
#31253=CARTESIAN_POINT('Ctrl Pts',(1.94545392811741,-2.77625931278211,-32.4277653615304));
#31254=CARTESIAN_POINT('Ctrl Pts',(1.80491013733798,-2.8720043419099,-32.4373686253088));
#31255=CARTESIAN_POINT('Ctrl Pts',(1.69750361703348,-2.93676611928618,-32.4442388628275));
#31256=CARTESIAN_POINT('Ctrl Pts',(1.34415497828158,-3.123942761491,-32.4657902318559));
#31257=CARTESIAN_POINT('Ctrl Pts',(1.08687652711141,-3.22249015303326,-32.4798868563597));
#31258=CARTESIAN_POINT('Ctrl Pts',(0.769552245225484,-3.30165993559616,
-32.4980623491101));
#31259=CARTESIAN_POINT('Ctrl Pts',(0.718256367792776,-3.31319727398392,
-32.5010266801109));
#31260=CARTESIAN_POINT('Ctrl Pts',(0.644004175609585,-3.32809258626547,
-32.5053817130149));
#31261=CARTESIAN_POINT('Ctrl Pts',(0.621247062055888,-3.33241559001659,
-32.5067250631894));
#31262=CARTESIAN_POINT('Ctrl Pts',(0.581023092180704,-3.33963031317349,
-32.509117432149));
#31263=CARTESIAN_POINT('Ctrl Pts',(0.563575052827663,-3.34261897321262,
-32.5101612348143));
#31264=CARTESIAN_POINT('Ctrl Pts',(0.524552456121503,-3.34898889524847,
-32.5125097540141));
#31265=CARTESIAN_POINT('Ctrl Pts',(0.50296822981662,-3.35229843596043,-32.5138180573591));
#31266=CARTESIAN_POINT('Ctrl Pts',(0.436285988334247,-3.36186444418595,
-32.5178854159327));
#31267=CARTESIAN_POINT('Ctrl Pts',(0.39109435450394,-3.36742079155512,-32.5206777677869));
#31268=CARTESIAN_POINT('Ctrl Pts',(0.114982040658503,-3.39573624603538,
-32.5379027112432));
#31269=CARTESIAN_POINT('Ctrl Pts',(-0.117654664896214,-3.39564404651224,
-32.5530651210382));
#31270=CARTESIAN_POINT('Ctrl Pts',(-0.517842806298667,-3.35428736911374,
-32.578799343628));
#31271=CARTESIAN_POINT('Ctrl Pts',(-0.685691389440883,-3.3240405318538,
-32.5894941377782));
#31272=CARTESIAN_POINT('Ctrl Pts',(-0.897627094507028,-3.26910284516409,
-32.6027542036788));
#31273=CARTESIAN_POINT('Ctrl Pts',(-0.944413978038173,-3.25589471822949,
-32.6056671839362));
#31274=CARTESIAN_POINT('Ctrl Pts',(-1.01903147845844,-3.23308599954552,
-32.6102919403707));
#31275=CARTESIAN_POINT('Ctrl Pts',(-1.04704800175423,-3.22412170948235,
-32.6120236053747));
#31276=CARTESIAN_POINT('Ctrl Pts',(-1.10535487052155,-3.20462538044818,
-32.6156186140622));
#31277=CARTESIAN_POINT('Ctrl Pts',(-1.13561968478087,-3.19402586916629,
-32.6174795781308));
#31278=CARTESIAN_POINT('Ctrl Pts',(-1.20819941916067,-3.16744451709117,
-32.6219326170104));
#31279=CARTESIAN_POINT('Ctrl Pts',(-1.25035428585623,-3.15104189697381,
-32.6245107660179));
#31280=CARTESIAN_POINT('Ctrl Pts',(-1.41256033509321,-3.084158960479,-32.6344136924874));
#31281=CARTESIAN_POINT('Ctrl Pts',(-1.52999665373768,-3.0276192075684,-32.6415405300569));
#31282=CARTESIAN_POINT('Ctrl Pts',(-1.76616463944526,-2.89665564350464,
-32.6560718204154));
#31283=CARTESIAN_POINT('Ctrl Pts',(-1.8841220704842,-2.82135361801482,-32.6634438310438));
#31284=CARTESIAN_POINT('Ctrl Pts',(-2.11924823593796,-2.64991457901812,
-32.6789217512281));
#31285=CARTESIAN_POINT('Ctrl Pts',(-2.23529825359217,-2.55278156768532,
-32.6870223784718));
#31286=CARTESIAN_POINT('Ctrl Pts',(-2.37185952638152,-2.42200863642846,
-32.69767502404));
#31287=CARTESIAN_POINT('Ctrl Pts',(-2.39880820687299,-2.39532093594945,
-32.6998374277481));
#31288=CARTESIAN_POINT('Ctrl Pts',(-2.43969310712116,-2.35345000104187,
-32.7032232790171));
#31289=CARTESIAN_POINT('Ctrl Pts',(-2.45394890706871,-2.33858163829019,
-32.7044243185735));
#31290=CARTESIAN_POINT('Ctrl Pts',(-2.4803439031346,-2.31054537032509,-32.706688768304));
#31291=CARTESIAN_POINT('Ctrl Pts',(-2.49251561042367,-2.29740977253695,
-32.7077497902968));
#31292=CARTESIAN_POINT('Ctrl Pts',(-2.5217767051608,-2.26532523254966,-32.710340781097));
#31293=CARTESIAN_POINT('Ctrl Pts',(-2.53875705177506,-2.24627885761541,
-32.711878214781));
#31294=CARTESIAN_POINT('Ctrl Pts',(-2.60126714011425,-2.17454886619738,
-32.7176599079028));
#31295=CARTESIAN_POINT('Ctrl Pts',(-2.64538277147758,-2.12066078960656,
-32.7219866406303));
#31296=CARTESIAN_POINT('Ctrl Pts',(-2.76316635254191,-1.96738752660349,
-32.7341630345344));
#31297=CARTESIAN_POINT('Ctrl Pts',(-2.83310125761782,-1.86527125512021,
-32.7421280416902));
#31298=CARTESIAN_POINT('Ctrl Pts',(-3.01570796189553,-1.56459164389676,
-32.7647866628734));
#31299=CARTESIAN_POINT('Ctrl Pts',(-3.11415140262951,-1.35813482925953,
-32.7793827059522));
#31300=CARTESIAN_POINT('Ctrl Pts',(-3.21036196650114,-1.08960455034356,
-32.7967818562704));
#31301=CARTESIAN_POINT('Ctrl Pts',(-3.22825203253292,-1.03539916600064,
-32.8002212944883));
#31302=CARTESIAN_POINT('Ctrl Pts',(-3.25470122570166,-0.947894610968836,
-32.8056605203366));
#31303=CARTESIAN_POINT('Ctrl Pts',(-3.26413695295494,-0.914873949533435,
-32.807687755527));
#31304=CARTESIAN_POINT('Ctrl Pts',(-3.28129748812828,-0.851171227284105,
-32.8115518459151));
#31305=CARTESIAN_POINT('Ctrl Pts',(-3.2890976801872,-0.820513383675932,
-32.8133909133239));
#31306=CARTESIAN_POINT('Ctrl Pts',(-3.30636380053194,-0.74844348222983,
-32.8176683040146));
#31307=CARTESIAN_POINT('Ctrl Pts',(-3.31548283813274,-0.70695332569466,
-32.8200955689807));
#31308=CARTESIAN_POINT('Ctrl Pts',(-3.33789481238578,-0.594983969278794,
-32.8265599203939));
#31309=CARTESIAN_POINT('Ctrl Pts',(-3.34973529178031,-0.524234790278472,
-32.8305532037746));
#31310=CARTESIAN_POINT('Ctrl Pts',(-3.37971578929821,-0.301986095678115,
-32.8428764286686));
#31311=CARTESIAN_POINT('Ctrl Pts',(-3.38988114114937,-0.149605677499533,
-32.8509992266607));
#31312=CARTESIAN_POINT('Ctrl Pts',(-3.38974872291658,0.00294244548350111,
-32.859096383374));
#31313=CARTESIAN_POINT('',(-3.38974995202214,-0.000570320900454691,-35.3620086083019));
#31314=CARTESIAN_POINT('Ctrl Pts',(-3.38974872318309,0.00294213844468618,
-32.8590963670765));
#31315=CARTESIAN_POINT('Ctrl Pts',(-3.38957866884684,0.198868156207286,
-32.8694959947181));
#31316=CARTESIAN_POINT('Ctrl Pts',(-3.37242232301567,0.394398350512979,
-32.8798156181844));
#31317=CARTESIAN_POINT('Ctrl Pts',(-3.33313537108559,0.617709245412695,
-32.8925278884542));
#31318=CARTESIAN_POINT('Ctrl Pts',(-3.32737786332044,0.648006592528334,
-32.894273105052));
#31319=CARTESIAN_POINT('Ctrl Pts',(-3.31596013979505,0.703918576631977,
-32.8975387115144));
#31320=CARTESIAN_POINT('Ctrl Pts',(-3.31041437408373,0.729554379380284,
-32.8990536090901));
#31321=CARTESIAN_POINT('Ctrl Pts',(-3.30055880730922,0.772684379337358,
-32.9016359558564));
#31322=CARTESIAN_POINT('Ctrl Pts',(-3.29640589675622,0.790213733915254,
-32.9026949915034));
#31323=CARTESIAN_POINT('Ctrl Pts',(-3.28728614573419,0.827384602266697,
-32.9049621111853));
#31324=CARTESIAN_POINT('Ctrl Pts',(-3.28228271071418,0.847015729224043,
-32.9061720128739));
#31325=CARTESIAN_POINT('Ctrl Pts',(-3.26755553328994,0.902707482043506,
-32.909637894282));
#31326=CARTESIAN_POINT('Ctrl Pts',(-3.25741163036675,0.938652856744965,
-32.9119150157372));
#31327=CARTESIAN_POINT('Ctrl Pts',(-3.19363817663677,1.15113968372738,-32.9255861175308));
#31328=CARTESIAN_POINT('Ctrl Pts',(-3.12626398020651,1.323220216345,-32.9375076425619));
#31329=CARTESIAN_POINT('Ctrl Pts',(-2.97822509841098,1.62599209145817,-32.9592094683079));
#31330=CARTESIAN_POINT('Ctrl Pts',(-2.90204073986036,1.75836319971557,-32.9689816557687));
#31331=CARTESIAN_POINT('Ctrl Pts',(-2.76374814515095,1.96502839308152,-32.9845064626342));
#31332=CARTESIAN_POINT('Ctrl Pts',(-2.70692753078343,2.04259305868081,-32.9904039982188));
#31333=CARTESIAN_POINT('Ctrl Pts',(-2.6211770957806,2.14977413477992,-32.9986532948203));
#31334=CARTESIAN_POINT('Ctrl Pts',(-2.59488759754773,2.18143456846072,-33.001103614409));
#31335=CARTESIAN_POINT('Ctrl Pts',(-2.5474927236205,2.23644261433742,-33.0053870409631));
#31336=CARTESIAN_POINT('Ctrl Pts',(-2.52662691652593,2.25998921840134,-33.0072294053604));
#31337=CARTESIAN_POINT('Ctrl Pts',(-2.48188991857644,2.30907978787897,-33.011090907111));
#31338=CARTESIAN_POINT('Ctrl Pts',(-2.45794517609485,2.33455192203991,-33.0131066939468));
#31339=CARTESIAN_POINT('Ctrl Pts',(-2.39171888237064,2.40285399489646,-33.0185493776631));
#31340=CARTESIAN_POINT('Ctrl Pts',(-2.34868305766029,2.44493661133928,-33.0219439673234));
#31341=CARTESIAN_POINT('Ctrl Pts',(-2.1133402605214,2.66311472301906,-33.0398233995884));
#31342=CARTESIAN_POINT('Ctrl Pts',(-1.90232570433707,2.81772074200772,-33.0534249805982));
#31343=CARTESIAN_POINT('Ctrl Pts',(-1.56015434101048,3.01230504697545,-33.0744304859596));
#31344=CARTESIAN_POINT('Ctrl Pts',(-1.44088863834648,3.07113937230117,-33.0816020837599));
#31345=CARTESIAN_POINT('Ctrl Pts',(-1.28445919895993,3.13718570874788,-33.0911835336884));
#31346=CARTESIAN_POINT('Ctrl Pts',(-1.25019721851796,3.15099607866703,-33.0932926378725));
#31347=CARTESIAN_POINT('Ctrl Pts',(-1.19688439897962,3.17147912762038,-33.0966005732746));
#31348=CARTESIAN_POINT('Ctrl Pts',(-1.1779871932423,3.17854656245025,-33.0977781059149));
#31349=CARTESIAN_POINT('Ctrl Pts',(-1.14207033862947,3.19161496064862,-33.1000276191938));
#31350=CARTESIAN_POINT('Ctrl Pts',(-1.1250640855269,3.19764936499773,-33.1010977309092));
#31351=CARTESIAN_POINT('Ctrl Pts',(-1.08304309323718,3.21218316602493,-33.1037530954693));
#31352=CARTESIAN_POINT('Ctrl Pts',(-1.05797590562231,3.22052634247081,-33.1053467502759));
#31353=CARTESIAN_POINT('Ctrl Pts',(-0.964746968840573,3.25035008771109,
-33.1113027622695));
#31354=CARTESIAN_POINT('Ctrl Pts',(-0.896012165114405,3.26996532337549,
-33.115750637736));
#31355=CARTESIAN_POINT('Ctrl Pts',(-0.581828885308255,3.34897617773903,
-33.1361875176625));
#31356=CARTESIAN_POINT('Ctrl Pts',(-0.33082662813074,3.38300639984154,-33.1527311279377));
#31357=CARTESIAN_POINT('Ctrl Pts',(0.0435898422567594,3.39166400082765,
-33.1763644577356));
#31358=CARTESIAN_POINT('Ctrl Pts',(0.165612339454509,3.38789943257147,-33.1839172779407));
#31359=CARTESIAN_POINT('Ctrl Pts',(0.331404875001098,3.37380290817119,-33.193953109855));
#31360=CARTESIAN_POINT('Ctrl Pts',(0.375555479367614,3.36917402563424,-33.1966041947997));
#31361=CARTESIAN_POINT('Ctrl Pts',(0.451283049186981,3.35972734719554,-33.2011164399241));
#31362=CARTESIAN_POINT('Ctrl Pts',(0.482905399583395,3.35532810858078,-33.2029901562619));
#31363=CARTESIAN_POINT('Ctrl Pts',(0.54771237002634,3.34537709322387,-33.2068101369835));
#31364=CARTESIAN_POINT('Ctrl Pts',(0.580886005924621,3.33977668437849,-33.2087546740464));
#31365=CARTESIAN_POINT('Ctrl Pts',(0.666645530648735,3.32398216690663,-33.2137566853829));
#31366=CARTESIAN_POINT('Ctrl Pts',(0.719083919677958,3.31303372501736,-33.2167906374287));
#31367=CARTESIAN_POINT('Ctrl Pts',(1.051316999132,3.23540745781591,-33.2358990552825));
#31368=CARTESIAN_POINT('Ctrl Pts',(1.32191154160378,3.13459454853511,-33.2508204427465));
#31369=CARTESIAN_POINT('Ctrl Pts',(1.69197484666758,2.94017527281209,-33.2731970795905));
#31370=CARTESIAN_POINT('Ctrl Pts',(1.80380800333793,2.87292181622552,-33.2802776265961));
#31371=CARTESIAN_POINT('Ctrl Pts',(1.93659994096173,2.7822492796301,-33.2894230377376));
#31372=CARTESIAN_POINT('Ctrl Pts',(1.96148841441477,2.76475920276684,-33.2911710611914));
#31373=CARTESIAN_POINT('Ctrl Pts',(2.00138093772629,2.7359154327832,-33.2940341499721));
#31374=CARTESIAN_POINT('Ctrl Pts',(2.0165322899965,2.72476721995828,-33.2951361834862));
#31375=CARTESIAN_POINT('Ctrl Pts',(2.04674874983643,2.70214419054493,-33.2973652021991));
#31376=CARTESIAN_POINT('Ctrl Pts',(2.06181202094502,2.69066809991932,-33.2984922457848));
#31377=CARTESIAN_POINT('Ctrl Pts',(2.10129022621982,2.6600651045834,-33.30148635143));
#31378=CARTESIAN_POINT('Ctrl Pts',(2.12553964540491,2.64072869561797,-33.3033667417317));
#31379=CARTESIAN_POINT('Ctrl Pts',(2.25679852348598,2.53308401193048,-33.3137577625229));
#31380=CARTESIAN_POINT('Ctrl Pts',(2.35856613850709,2.4386088768473,-33.3225956154495));
#31381=CARTESIAN_POINT('Ctrl Pts',(2.54603097230073,2.24183762419599,-33.3400577281402));
#31382=CARTESIAN_POINT('Ctrl Pts',(2.63206243720546,2.14017722431417,-33.348660850376));
#31383=CARTESIAN_POINT('Ctrl Pts',(2.77530323336927,1.94917069204475,-33.3638871783714));
#31384=CARTESIAN_POINT('Ctrl Pts',(2.83472522296516,1.86169552257456,-33.3705467941004));
#31385=CARTESIAN_POINT('Ctrl Pts',(2.92979231201171,1.70661329945789,-33.3817852073502));
#31386=CARTESIAN_POINT('Ctrl Pts',(2.96741820017876,1.64031781556161,-33.3864235667379));
#31387=CARTESIAN_POINT('Ctrl Pts',(3.02039556579916,1.5391741693539,-33.3932576355401));
#31388=CARTESIAN_POINT('Ctrl Pts',(3.03744570458595,1.50524757563404,-33.3955106928335));
#31389=CARTESIAN_POINT('Ctrl Pts',(3.06746920513162,1.44291792209281,-33.3995807433197));
#31390=CARTESIAN_POINT('Ctrl Pts',(3.08062681348076,1.4146087749619,-33.4014038303834));
#31391=CARTESIAN_POINT('Ctrl Pts',(3.10858143611425,1.35222274311065,-33.4053678223855));
#31392=CARTESIAN_POINT('Ctrl Pts',(3.1232132044165,1.31807599436185,-33.4075030335856));
#31393=CARTESIAN_POINT('Ctrl Pts',(3.16357460837197,1.21943487838255,-33.4135782327898));
#31394=CARTESIAN_POINT('Ctrl Pts',(3.18788863150178,1.15437978807924,-33.4174722390013));
#31395=CARTESIAN_POINT('Ctrl Pts',(3.28990248112387,0.853555334395103,-33.4350461858672));
#31396=CARTESIAN_POINT('Ctrl Pts',(3.34355605048408,0.610452166633055,-33.4479886636889));
#31397=CARTESIAN_POINT('Ctrl Pts',(3.38402099983914,0.23545043532618,-33.4681352554235));
#31398=CARTESIAN_POINT('Ctrl Pts',(3.39052704336033,0.106562978730718,-33.4751066392919));
#31399=CARTESIAN_POINT('Ctrl Pts',(3.38943548683829,-0.0588438593883352,
-33.4844451816288));
#31400=CARTESIAN_POINT('Ctrl Pts',(3.38860607986942,-0.0953107055720004,
-33.4865286472478));
#31401=CARTESIAN_POINT('Ctrl Pts',(3.38640792825984,-0.151821088923058,
-33.4898050306639));
#31402=CARTESIAN_POINT('Ctrl Pts',(3.38544914787157,-0.171878803259563,
-33.4909772908814));
#31403=CARTESIAN_POINT('Ctrl Pts',(3.38330002324623,-0.209775173124198,
-33.4932117517844));
#31404=CARTESIAN_POINT('Ctrl Pts',(3.38214667163084,-0.227614820294416,
-33.4942720210313));
#31405=CARTESIAN_POINT('Ctrl Pts',(3.37924351783717,-0.26760413441439,-33.4966666046545));
#31406=CARTESIAN_POINT('Ctrl Pts',(3.37741693247253,-0.289747360750057,
-33.4980048174597));
#31407=CARTESIAN_POINT('Ctrl Pts',(3.37009055105826,-0.369040780045293,
-33.5028370649734));
#31408=CARTESIAN_POINT('Ctrl Pts',(3.36335690972538,-0.426064475356408,
-33.5063870217699));
#31409=CARTESIAN_POINT('Ctrl Pts',(3.31703629659566,-0.747908371550464,
-33.5267500540963));
#31410=CARTESIAN_POINT('Ctrl Pts',(3.24762896243497,-1.00747945967103,-33.5443411831996));
#31411=CARTESIAN_POINT('Ctrl Pts',(3.10230691174956,-1.37170118010862,-33.5691078137422));
#31412=CARTESIAN_POINT('Ctrl Pts',(3.04989263227307,-1.48459852164717,-33.5768141087772));
#31413=CARTESIAN_POINT('Ctrl Pts',(2.97038993195384,-1.63376294591257,-33.5870117226861));
#31414=CARTESIAN_POINT('Ctrl Pts',(2.9486171303427,-1.67273877620257,-33.5896784474023));
#31415=CARTESIAN_POINT('Ctrl Pts',(2.90994236706701,-1.73886811106582,-33.594208789621));
#31416=CARTESIAN_POINT('Ctrl Pts',(2.89341481812748,-1.76623262374934,-33.5960852266785));
#31417=CARTESIAN_POINT('Ctrl Pts',(2.85874643571015,-1.82183979749035,-33.5999035726923));
#31418=CARTESIAN_POINT('Ctrl Pts',(2.84056822242917,-1.85005505907499,-33.6018438621193));
#31419=CARTESIAN_POINT('Ctrl Pts',(2.79252068678727,-1.92225374287121,-33.6068194048722));
#31420=CARTESIAN_POINT('Ctrl Pts',(2.76202980001436,-1.96581358477319,-33.6098316299965));
#31421=CARTESIAN_POINT('Ctrl Pts',(2.55895521573008,-2.24187121186073,-33.6290318828746));
#31422=CARTESIAN_POINT('Ctrl Pts',(2.35822015009203,-2.45215008703459,-33.644046316049));
#31423=CARTESIAN_POINT('Ctrl Pts',(2.03266072350545,-2.71577441501087,-33.66647647633));
#31424=CARTESIAN_POINT('Ctrl Pts',(1.92755529004081,-2.79135533015354,-33.6735037019972));
#31425=CARTESIAN_POINT('Ctrl Pts',(1.79276813939869,-2.87703144063635,-33.6825880708323));
#31426=CARTESIAN_POINT('Ctrl Pts',(1.76691930133804,-2.89297831983318,-33.6843334691911));
#31427=CARTESIAN_POINT('Ctrl Pts',(1.72472846438684,-2.91823067344946,-33.6871933323607));
#31428=CARTESIAN_POINT('Ctrl Pts',(1.7085166108802,-2.92775161114048,-33.6882948200472));
#31429=CARTESIAN_POINT('Ctrl Pts',(1.67580924936994,-2.94659590525321,-33.6905239381613));
#31430=CARTESIAN_POINT('Ctrl Pts',(1.65931313132667,-2.95591677207997,-33.6916516428141));
#31431=CARTESIAN_POINT('Ctrl Pts',(1.61556752419028,-2.98015295310937,-33.6946494479529));
#31432=CARTESIAN_POINT('Ctrl Pts',(1.58819023387242,-2.99483249650858,-33.6965329324586));
#31433=CARTESIAN_POINT('Ctrl Pts',(1.43417981086195,-3.07470638109278,-33.7071533340132));
#31434=CARTESIAN_POINT('Ctrl Pts',(1.30374680507852,-3.13224013398883,-33.7162352510922));
#31435=CARTESIAN_POINT('Ctrl Pts',(0.991988016320563,-3.24690288187274,
-33.7375873191414));
#31436=CARTESIAN_POINT('Ctrl Pts',(0.808679744261229,-3.29734214961956,
-33.7498625336535));
#31437=CARTESIAN_POINT('Ctrl Pts',(0.515875549986654,-3.35200771303694,
-33.7685575933023));
#31438=CARTESIAN_POINT('Ctrl Pts',(0.408750135695405,-3.36675070969322,
-33.775218007896));
#31439=CARTESIAN_POINT('Ctrl Pts',(0.258499667809446,-3.38014965848058,
-33.7843004630683));
#31440=CARTESIAN_POINT('Ctrl Pts',(0.215835624946258,-3.3831418865376,-33.7868509298278));
#31441=CARTESIAN_POINT('Ctrl Pts',(0.141492719894735,-3.38694376729331,
-33.7912475597717));
#31442=CARTESIAN_POINT('Ctrl Pts',(0.109838688705697,-3.38811803745276,
-33.7931046085018));
#31443=CARTESIAN_POINT('Ctrl Pts',(0.0439598811176838,-3.38963769235233,
-33.7969400305457));
#31444=CARTESIAN_POINT('Ctrl Pts',(0.00973688866917836,-3.3899087705436,
-33.7989159259696));
#31445=CARTESIAN_POINT('Ctrl Pts',(-0.080960575403858,-3.3892536161392,
-33.804112141181));
#31446=CARTESIAN_POINT('Ctrl Pts',(-0.13741891611573,-3.38743431493963,
-33.8073052006884));
#31447=CARTESIAN_POINT('Ctrl Pts',(-0.418287936822755,-3.3713494130525,
-33.8230238930198));
#31448=CARTESIAN_POINT('Ctrl Pts',(-0.640934407026466,-3.33619167029793,
-33.8349084265437));
#31449=CARTESIAN_POINT('Ctrl Pts',(-0.981118889564493,-3.24713465271878,
-33.853576931239));
#31450=CARTESIAN_POINT('Ctrl Pts',(-1.10185977840245,-3.20817383771495,
-33.8603209193196));
#31451=CARTESIAN_POINT('Ctrl Pts',(-1.28603381854589,-3.1371184567035,-33.8711575933531));
#31452=CARTESIAN_POINT('Ctrl Pts',(-1.35112460440021,-3.10963923367563,
-33.8751001673527));
#31453=CARTESIAN_POINT('Ctrl Pts',(-1.43860594519594,-3.06944222389113,
-33.8806147491272));
#31454=CARTESIAN_POINT('Ctrl Pts',(-1.46178395586088,-3.05847187539271,
-33.8820970073651));
#31455=CARTESIAN_POINT('Ctrl Pts',(-1.50094949792565,-3.03938760602815,
-33.8846415242646));
#31456=CARTESIAN_POINT('Ctrl Pts',(-1.51700096358366,-3.03140800314464,
-33.8856959474534));
#31457=CARTESIAN_POINT('Ctrl Pts',(-1.55130389997304,-3.01401442373805,
-33.8879753911136));
#31458=CARTESIAN_POINT('Ctrl Pts',(-1.56953342889787,-3.00456178252967,
-33.8892025200976));
#31459=CARTESIAN_POINT('Ctrl Pts',(-1.62091720148741,-2.97732229379212,
-33.8927039224996));
#31460=CARTESIAN_POINT('Ctrl Pts',(-1.65386183810675,-2.95914876028468,
-33.8949994256224));
#31461=CARTESIAN_POINT('Ctrl Pts',(-1.81284582266028,-2.86796289152058,
-33.9063011959732));
#31462=CARTESIAN_POINT('Ctrl Pts',(-1.934384475333,-2.78743097472684,-33.9156309140578));
#31463=CARTESIAN_POINT('Ctrl Pts',(-2.15239428135991,-2.62183569639369,
-33.9332521156799));
#31464=CARTESIAN_POINT('Ctrl Pts',(-2.24995789486095,-2.5386049520326,-33.941520479365));
#31465=CARTESIAN_POINT('Ctrl Pts',(-2.4473319423018,-2.34988871627047,-33.9588792498742));
#31466=CARTESIAN_POINT('Ctrl Pts',(-2.54556462969428,-2.24310495068206,
-33.9679153428951));
#31467=CARTESIAN_POINT('Ctrl Pts',(-2.66590769863997,-2.09415990671961,
-33.9794897570944));
#31468=CARTESIAN_POINT('Ctrl Pts',(-2.69439960228897,-2.05737227460727,
-33.9822734032208));
#31469=CARTESIAN_POINT('Ctrl Pts',(-2.74136944304887,-1.99407657726352,
-33.9869398289304));
#31470=CARTESIAN_POINT('Ctrl Pts',(-2.76024156809812,-1.96787052723638,
-33.9888374327708));
#31471=CARTESIAN_POINT('Ctrl Pts',(-2.79766495426263,-1.91430617016825,
-33.9926487411673));
#31472=CARTESIAN_POINT('Ctrl Pts',(-2.81619630786475,-1.8869382015794,-33.994561572194));
#31473=CARTESIAN_POINT('Ctrl Pts',(-2.86205476548722,-1.81703147911282,
-33.9993640824283));
#31474=CARTESIAN_POINT('Ctrl Pts',(-2.88883639316144,-1.77414360803328,
-34.0022338772806));
#31475=CARTESIAN_POINT('Ctrl Pts',(-3.05520077975636,-1.49396679694007,
-34.020531227001));
#31476=CARTESIAN_POINT('Ctrl Pts',(-3.16639252441545,-1.24103021760397,
-34.0348996042033));
#31477=CARTESIAN_POINT('Ctrl Pts',(-3.28831183410698,-0.836165232795949,
-34.0574463648084));
#31478=CARTESIAN_POINT('Ctrl Pts',(-3.32157799672088,-0.692298984761503,
-34.0654022834829));
#31479=CARTESIAN_POINT('Ctrl Pts',(-3.35037701063691,-0.516085070735116,
-34.0755489351574));
#31480=CARTESIAN_POINT('Ctrl Pts',(-3.35496528964148,-0.485363446006798,
-34.0773326563309));
#31481=CARTESIAN_POINT('Ctrl Pts',(-3.36167147105276,-0.43580841250091,
-34.0802396765024));
#31482=CARTESIAN_POINT('Ctrl Pts',(-3.36405483759344,-0.417012066758022,
-34.0813491957314));
#31483=CARTESIAN_POINT('Ctrl Pts',(-3.36822372475534,-0.381769120537876,
-34.0834440356721));
#31484=CARTESIAN_POINT('Ctrl Pts',(-3.37004667018608,-0.365327433925368,
-34.0844272409039));
#31485=CARTESIAN_POINT('Ctrl Pts',(-3.37464780142137,-0.320858992556897,
-34.087101199132));
#31486=CARTESIAN_POINT('Ctrl Pts',(-3.37719709385888,-0.29281043892541,
-34.0888036252799));
#31487=CARTESIAN_POINT('Ctrl Pts',(-3.38624523605637,-0.177308788198433,
-34.0958702750957));
#31488=CARTESIAN_POINT('Ctrl Pts',(-3.38969829837649,-0.0896566665961387,
-34.1013646723238));
#31489=CARTESIAN_POINT('Ctrl Pts',(-3.38986499262025,0.19622356003253,-34.1195194495297));
#31490=CARTESIAN_POINT('Ctrl Pts',(-3.37259756120772,0.394052114179757,
-34.1324249634223));
#31491=CARTESIAN_POINT('Ctrl Pts',(-3.31234492261008,0.735392055258899,
-34.1544906165657));
#31492=CARTESIAN_POINT('Ctrl Pts',(-3.2769745204564,0.879702997720911,-34.1637602107885));
#31493=CARTESIAN_POINT('Ctrl Pts',(-3.21785727187418,1.06680971605334,-34.1756353193021));
#31494=CARTESIAN_POINT('Ctrl Pts',(-3.20249875485041,1.11206585444116,-34.1784971490572));
#31495=CARTESIAN_POINT('Ctrl Pts',(-3.17619591121179,1.1845005706199,-34.1830627896972));
#31496=CARTESIAN_POINT('Ctrl Pts',(-3.16584766920085,1.21188724039255,-34.1847855454195));
#31497=CARTESIAN_POINT('Ctrl Pts',(-3.14337838573098,1.26909952519826,-34.1883783677504));
#31498=CARTESIAN_POINT('Ctrl Pts',(-3.13118458828062,1.29889355165416,-34.1902458352731));
#31499=CARTESIAN_POINT('Ctrl Pts',(-3.10055815166929,1.37078658483829,-34.1947458834263));
#31500=CARTESIAN_POINT('Ctrl Pts',(-3.08169000842965,1.41269377036442,-34.1973637612878));
#31501=CARTESIAN_POINT('Ctrl Pts',(-3.00273330698203,1.57894495535171,-34.2077440297647));
#31502=CARTESIAN_POINT('Ctrl Pts',(-2.93592171848532,1.6999539588631,-34.2152809706273));
#31503=CARTESIAN_POINT('Ctrl Pts',(-2.78756965916299,1.9336760536422,-34.2301414609723));
#31504=CARTESIAN_POINT('Ctrl Pts',(-2.70611237850348,2.04611921764427,-34.2374503637462));
#31505=CARTESIAN_POINT('Ctrl Pts',(-2.526915263411,2.26399257682621,-34.252472741218));
#31506=CARTESIAN_POINT('Ctrl Pts',(-2.42890958920908,2.36882966747253,-34.2601777563289));
#31507=CARTESIAN_POINT('Ctrl Pts',(-2.29725315033719,2.49287824440455,-34.2703734605083));
#31508=CARTESIAN_POINT('Ctrl Pts',(-2.26950943323998,2.51816216103339,-34.2725143350504));
#31509=CARTESIAN_POINT('Ctrl Pts',(-2.22596178515698,2.55654456245038,-34.2758735158974));
#31510=CARTESIAN_POINT('Ctrl Pts',(-2.21044833637498,2.56996966414165,-34.2770699622021));
#31511=CARTESIAN_POINT('Ctrl Pts',(-2.18114871188186,2.59486356512339,-34.2793312869031));
#31512=CARTESIAN_POINT('Ctrl Pts',(-2.16739192096898,2.60636506081742,-34.2803938766907));
#31513=CARTESIAN_POINT('Ctrl Pts',(-2.13371275474353,2.63407183731994,-34.2829964885894));
#31514=CARTESIAN_POINT('Ctrl Pts',(-2.11369650202648,2.65016066944794,-34.284544145777));
#31515=CARTESIAN_POINT('Ctrl Pts',(-2.03770255909218,2.70983513744212,-34.2904171095247));
#31516=CARTESIAN_POINT('Ctrl Pts',(-1.98054695187105,2.75188491476045,-34.29482813212));
#31517=CARTESIAN_POINT('Ctrl Pts',(-1.81691705377377,2.86452958928056,-34.3073497153043));
#31518=CARTESIAN_POINT('Ctrl Pts',(-1.70771047857385,2.93094521640858,-34.3155823397102));
#31519=CARTESIAN_POINT('Ctrl Pts',(-1.39794646147904,3.09613213965208,-34.3381927643107));
#31520=CARTESIAN_POINT('Ctrl Pts',(-1.19094028928378,3.18150530386029,-34.3524638279715));
#31521=CARTESIAN_POINT('Ctrl Pts',(-0.922863179302594,3.26219663220974,
-34.3695336105765));
#31522=CARTESIAN_POINT('Ctrl Pts',(-0.868308411390444,3.27713966571272,
-34.3729408330519));
#31523=CARTESIAN_POINT('Ctrl Pts',(-0.780166540973884,3.29892669935651,
-34.3783420690312));
#31524=CARTESIAN_POINT('Ctrl Pts',(-0.746806930282671,3.30663828323955,
-34.3803628507207));
#31525=CARTESIAN_POINT('Ctrl Pts',(-0.682376401614594,3.32050754739192,
-34.3842223758094));
#31526=CARTESIAN_POINT('Ctrl Pts',(-0.651324929650731,3.32673772049028,
-34.3860632055121));
#31527=CARTESIAN_POINT('Ctrl Pts',(-0.578185287944982,3.34034913326486,
-34.3903563437231));
#31528=CARTESIAN_POINT('Ctrl Pts',(-0.536035371616945,3.34737163616403,
-34.3927973378157));
#31529=CARTESIAN_POINT('Ctrl Pts',(-0.387144033458921,3.36929347115258,
-34.4013145772699));
#31530=CARTESIAN_POINT('Ctrl Pts',(-0.279832129318265,3.37989879741465,
-34.407261111356));
#31531=CARTESIAN_POINT('Ctrl Pts',(0.0162888364614813,3.39496036038646,
-34.4233481261632));
#31532=CARTESIAN_POINT('Ctrl Pts',(0.205236842147306,3.38879035950003,-34.4332410926898));
#31533=CARTESIAN_POINT('Ctrl Pts',(0.535591867762952,3.35026039985449,-34.4509882791587));
#31534=CARTESIAN_POINT('Ctrl Pts',(0.677272857068071,3.32451450141487,-34.4587575406116));
#31535=CARTESIAN_POINT('Ctrl Pts',(0.847033040975952,3.28236282430959,-34.4686973678093));
#31536=CARTESIAN_POINT('Ctrl Pts',(0.877086165916422,3.27446032134965,-34.4704817761839));
#31537=CARTESIAN_POINT('Ctrl Pts',(0.925283917335664,3.26107556237097,-34.473389642628));
#31538=CARTESIAN_POINT('Ctrl Pts',(0.943499255967374,3.25585215690295,-34.4744993064328));
#31539=CARTESIAN_POINT('Ctrl Pts',(0.979696012736823,3.24514316926176,-34.4767274766792));
#31540=CARTESIAN_POINT('Ctrl Pts',(0.997677465724576,3.2396601827859,-34.4778458218761));
#31541=CARTESIAN_POINT('Ctrl Pts',(1.04457920921106,3.2249311928968,-34.4807911841795));
#31542=CARTESIAN_POINT('Ctrl Pts',(1.0734219563561,3.21544586144648,-34.4826308044277));
#31543=CARTESIAN_POINT('Ctrl Pts',(1.2242683493533,3.16358225111707,-34.4923874122592));
#31544=CARTESIAN_POINT('Ctrl Pts',(1.34389454423919,3.1146472177287,-34.5005897915081));
#31545=CARTESIAN_POINT('Ctrl Pts',(1.72202210299792,2.93412253094872,-34.5274727874733));
#31546=CARTESIAN_POINT('Ctrl Pts',(1.96657109824326,2.77616427900633,-34.5462559396613));
#31547=CARTESIAN_POINT('Ctrl Pts',(2.2285851371409,2.55472714592498,-34.5671144135563));
#31548=CARTESIAN_POINT('Ctrl Pts',(2.26831695113063,2.51951606195062,-34.5703053172204));
#31549=CARTESIAN_POINT('Ctrl Pts',(2.33178286696648,2.46055258032382,-34.5754511906831));
#31550=CARTESIAN_POINT('Ctrl Pts',(2.35601892117614,2.43735621165582,-34.5774285298408));
#31551=CARTESIAN_POINT('Ctrl Pts',(2.40267621904569,2.39135410105182,-34.5812610067906));
#31552=CARTESIAN_POINT('Ctrl Pts',(2.42512687988977,2.36858336741602,-34.5831173338275));
#31553=CARTESIAN_POINT('Ctrl Pts',(2.47817683671519,2.31323194349525,-34.587535821545));
#31554=CARTESIAN_POINT('Ctrl Pts',(2.50846091470029,2.28035667389836,-34.5900846240504));
#31555=CARTESIAN_POINT('Ctrl Pts',(2.6208639491699,2.15338625817068,-34.5996611177607));
#31556=CARTESIAN_POINT('Ctrl Pts',(2.69841485700287,2.05537385074105,-34.6065084660344));
#31557=CARTESIAN_POINT('Ctrl Pts',(2.92675341583585,1.73151851596639,-34.627868749138));
#31558=CARTESIAN_POINT('Ctrl Pts',(3.05590866610436,1.49179038285107,-34.641812778129));
#31559=CARTESIAN_POINT('Ctrl Pts',(3.17497918389823,1.18864186072428,-34.6598756371091));
#31560=CARTESIAN_POINT('Ctrl Pts',(3.19363812211422,1.13755755074913,-34.6629360347239));
#31561=CARTESIAN_POINT('Ctrl Pts',(3.21803978615924,1.06541057383332,-34.6673097554696));
#31562=CARTESIAN_POINT('Ctrl Pts',(3.22482098102185,1.04470538611959,-34.6685708116522));
#31563=CARTESIAN_POINT('Ctrl Pts',(3.23682770593384,1.00681383645763,-34.6708916776225));
#31564=CARTESIAN_POINT('Ctrl Pts',(3.24211717801349,0.98964836873316,-34.6719479791831));
#31565=CARTESIAN_POINT('Ctrl Pts',(3.25312675478436,0.952884133955721,-34.6742219621565));
#31566=CARTESIAN_POINT('Ctrl Pts',(3.25880653168419,0.933274770969195,-34.6754416485859));
#31567=CARTESIAN_POINT('Ctrl Pts',(3.27458375400896,0.876903459717626,-34.6789649282103));
#31568=CARTESIAN_POINT('Ctrl Pts',(3.28423831468145,0.840021947107023,-34.681290714281));
#31569=CARTESIAN_POINT('Ctrl Pts',(3.32723231452811,0.663691881831474,-34.6924832295635));
#31570=CARTESIAN_POINT('Ctrl Pts',(3.35232188866183,0.522392143099672,-34.7016620793814));
#31571=CARTESIAN_POINT('Ctrl Pts',(3.39787408297614,0.118546318921703,-34.7278167189869));
#31572=CARTESIAN_POINT('Ctrl Pts',(3.39683557008148,-0.14543756773046,-34.7447406300557));
#31573=CARTESIAN_POINT('Ctrl Pts',(3.35898735129977,-0.458638414500808,
-34.7639107261228));
#31574=CARTESIAN_POINT('Ctrl Pts',(3.35150412743073,-0.510456423024906,
-34.7670560265971));
#31575=CARTESIAN_POINT('Ctrl Pts',(3.33728503183569,-0.595020379461398,
-34.7721480466641));
#31576=CARTESIAN_POINT('Ctrl Pts',(3.33126001244793,-0.627875372821941,
-34.7741162439637));
#31577=CARTESIAN_POINT('Ctrl Pts',(3.31850249708846,-0.692079408598487,
-34.7779440259821));
#31578=CARTESIAN_POINT('Ctrl Pts',(3.31180890851199,-0.723432503409318,
-34.779804597304));
#31579=CARTESIAN_POINT('Ctrl Pts',(3.29461194556609,-0.798735684208286,
-34.7842547468235));
#31580=CARTESIAN_POINT('Ctrl Pts',(3.2836724861106,-0.84258046477976,-34.7868304467869));
#31581=CARTESIAN_POINT('Ctrl Pts',(3.2379347793336,-1.01144550313212,-34.7967053535089));
#31582=CARTESIAN_POINT('Ctrl Pts',(3.19684449558154,-1.13465127065709,-34.8038081690403));
#31583=CARTESIAN_POINT('Ctrl Pts',(3.09611256668366,-1.38734538738263,-34.8184482761359));
#31584=CARTESIAN_POINT('Ctrl Pts',(3.03517161476951,-1.51603900686257,-34.8259464623072));
#31585=CARTESIAN_POINT('Ctrl Pts',(2.89397856132622,-1.77133848810336,-34.8414679968559));
#31586=CARTESIAN_POINT('Ctrl Pts',(2.81306310590148,-1.89721369027721,-34.8494831617403));
#31587=CARTESIAN_POINT('Ctrl Pts',(2.7016094239725,-2.0477162012003,-34.8600356287492));
#31588=CARTESIAN_POINT('Ctrl Pts',(2.67859808864502,-2.07772643857734,-34.8621919721336));
#31589=CARTESIAN_POINT('Ctrl Pts',(2.64229922340208,-2.12346020036185,-34.8655703170097));
#31590=CARTESIAN_POINT('Ctrl Pts',(2.62936178248234,-2.13945903877328,-34.8667700653561));
#31591=CARTESIAN_POINT('Ctrl Pts',(2.6048886661817,-2.1691659810227,-34.8690336274041));
#31592=CARTESIAN_POINT('Ctrl Pts',(2.59338873263631,-2.18290193153236,-34.8700950808327));
#31593=CARTESIAN_POINT('Ctrl Pts',(2.56521653358994,-2.21601503265293,-34.8726892958089));
#31594=CARTESIAN_POINT('Ctrl Pts',(2.54843315455329,-2.23529569848921,-34.8742295695073));
#31595=CARTESIAN_POINT('Ctrl Pts',(2.48488437643595,-2.30665422771724,-34.8800364518458));
#31596=CARTESIAN_POINT('Ctrl Pts',(2.43673010987006,-2.35746667650125,-34.8843864222713));
#31597=CARTESIAN_POINT('Ctrl Pts',(2.29844416648062,-2.49462027990646,-34.8966572761193));
#31598=CARTESIAN_POINT('Ctrl Pts',(2.20506598488657,-2.57752934795268,-34.9046953315908));
#31599=CARTESIAN_POINT('Ctrl Pts',(1.92872128571085,-2.7968623166099,-34.9274196290776));
#31600=CARTESIAN_POINT('Ctrl Pts',(1.73623457465289,-2.92026059402176,-34.9420035506775));
#31601=CARTESIAN_POINT('Ctrl Pts',(1.48259538617798,-3.04884948356767,-34.9593387994373));
#31602=CARTESIAN_POINT('Ctrl Pts',(1.43177182244399,-3.07304446174398,-34.9627288631305));
#31603=CARTESIAN_POINT('Ctrl Pts',(1.34914788102612,-3.10988318747088,-34.968109859079));
#31604=CARTESIAN_POINT('Ctrl Pts',(1.31771919912988,-3.12332990318589,-34.9701272002548));
#31605=CARTESIAN_POINT('Ctrl Pts',(1.25677293888865,-3.14832192936303,-34.9739843424391));
#31606=CARTESIAN_POINT('Ctrl Pts',(1.22728642329919,-3.15993312038952,-34.9758261619595));
#31607=CARTESIAN_POINT('Ctrl Pts',(1.15754195820792,-3.18627351746299,-34.980127961157));
#31608=CARTESIAN_POINT('Ctrl Pts',(1.11715841451135,-3.20065612383089,-34.9825764855907));
#31609=CARTESIAN_POINT('Ctrl Pts',(0.973288417892133,-3.24884054868211,
-34.9911618952961));
#31610=CARTESIAN_POINT('Ctrl Pts',(0.868454568037573,-3.27842109829037,
-34.9971660981783));
#31611=CARTESIAN_POINT('Ctrl Pts',(0.606095365092284,-3.33897841490783,
-35.0117682317079));
#31612=CARTESIAN_POINT('Ctrl Pts',(0.447452281209644,-3.36391391680284,
-35.0202244245797));
#31613=CARTESIAN_POINT('Ctrl Pts',(0.118544636904989,-3.39192463404747,
-35.0377696114158));
#31614=CARTESIAN_POINT('Ctrl Pts',(-0.0513757646744192,-3.39360483469187,
-35.0468449935368));
#31615=CARTESIAN_POINT('Ctrl Pts',(-0.252244515554937,-3.38049965355785,
-35.0582757641332));
#31616=CARTESIAN_POINT('Ctrl Pts',(-0.283770878104262,-3.37799928072184,
-35.0600907254119));
#31617=CARTESIAN_POINT('Ctrl Pts',(-0.334240136233976,-3.37328506345338,
-35.0630362274157));
#31618=CARTESIAN_POINT('Ctrl Pts',(-0.35320804733597,-3.37135175042932,
-35.0641523236043));
#31619=CARTESIAN_POINT('Ctrl Pts',(-0.390739298204573,-3.36720616167878,
-35.0663804760888));
#31620=CARTESIAN_POINT('Ctrl Pts',(-0.409302557241863,-3.36500013460346,
-35.0674921892218));
#31621=CARTESIAN_POINT('Ctrl Pts',(-0.457465896708807,-3.35887206601575,
-35.0704000266512));
#31622=CARTESIAN_POINT('Ctrl Pts',(-0.487033599472257,-3.35471231893777,
-35.0722082031989));
#31623=CARTESIAN_POINT('Ctrl Pts',(-0.634443566264481,-3.33198406586412,
-35.0813254680643));
#31624=CARTESIAN_POINT('Ctrl Pts',(-0.75129431770149,-3.30759556292489,
-35.0888785579196));
#31625=CARTESIAN_POINT('Ctrl Pts',(-1.1131567996652,-3.2119037072286,-35.1128495592457));
#31626=CARTESIAN_POINT('Ctrl Pts',(-1.3515992252719,-3.11907870056493,-35.1294288132987));
#31627=CARTESIAN_POINT('Ctrl Pts',(-1.6480641028837,-2.96321896690237,-35.1501657119898));
#31628=CARTESIAN_POINT('Ctrl Pts',(-1.71741537342769,-2.92357109233622,
-35.1550342867275));
#31629=CARTESIAN_POINT('Ctrl Pts',(-1.818116873072,-2.86117911333031,-35.1621309962846));
#31630=CARTESIAN_POINT('Ctrl Pts',(-1.85057918786169,-2.84029078366784,
-35.1644232613473));
#31631=CARTESIAN_POINT('Ctrl Pts',(-1.90865493207414,-2.80150266354938,
-35.1685342756865));
#31632=CARTESIAN_POINT('Ctrl Pts',(-1.9343907301161,-2.78379478822542,-35.1703597491713));
#31633=CARTESIAN_POINT('Ctrl Pts',(-1.98974337551054,-2.74457029965302,
-35.1742958737963));
#31634=CARTESIAN_POINT('Ctrl Pts',(-2.01926406716062,-2.72292445838318,
-35.1764013914196));
#31635=CARTESIAN_POINT('Ctrl Pts',(-2.10317144685449,-2.65928477105043,
-35.1824093302879));
#31636=CARTESIAN_POINT('Ctrl Pts',(-2.1566409619468,-2.61610899317284,-35.1862664841598));
#31637=CARTESIAN_POINT('Ctrl Pts',(-2.27780629553214,-2.51202860981317,
-35.1951125434662));
#31638=CARTESIAN_POINT('Ctrl Pts',(-2.34443480454401,-2.44996247710945,
-35.2000580986521));
#31639=CARTESIAN_POINT('Ctrl Pts',(-2.50427398751017,-2.2885686365677,-35.2122632748618));
#31640=CARTESIAN_POINT('Ctrl Pts',(-2.59414900486868,-2.18616699521902,
-35.2194410224671));
#31641=CARTESIAN_POINT('Ctrl Pts',(-2.76923251318593,-1.96063116302429,
-35.2346316477654));
#31642=CARTESIAN_POINT('Ctrl Pts',(-2.85293268298594,-1.83670636187101,
-35.2426419561871));
#31643=CARTESIAN_POINT('Ctrl Pts',(-2.94722773916401,-1.67501741597873,
-35.2531887617117));
#31644=CARTESIAN_POINT('Ctrl Pts',(-2.96572714265961,-1.64204048653617,
-35.2553447916394));
#31645=CARTESIAN_POINT('Ctrl Pts',(-2.993434702066,-1.59065302421324,-35.2587227481022));
#31646=CARTESIAN_POINT('Ctrl Pts',(-3.00303377971475,-1.57245554154213,
-35.2599224294812));
#31647=CARTESIAN_POINT('Ctrl Pts',(-3.02068045963614,-1.53825082117741,
-35.2621859450144));
#31648=CARTESIAN_POINT('Ctrl Pts',(-3.02876772364012,-1.52226543320539,
-35.2632474203345));
#31649=CARTESIAN_POINT('Ctrl Pts',(-3.0480871732751,-1.48331493392726,-35.2658418009273));
#31650=CARTESIAN_POINT('Ctrl Pts',(-3.05918682996894,-1.46028574675723,
-35.2673822207929));
#31651=CARTESIAN_POINT('Ctrl Pts',(-3.09970711482363,-1.37372578036355,
-35.2731904068348));
#31652=CARTESIAN_POINT('Ctrl Pts',(-3.12741613132221,-1.3094173233164,-35.2775415810053));
#31653=CARTESIAN_POINT('Ctrl Pts',(-3.19893862914404,-1.12817635351619,
-35.2898173422398));
#31654=CARTESIAN_POINT('Ctrl Pts',(-3.23831293849903,-1.00961238079984,
-35.2978591966103));
#31655=CARTESIAN_POINT('Ctrl Pts',(-3.3316208885491,-0.666346559360019,
-35.3207711574687));
#31656=CARTESIAN_POINT('Ctrl Pts',(-3.36927060381493,-0.437904382366628,
-35.3355340534069));
#31657=CARTESIAN_POINT('Ctrl Pts',(-3.38592720710908,-0.166156663714583,
-35.3521105615618));
#31658=CARTESIAN_POINT('Ctrl Pts',(-3.38770051919659,-0.124885959207531,
-35.3546035224054));
#31659=CARTESIAN_POINT('Ctrl Pts',(-3.3894016571878,-0.0559236771259651,
-35.3587290930678));
#31660=CARTESIAN_POINT('Ctrl Pts',(-3.38974529532265,-0.0282478036078279,
-35.3603740052445));
#31661=CARTESIAN_POINT('Ctrl Pts',(-3.38974995202214,-0.000570320900454691,
-35.3620086083019));
#31662=CARTESIAN_POINT('',(-3.38974881917027,-0.00282938752709428,-37.858982196792));
#31663=CARTESIAN_POINT('Ctrl Pts',(-3.38974995218624,-0.000569344707213824,
-35.3620086659549));
#31664=CARTESIAN_POINT('Ctrl Pts',(-3.38975291771051,0.0170867178207382,
-35.3630514143067));
#31665=CARTESIAN_POINT('Ctrl Pts',(-3.38961793660862,0.0347428412226555,
-35.3640899355741));
#31666=CARTESIAN_POINT('Ctrl Pts',(-3.38899648935759,0.0749413677413,-35.3664450366862));
#31667=CARTESIAN_POINT('Ctrl Pts',(-3.38842305138582,0.0974816613336302,
-35.3677589012831));
#31668=CARTESIAN_POINT('Ctrl Pts',(-3.38633786802073,0.156339478828068,
-35.3711730432985));
#31669=CARTESIAN_POINT('Ctrl Pts',(-3.3844667875467,0.192641891672846,-35.3732622228711));
#31670=CARTESIAN_POINT('Ctrl Pts',(-3.37743126570341,0.296588443641161,
-35.3792016301057));
#31671=CARTESIAN_POINT('Ctrl Pts',(-3.3708196476492,0.364118664350168,-35.3830080450371));
#31672=CARTESIAN_POINT('Ctrl Pts',(-3.32893255581873,0.690566233059449,
-35.4012302280557));
#31673=CARTESIAN_POINT('Ctrl Pts',(-3.26583046453775,0.945001076324621,
-35.4148059003865));
#31674=CARTESIAN_POINT('Ctrl Pts',(-3.12885695894632,1.31045759471189,-35.4357052014358));
#31675=CARTESIAN_POINT('Ctrl Pts',(-3.07673056159079,1.42855442965356,-35.4427134383941));
#31676=CARTESIAN_POINT('Ctrl Pts',(-3.00418794873899,1.57040798658966,-35.4517760667065));
#31677=CARTESIAN_POINT('Ctrl Pts',(-2.99000526293708,1.5972460261098,-35.4535205171969));
#31678=CARTESIAN_POINT('Ctrl Pts',(-2.96645955391385,1.64038901469365,-35.4563792159617));
#31679=CARTESIAN_POINT('Ctrl Pts',(-2.95731761825868,1.65681347058994,-35.4574805068459));
#31680=CARTESIAN_POINT('Ctrl Pts',(-2.93868551465495,1.68964246526695,-35.4597096638239));
#31681=CARTESIAN_POINT('Ctrl Pts',(-2.92919345198542,1.70604510416031,-35.4608376098902));
#31682=CARTESIAN_POINT('Ctrl Pts',(-2.90377139414472,1.74913774743499,-35.4638367621322));
#31683=CARTESIAN_POINT('Ctrl Pts',(-2.88761131132333,1.77568914379793,-35.4657213726169));
#31684=CARTESIAN_POINT('Ctrl Pts',(-2.79371509358002,1.925290908049,-35.4765340046787));
#31685=CARTESIAN_POINT('Ctrl Pts',(-2.70848803534926,2.04344666711543,-35.4858225056777));
#31686=CARTESIAN_POINT('Ctrl Pts',(-2.49671376131709,2.30042887305412,-35.5072343596712));
#31687=CARTESIAN_POINT('Ctrl Pts',(-2.36567915252082,2.43497930434765,-35.5193545716203));
#31688=CARTESIAN_POINT('Ctrl Pts',(-2.14312537729774,2.62848944785032,-35.5378597078768));
#31689=CARTESIAN_POINT('Ctrl Pts',(-2.05875642223739,2.69508233904294,-35.5444785533682));
#31690=CARTESIAN_POINT('Ctrl Pts',(-1.9366388379265,2.7823832883132,-35.5535160555926));
#31691=CARTESIAN_POINT('Ctrl Pts',(-1.90145082295967,2.80654801625459,-35.5560614154846));
#31692=CARTESIAN_POINT('Ctrl Pts',(-1.83938084509652,2.84747003974829,-35.5604522228099));
#31693=CARTESIAN_POINT('Ctrl Pts',(-1.81270361429481,2.86452670223781,-35.5623084719832));
#31694=CARTESIAN_POINT('Ctrl Pts',(-1.75667504342926,2.89925356448393,-35.5661449399777));
#31695=CARTESIAN_POINT('Ctrl Pts',(-1.727286855693,2.9168576723787,-35.5681226397859));
#31696=CARTESIAN_POINT('Ctrl Pts',(-1.64860768004616,2.96238186472672,-35.573329987948));
#31697=CARTESIAN_POINT('Ctrl Pts',(-1.59887414346704,2.98951761661171,-35.5765321555945));
#31698=CARTESIAN_POINT('Ctrl Pts',(-1.35146687251281,3.1165675104746,-35.592069603623));
#31699=CARTESIAN_POINT('Ctrl Pts',(-1.14500893308432,3.19819016642658,-35.6037865171123));
#31700=CARTESIAN_POINT('Ctrl Pts',(-0.80807874034587,3.2945469530148,-35.6223880282357));
#31701=CARTESIAN_POINT('Ctrl Pts',(-0.682192001087079,3.32289654697456,
-35.6292418622242));
#31702=CARTESIAN_POINT('Ctrl Pts',(-0.484632845259992,3.35568541660366,
-35.6402306232104));
#31703=CARTESIAN_POINT('Ctrl Pts',(-0.413914906674825,3.36513992153181,
-35.6442103810439));
#31704=CARTESIAN_POINT('Ctrl Pts',(-0.317359659589477,3.37495924121354,
-35.6497687830793));
#31705=CARTESIAN_POINT('Ctrl Pts',(-0.291734908290365,3.3772707458406,-35.6512558174739));
#31706=CARTESIAN_POINT('Ctrl Pts',(-0.248203797306119,3.3806984094119,-35.6538058378971));
#31707=CARTESIAN_POINT('Ctrl Pts',(-0.230310605959728,3.38196449943124,
-35.6548608984204));
#31708=CARTESIAN_POINT('Ctrl Pts',(-0.191955347339183,3.38437263649069,
-35.6571383839676));
#31709=CARTESIAN_POINT('Ctrl Pts',(-0.171492631767347,3.38547119739737,
-35.6583628673194));
#31710=CARTESIAN_POINT('Ctrl Pts',(-0.11363498725822,3.388051461454,-35.6618493321668));
#31711=CARTESIAN_POINT('Ctrl Pts',(-0.0762247436628929,3.38909946117314,
-35.6641322770748));
#31712=CARTESIAN_POINT('Ctrl Pts',(0.101436125963169,3.39113349095388,-35.6750863124207));
#31713=CARTESIAN_POINT('Ctrl Pts',(0.241633038560804,3.38403356193318,-35.6840573052982));
#31714=CARTESIAN_POINT('Ctrl Pts',(0.558759621458789,3.34816433810946,-35.7045910175322));
#31715=CARTESIAN_POINT('Ctrl Pts',(0.734686026237222,3.31400988494271,-35.7161446332566));
#31716=CARTESIAN_POINT('Ctrl Pts',(1.01182980042781,3.23703870454008,-35.7342023409552));
#31717=CARTESIAN_POINT('Ctrl Pts',(1.11510604435908,3.20293012950349,-35.7409028220947));
#31718=CARTESIAN_POINT('Ctrl Pts',(1.25656151834535,3.14853834176111,-35.7500285574717));
#31719=CARTESIAN_POINT('Ctrl Pts',(1.29625586888896,3.13240506833449,-35.752583909069));
#31720=CARTESIAN_POINT('Ctrl Pts',(1.36475676568306,3.10303850566469,-35.7569861124891));
#31721=CARTESIAN_POINT('Ctrl Pts',(1.39370263897547,3.09014595966006,-35.7588439301141));
#31722=CARTESIAN_POINT('Ctrl Pts',(1.45349798159029,3.06250185589898,-35.7626783760108));
#31723=CARTESIAN_POINT('Ctrl Pts',(1.48431365699262,3.04768553008071,-35.764652565434));
#31724=CARTESIAN_POINT('Ctrl Pts',(1.56528243301119,3.0072359024034,-35.7698382555006));
#31725=CARTESIAN_POINT('Ctrl Pts',(1.61503087642678,2.98081409002974,-35.7730227036185));
#31726=CARTESIAN_POINT('Ctrl Pts',(1.90260353620049,2.818767664648,-35.7914679314374));
#31727=CARTESIAN_POINT('Ctrl Pts',(2.12394099874499,2.6559803891965,-35.8057163167276));
#31728=CARTESIAN_POINT('Ctrl Pts',(2.4239696065906,2.37358174640973,-35.8277296163595));
#31729=CARTESIAN_POINT('Ctrl Pts',(2.51874155615987,2.272763182921,-35.8352129235487));
#31730=CARTESIAN_POINT('Ctrl Pts',(2.62673437512369,2.1428058391625,-35.8448191651196));
#31731=CARTESIAN_POINT('Ctrl Pts',(2.64606098020176,2.11889393095564,-35.8465853068881));
#31732=CARTESIAN_POINT('Ctrl Pts',(2.67672589852464,2.07987979841184,-35.8494706819188));
#31733=CARTESIAN_POINT('Ctrl Pts',(2.68826834238122,2.0649394165042,-35.8505765042623));
#31734=CARTESIAN_POINT('Ctrl Pts',(2.71109427013734,2.03487809512877,-35.8528049736035));
#31735=CARTESIAN_POINT('Ctrl Pts',(2.72237751951488,2.01975780900952,-35.8539275708698));
#31736=CARTESIAN_POINT('Ctrl Pts',(2.7516775638514,1.97980226987503,-35.8568968086561));
#31737=CARTESIAN_POINT('Ctrl Pts',(2.76948402349501,1.95481573140963,-35.8587564049866));
#31738=CARTESIAN_POINT('Ctrl Pts',(2.85973313458692,1.82446713598509,-35.8684573417746));
#31739=CARTESIAN_POINT('Ctrl Pts',(2.92650577685155,1.71531694425535,-35.8765766886657));
#31740=CARTESIAN_POINT('Ctrl Pts',(3.08202248402718,1.42547491934944,-35.8976780570107));
#31741=CARTESIAN_POINT('Ctrl Pts',(3.16114815575196,1.24015890195404,-35.9107186135274));
#31742=CARTESIAN_POINT('Ctrl Pts',(3.25776348113121,0.943254337566089,-35.9303398133329));
#31743=CARTESIAN_POINT('Ctrl Pts',(3.28693308231621,0.835958483269102,-35.9371953042471));
#31744=CARTESIAN_POINT('Ctrl Pts',(3.32003938624461,0.685277151700812,-35.9464880584979));
#31745=CARTESIAN_POINT('Ctrl Pts',(3.32849236888023,0.642965867880995,-35.9490619804585));
#31746=CARTESIAN_POINT('Ctrl Pts',(3.34175655011935,0.569275827759441,-35.9534854182481));
#31747=CARTESIAN_POINT('Ctrl Pts',(3.34693888166077,0.537970289131252,-35.9553462056115));
#31748=CARTESIAN_POINT('Ctrl Pts',(3.35677328294944,0.47290505017467,-35.9591771855472));
#31749=CARTESIAN_POINT('Ctrl Pts',(3.36135738442838,0.43913860602872,-35.9611450849676));
#31750=CARTESIAN_POINT('Ctrl Pts',(3.37209591025473,0.349972375166795,-35.9662919184249));
#31751=CARTESIAN_POINT('Ctrl Pts',(3.37739457745438,0.294478943869608,-35.9694445619635));
#31752=CARTESIAN_POINT('Ctrl Pts',(3.40012405595376,-0.0272575366014145,
-35.9874764569558));
#31753=CARTESIAN_POINT('Ctrl Pts',(3.38744161374581,-0.294674942972111,
-36.0013988635261));
#31754=CARTESIAN_POINT('Ctrl Pts',(3.32136563213738,-0.690708506732728,
-36.0228160547917));
#31755=CARTESIAN_POINT('Ctrl Pts',(3.29130146008207,-0.822116934412209,
-36.03007982314));
#31756=CARTESIAN_POINT('Ctrl Pts',(3.24307756610912,-0.987032458026619,
-36.0397730594453));
#31757=CARTESIAN_POINT('Ctrl Pts',(3.23206597784166,-1.0225137907367,-36.0418937634142));
#31758=CARTESIAN_POINT('Ctrl Pts',(3.21416459467101,-1.07701430337186,-36.0452159703073));
#31759=CARTESIAN_POINT('Ctrl Pts',(3.20768363928058,-1.09616580725634,-36.0463958819132));
#31760=CARTESIAN_POINT('Ctrl Pts',(3.19509987967942,-1.13228393278525,-36.0486467893349));
#31761=CARTESIAN_POINT('Ctrl Pts',(3.18903242051825,-1.14926163652814,-36.0497158626368));
#31762=CARTESIAN_POINT('Ctrl Pts',(3.17377481149534,-1.19090355814875,-36.0523641535892));
#31763=CARTESIAN_POINT('Ctrl Pts',(3.16443237271307,-1.21551038823812,-36.0539516705828));
#31764=CARTESIAN_POINT('Ctrl Pts',(3.12893441450875,-1.30582382773512,-36.0598554938788));
#31765=CARTESIAN_POINT('Ctrl Pts',(3.10101240869683,-1.37081257914646,-36.0642554892892));
#31766=CARTESIAN_POINT('Ctrl Pts',(2.96385617729914,-1.6643695609491,-36.084688331463));
#31767=CARTESIAN_POINT('Ctrl Pts',(2.83124558311262,-1.88112471373453,-36.1012865895793));
#31768=CARTESIAN_POINT('Ctrl Pts',(2.6007449782222,-2.17748543488276,-36.1249797342027));
#31769=CARTESIAN_POINT('Ctrl Pts',(2.52061402688376,-2.26976374271456,-36.1325411133424));
#31770=CARTESIAN_POINT('Ctrl Pts',(2.40478894039566,-2.38942810891008,-36.1425859948302));
#31771=CARTESIAN_POINT('Ctrl Pts',(2.37328357910542,-2.42072341824658,-36.1452379737754));
#31772=CARTESIAN_POINT('Ctrl Pts',(2.31808235183769,-2.47344266355873,-36.1497512631183));
#31773=CARTESIAN_POINT('Ctrl Pts',(2.294682470455,-2.49516670040847,-36.1516251444605));
#31774=CARTESIAN_POINT('Ctrl Pts',(2.2460070190642,-2.53909214525705,-36.1554450577285));
#31775=CARTESIAN_POINT('Ctrl Pts',(2.22070084121954,-2.56125444710339,-36.1573893683854));
#31776=CARTESIAN_POINT('Ctrl Pts',(2.15427188189128,-2.6177058657963,-36.1623899192092));
#31777=CARTESIAN_POINT('Ctrl Pts',(2.11265841796573,-2.65140456864205,-36.1654226649753));
#31778=CARTESIAN_POINT('Ctrl Pts',(1.86883305616828,-2.83946820692365,-36.1826689239435));
#31779=CARTESIAN_POINT('Ctrl Pts',(1.65055822265646,-2.97166356119366,-36.1960143329014));
#31780=CARTESIAN_POINT('Ctrl Pts',(1.28447274730785,-3.14048663145417,-36.2174625177599));
#31781=CARTESIAN_POINT('Ctrl Pts',(1.1454684806342,-3.19380971652053,-36.2254370029875));
#31782=CARTESIAN_POINT('Ctrl Pts',(0.966464736469511,-3.24928429156306,
-36.2359915812267));
#31783=CARTESIAN_POINT('Ctrl Pts',(0.929310538727336,-3.26010492981414,
-36.2381976070474));
#31784=CARTESIAN_POINT('Ctrl Pts',(0.872173889432924,-3.27568912965052,
-36.2416246885382));
#31785=CARTESIAN_POINT('Ctrl Pts',(0.852318724550081,-3.28091135400362,
-36.2428219461697));
#31786=CARTESIAN_POINT('Ctrl Pts',(0.815039043511313,-3.29035527365504,
-36.2450838105314));
#31787=CARTESIAN_POINT('Ctrl Pts',(0.797626588703601,-3.29461958939148,
-36.2461461109411));
#31788=CARTESIAN_POINT('Ctrl Pts',(0.755218990477658,-3.3046493498504,-36.2487466263342));
#31789=CARTESIAN_POINT('Ctrl Pts',(0.730191005138493,-3.31026948419533,
-36.2502924458802));
#31790=CARTESIAN_POINT('Ctrl Pts',(0.640819120970191,-3.329275469935,-36.2558458677938));
#31791=CARTESIAN_POINT('Ctrl Pts',(0.576155774284394,-3.34107283756328,
-36.2599253220164));
#31792=CARTESIAN_POINT('Ctrl Pts',(0.25541767885469,-3.39000167294133,-36.2803342803101));
#31793=CARTESIAN_POINT('Ctrl Pts',(-0.00398814605230557,-3.39960966097446,
-36.2973052599942));
#31794=CARTESIAN_POINT('Ctrl Pts',(-0.384604737145773,-3.37010576771504,
-36.3214043662639));
#31795=CARTESIAN_POINT('Ctrl Pts',(-0.506636573493728,-3.35393178806398,
-36.3290225551889));
#31796=CARTESIAN_POINT('Ctrl Pts',(-0.671256265252023,-3.3229203853085,
-36.3391273503782));
#31797=CARTESIAN_POINT('Ctrl Pts',(-0.714817114836644,-3.31382281267955,
-36.3417851366238));
#31798=CARTESIAN_POINT('Ctrl Pts',(-0.789320514613876,-3.29672541709016,
-36.346305115707));
#31799=CARTESIAN_POINT('Ctrl Pts',(-0.82035141690064,-3.28914107430005,
-36.3481799778022));
#31800=CARTESIAN_POINT('Ctrl Pts',(-0.883799976141665,-3.27267963660726,
-36.3519991869666));
#31801=CARTESIAN_POINT('Ctrl Pts',(-0.916202161966396,-3.26375674905641,
-36.3539418534187));
#31802=CARTESIAN_POINT('Ctrl Pts',(-0.999720855458628,-3.23941558747661,
-36.3589322959125));
#31803=CARTESIAN_POINT('Ctrl Pts',(-1.05061629678126,-3.223268677506,-36.3619567653099));
#31804=CARTESIAN_POINT('Ctrl Pts',(-1.37392680855188,-3.11222405602653,
-36.381105359474));
#31805=CARTESIAN_POINT('Ctrl Pts',(-1.63365451148497,-2.9840895650487,-36.3960674469637));
#31806=CARTESIAN_POINT('Ctrl Pts',(-1.98230938712216,-2.75276964665447,
-36.4184674235656));
#31807=CARTESIAN_POINT('Ctrl Pts',(-2.08636100829852,-2.67476776392646,
-36.4255245949722));
#31808=CARTESIAN_POINT('Ctrl Pts',(-2.20890389594356,-2.57139508772896,
-36.4346432399871));
#31809=CARTESIAN_POINT('Ctrl Pts',(-2.23187363266353,-2.55148369985361,
-36.4363901063229));
#31810=CARTESIAN_POINT('Ctrl Pts',(-2.26861513026565,-2.51875845071746,
-36.4392517641279));
#31811=CARTESIAN_POINT('Ctrl Pts',(-2.28255396088171,-2.50613370045288,
-36.4403535475563));
#31812=CARTESIAN_POINT('Ctrl Pts',(-2.30862471872654,-2.48212283686028,
-36.4424465385982));
#31813=CARTESIAN_POINT('Ctrl Pts',(-2.32077931911639,-2.47076206773626,
-36.4434358053059));
#31814=CARTESIAN_POINT('Ctrl Pts',(-2.35367410233178,-2.43955880370968,
-36.4461488812855));
#31815=CARTESIAN_POINT('Ctrl Pts',(-2.37424621315771,-2.41954205111799,
-36.4478849414556));
#31816=CARTESIAN_POINT('Ctrl Pts',(-2.46043420647661,-2.33352312116177,
-36.4553175230928));
#31817=CARTESIAN_POINT('Ctrl Pts',(-2.52356710335471,-2.26509889671435,
-36.4611607262966));
#31818=CARTESIAN_POINT('Ctrl Pts',(-2.73333483079591,-2.01808166833021,
-36.4817790773549));
#31819=CARTESIAN_POINT('Ctrl Pts',(-2.86449060378868,-1.82715035841029,
-36.4968538516686));
#31820=CARTESIAN_POINT('Ctrl Pts',(-3.03175149545973,-1.52079335139829,
-36.518847473521));
#31821=CARTESIAN_POINT('Ctrl Pts',(-3.08285550873292,-1.4143324346848,-36.5261445085339));
#31822=CARTESIAN_POINT('Ctrl Pts',(-3.14523174932234,-1.26485329195309,
-36.5359093168795));
#31823=CARTESIAN_POINT('Ctrl Pts',(-3.16136705448322,-1.22396700305792,
-36.5385332802285));
#31824=CARTESIAN_POINT('Ctrl Pts',(-3.18781798111594,-1.15292508678705,
-36.5430142105183));
#31825=CARTESIAN_POINT('Ctrl Pts',(-3.19851163163598,-1.12291726375779,
-36.544883279457));
#31826=CARTESIAN_POINT('Ctrl Pts',(-3.21967195490185,-1.06078221592646,
-36.5487065322976));
#31827=CARTESIAN_POINT('Ctrl Pts',(-3.23008448871297,-1.0286402292572,-36.5506587968162));
#31828=CARTESIAN_POINT('Ctrl Pts',(-3.25597007481545,-0.944463048939245,
-36.5557088521758));
#31829=CARTESIAN_POINT('Ctrl Pts',(-3.27067709468231,-0.892201420740232,
-36.5587822146736));
#31830=CARTESIAN_POINT('Ctrl Pts',(-3.35448665182334,-0.564380297930336,
-36.577721452716));
#31831=CARTESIAN_POINT('Ctrl Pts',(-3.38997308429562,-0.281412539648163,
-36.5924713748989));
#31832=CARTESIAN_POINT('Ctrl Pts',(-3.38964502994714,0.134382255907334,
-36.6147175253541));
#31833=CARTESIAN_POINT('Ctrl Pts',(-3.38186496413727,0.265960181732457,
-36.6218630082191));
#31834=CARTESIAN_POINT('Ctrl Pts',(-3.36284433729166,0.427356445404911,
-36.6311010535003));
#31835=CARTESIAN_POINT('Ctrl Pts',(-3.35881852960865,0.45792304174268,-36.6328719083191));
#31836=CARTESIAN_POINT('Ctrl Pts',(-3.35165350531222,0.507130139371208,
-36.635763094996));
#31837=CARTESIAN_POINT('Ctrl Pts',(-3.34877421887896,0.525807371207814,
-36.636869917773));
#31838=CARTESIAN_POINT('Ctrl Pts',(-3.34271126427504,0.563064651079814,
-36.6390983960983));
#31839=CARTESIAN_POINT('Ctrl Pts',(-3.33952847397364,0.581644161505239,
-36.6402199738387));
#31840=CARTESIAN_POINT('Ctrl Pts',(-3.33077258558937,0.630313817552062,
-36.6431832628485));
#31841=CARTESIAN_POINT('Ctrl Pts',(-3.32494679575552,0.660356107646768,
-36.6450378394294));
#31842=CARTESIAN_POINT('Ctrl Pts',(-3.29130386271036,0.822095951276855,
-36.6551452485449));
#31843=CARTESIAN_POINT('Ctrl Pts',(-3.25606967429916,0.952117015032049,
-36.663707625182));
#31844=CARTESIAN_POINT('Ctrl Pts',(-3.12402600083044,1.34508590943447,-36.6903271700678));
#31845=CARTESIAN_POINT('Ctrl Pts',(-3.0022912561801,1.59846509655454,-36.7084444283449));
#31846=CARTESIAN_POINT('Ctrl Pts',(-2.82095570685706,1.88033213273115,-36.7288563368684));
#31847=CARTESIAN_POINT('Ctrl Pts',(-2.79002312231579,1.9259313421964,-36.7321724237843));
#31848=CARTESIAN_POINT('Ctrl Pts',(-2.73825557165496,1.9983777974681,-36.7374661863661));
#31849=CARTESIAN_POINT('Ctrl Pts',(-2.71810548114049,2.02569990747675,-36.7394687402356));
#31850=CARTESIAN_POINT('Ctrl Pts',(-2.67830055027909,2.07800900967378,-36.7433162078615));
#31851=CARTESIAN_POINT('Ctrl Pts',(-2.658698040425,2.10303117235099,-36.7451628409474));
#31852=CARTESIAN_POINT('Ctrl Pts',(-2.61144485759412,2.16163190433837,-36.7495046618866));
#31853=CARTESIAN_POINT('Ctrl Pts',(-2.58349380022731,2.19496167646852,-36.7519877463303));
#31854=CARTESIAN_POINT('Ctrl Pts',(-2.47996468053917,2.31369489752438,-36.7608954913466));
#31855=CARTESIAN_POINT('Ctrl Pts',(-2.40072807146449,2.39581238245582,-36.7671729056432));
#31856=CARTESIAN_POINT('Ctrl Pts',(-2.16211110744881,2.61935405554379,-36.7848681418337));
#31857=CARTESIAN_POINT('Ctrl Pts',(-1.99336134398793,2.74995419251636,-36.7959601642627));
#31858=CARTESIAN_POINT('Ctrl Pts',(-1.71767262796747,2.92452819447855,-36.8135108449752));
#31859=CARTESIAN_POINT('Ctrl Pts',(-1.61889043833329,2.98034455534081,-36.8197082594451));
#31860=CARTESIAN_POINT('Ctrl Pts',(-1.49058127941906,3.04458194698583,-36.8278728509619));
#31861=CARTESIAN_POINT('Ctrl Pts',(-1.46347798122677,3.05770238063039,-36.8296038041403));
#31862=CARTESIAN_POINT('Ctrl Pts',(-1.41922355361421,3.07840234672147,-36.8324459480174));
#31863=CARTESIAN_POINT('Ctrl Pts',(-1.40217737988125,3.08620399007489,-36.8335444616942));
#31864=CARTESIAN_POINT('Ctrl Pts',(-1.36772187313736,3.101629107635,-36.8357741312093));
#31865=CARTESIAN_POINT('Ctrl Pts',(-1.35031146193354,3.10924832735753,-36.8369054488389));
#31866=CARTESIAN_POINT('Ctrl Pts',(-1.30402269784433,3.12904331381351,-36.8399237918581));
#31867=CARTESIAN_POINT('Ctrl Pts',(-1.27503860891919,3.14096540099801,-36.8418245155952));
#31868=CARTESIAN_POINT('Ctrl Pts',(-1.09878793836135,3.2106215156838,-36.8534296862701));
#31869=CARTESIAN_POINT('Ctrl Pts',(-0.947804513571259,3.25838663270074,
-36.8635590588152));
#31870=CARTESIAN_POINT('Ctrl Pts',(-0.541947128908081,3.3561803098806,-36.8904307750818));
#31871=CARTESIAN_POINT('Ctrl Pts',(-0.283659340571229,3.38780622133096,
-36.9071049852191));
#31872=CARTESIAN_POINT('Ctrl Pts',(0.028601019194524,3.39004160278234,-36.9260883361332));
#31873=CARTESIAN_POINT('Ctrl Pts',(0.0814713242028275,3.3891832317419,-36.9292660798254));
#31874=CARTESIAN_POINT('Ctrl Pts',(0.167776993736235,3.38576110567015,-36.9343962788525));
#31875=CARTESIAN_POINT('Ctrl Pts',(0.20123109377197,3.38393758082886,-36.936370848953));
#31876=CARTESIAN_POINT('Ctrl Pts',(0.266570915737505,3.37940359098133,-36.9402015784962));
#31877=CARTESIAN_POINT('Ctrl Pts',(0.298456049845389,3.37673700073289,-36.9420588707245));
#31878=CARTESIAN_POINT('Ctrl Pts',(0.374908411209628,3.36925181286649,-36.9464855740466));
#31879=CARTESIAN_POINT('Ctrl Pts',(0.419427706690148,3.36399981549961,-36.9490414864963));
#31880=CARTESIAN_POINT('Ctrl Pts',(0.588813788426818,3.34060205154497,-36.958696713878));
#31881=CARTESIAN_POINT('Ctrl Pts',(0.712741471448899,3.31637266219298,-36.9656115015557));
#31882=CARTESIAN_POINT('Ctrl Pts',(1.10739320832131,3.21606192873369,-36.9875518149668));
#31883=CARTESIAN_POINT('Ctrl Pts',(1.37004875909919,3.11324724875624,-37.0019599825599));
#31884=CARTESIAN_POINT('Ctrl Pts',(1.65518564131769,2.95848867263242,-37.0200676992201));
#31885=CARTESIAN_POINT('Ctrl Pts',(1.69298723811098,2.93702036054477,-37.0225246485086));
#31886=CARTESIAN_POINT('Ctrl Pts',(1.74900394862664,2.9037665458636,-37.0262664440408));
#31887=CARTESIAN_POINT('Ctrl Pts',(1.76753702866057,2.89252273379275,-37.02752135839));
#31888=CARTESIAN_POINT('Ctrl Pts',(1.80120748356269,2.87165082565038,-37.0298347818789));
#31889=CARTESIAN_POINT('Ctrl Pts',(1.81637831050721,2.8620790846298,-37.0308898363355));
#31890=CARTESIAN_POINT('Ctrl Pts',(1.84871017616473,2.84131929844363,-37.0331668332758));
#31891=CARTESIAN_POINT('Ctrl Pts',(1.86584607493384,2.83009594343037,-37.0343908267452));
#31892=CARTESIAN_POINT('Ctrl Pts',(1.91486815830668,2.79734962829294,-37.0379397423622));
#31893=CARTESIAN_POINT('Ctrl Pts',(1.94649010216414,2.77543888813075,-37.0402873377969));
#31894=CARTESIAN_POINT('Ctrl Pts',(2.09678807954769,2.66746598535107,-37.0517034879291));
#31895=CARTESIAN_POINT('Ctrl Pts',(2.21016306019687,2.57430920279654,-37.0610971714343));
#31896=CARTESIAN_POINT('Ctrl Pts',(2.50534313806257,2.29785705000134,-37.0871307831423));
#31897=CARTESIAN_POINT('Ctrl Pts',(2.67284807145013,2.10066998830198,-37.1037064956791));
#31898=CARTESIAN_POINT('Ctrl Pts',(2.84592087232235,1.84226950158106,-37.122616509712));
#31899=CARTESIAN_POINT('Ctrl Pts',(2.87442059997411,1.79747857179091,-37.1258074389278));
#31900=CARTESIAN_POINT('Ctrl Pts',(2.9191962781746,1.72331757151225,-37.1309533648295));
#31901=CARTESIAN_POINT('Ctrl Pts',(2.93610788900042,1.69434381020086,-37.1329307312326));
#31902=CARTESIAN_POINT('Ctrl Pts',(2.96829402639579,1.63727152518879,-37.136763263519));
#31903=CARTESIAN_POINT('Ctrl Pts',(2.98360647281516,1.60919855564406,-37.1386196186196));
#31904=CARTESIAN_POINT('Ctrl Pts',(3.01936366127919,1.54137782299547,-37.1430381781634));
#31905=CARTESIAN_POINT('Ctrl Pts',(3.03942424184145,1.5014336657723,-37.1455870244209));
#31906=CARTESIAN_POINT('Ctrl Pts',(3.1125202644816,1.34841362839067,-37.1551639302261));
#31907=CARTESIAN_POINT('Ctrl Pts',(3.16008498417495,1.23282958786549,-37.1620116384824));
#31908=CARTESIAN_POINT('Ctrl Pts',(3.29044171502856,0.858533473587456,-37.1833768406599));
#31909=CARTESIAN_POINT('Ctrl Pts',(3.34859577502072,0.592424749464088,-37.1973250982588));
#31910=CARTESIAN_POINT('Ctrl Pts',(3.37955854481869,0.268210537440614,-37.2153890060495));
#31911=CARTESIAN_POINT('Ctrl Pts',(3.38342059865414,0.214049645652439,-37.2184446951969));
#31912=CARTESIAN_POINT('Ctrl Pts',(3.38700690646354,0.138070557565989,-37.2228128932157));
#31913=CARTESIAN_POINT('Ctrl Pts',(3.38782396716887,0.116309836825469,-37.2240733226089));
#31914=CARTESIAN_POINT('Ctrl Pts',(3.38893230618268,0.0765870004195238,
-37.2263936415217));
#31915=CARTESIAN_POINT('Ctrl Pts',(3.38929056984387,0.0586273664766807,
-37.2274500364975));
#31916=CARTESIAN_POINT('Ctrl Pts',(3.38975124619518,0.0202296472509258,
-37.2297254251249));
#31917=CARTESIAN_POINT('Ctrl Pts',(3.3898115965596,-0.000207515682062414,
-37.2309464411633));
#31918=CARTESIAN_POINT('Ctrl Pts',(3.38945450111496,-0.0588433031554558,
-37.2344757666043));
#31919=CARTESIAN_POINT('Ctrl Pts',(3.38857614958776,-0.0970348709187651,
-37.2368063564077));
#31920=CARTESIAN_POINT('Ctrl Pts',(3.38130764675895,-0.279124357383077,
-37.2480448577335));
#31921=CARTESIAN_POINT('Ctrl Pts',(3.36639553878297,-0.422524148933205,
-37.2572672815859));
#31922=CARTESIAN_POINT('Ctrl Pts',(3.29882244385854,-0.822604964105486,
-37.2833789204256));
#31923=CARTESIAN_POINT('Ctrl Pts',(3.22548223248983,-1.07480909643512,-37.3002134041277));
#31924=CARTESIAN_POINT('Ctrl Pts',(3.10344517744663,-1.36447447444007,-37.3193155616264));
#31925=CARTESIAN_POINT('Ctrl Pts',(3.08193473080824,-1.41238852106913,-37.3224711068088));
#31926=CARTESIAN_POINT('Ctrl Pts',(3.04491767319536,-1.48996634181312,-37.327575689948));
#31927=CARTESIAN_POINT('Ctrl Pts',(3.03007039471902,-1.51993317562204,-37.3295463900245));
#31928=CARTESIAN_POINT('Ctrl Pts',(3.0001286867717,-1.57818257771385,-37.3333764321052));
#31929=CARTESIAN_POINT('Ctrl Pts',(2.9850717517939,-1.60648035308957,-37.3352368012902));
#31930=CARTESIAN_POINT('Ctrl Pts',(2.94786720200301,-1.67407232364282,-37.3396822079954));
#31931=CARTESIAN_POINT('Ctrl Pts',(2.9253320054658,-1.71314684495043,-37.3422534649262));
#31932=CARTESIAN_POINT('Ctrl Pts',(2.83544442130496,-1.86205744407763,-37.3520722221862));
#31933=CARTESIAN_POINT('Ctrl Pts',(2.76262873746929,-1.96847401954336,-37.3591264971512));
#31934=CARTESIAN_POINT('Ctrl Pts',(2.54869887984869,-2.24578541067506,-37.3779814784511));
#31935=CARTESIAN_POINT('Ctrl Pts',(2.39663278900657,-2.40739733275429,-37.3894824164829));
#31936=CARTESIAN_POINT('Ctrl Pts',(2.16219186096096,-2.61216657409743,-37.4063826502896));
#31937=CARTESIAN_POINT('Ctrl Pts',(2.09215842396768,-2.66858736059527,-37.4113477134018));
#31938=CARTESIAN_POINT('Ctrl Pts',(1.99720371625967,-2.739048407721,-37.4180922980394));
#31939=CARTESIAN_POINT('Ctrl Pts',(1.97422573337326,-2.75565627492988,-37.4197253842781));
#31940=CARTESIAN_POINT('Ctrl Pts',(1.9374886271607,-2.78151354779837,-37.4223424989463));
#31941=CARTESIAN_POINT('Ctrl Pts',(1.92386482105408,-2.79095394479073,-37.4233143590809));
#31942=CARTESIAN_POINT('Ctrl Pts',(1.89457615652055,-2.81093270745134,-37.4254077230467));
#31943=CARTESIAN_POINT('Ctrl Pts',(1.87889147060741,-2.82144082029587,-37.4265312048687));
#31944=CARTESIAN_POINT('Ctrl Pts',(1.83739598882599,-2.84874169111144,-37.4295081505959));
#31945=CARTESIAN_POINT('Ctrl Pts',(1.81144327154188,-2.86531435828851,-37.4313747132205));
#31946=CARTESIAN_POINT('Ctrl Pts',(1.66636464947796,-2.95519868299341,-37.4418192660119));
#31947=CARTESIAN_POINT('Ctrl Pts',(1.54302397050206,-3.0214302193212,-37.4507314924348));
#31948=CARTESIAN_POINT('Ctrl Pts',(1.18920684961266,-3.18409735966954,-37.4757566309404));
#31949=CARTESIAN_POINT('Ctrl Pts',(0.951601901919277,-3.26300075000567,
-37.4918994151223));
#31950=CARTESIAN_POINT('Ctrl Pts',(0.646451305857619,-3.32812237777288,
-37.5110946502849));
#31951=CARTESIAN_POINT('Ctrl Pts',(0.585082491678947,-3.33945760328811,
-37.5148851748929));
#31952=CARTESIAN_POINT('Ctrl Pts',(0.485097299231768,-3.35508437577289,
-37.5209494477165));
#31953=CARTESIAN_POINT('Ctrl Pts',(0.446660793380559,-3.36041736702635,
-37.5232543213384));
#31954=CARTESIAN_POINT('Ctrl Pts',(0.377142923058058,-3.3688489471352,-37.5273773248536));
#31955=CARTESIAN_POINT('Ctrl Pts',(0.346094688333628,-3.37218009243607,
-37.5292024057419));
#31956=CARTESIAN_POINT('Ctrl Pts',(0.278774327175527,-3.37846325499104,
-37.5331260413979));
#31957=CARTESIAN_POINT('Ctrl Pts',(0.242491537308451,-3.38126116879864,
-37.5352196616802));
#31958=CARTESIAN_POINT('Ctrl Pts',(0.138639672853667,-3.38758931095215,
-37.5411569896988));
#31959=CARTESIAN_POINT('Ctrl Pts',(0.0709988340015097,-3.38968174063348,
-37.5449570835341));
#31960=CARTESIAN_POINT('Ctrl Pts',(-0.144585117383982,-3.38989399499833,
-37.5569040719003));
#31961=CARTESIAN_POINT('Ctrl Pts',(-0.292365903960096,-3.38035693357025,
-37.5648393572385));
#31962=CARTESIAN_POINT('Ctrl Pts',(-0.633042949054784,-3.33585579927932,
-37.5831120860962));
#31963=CARTESIAN_POINT('Ctrl Pts',(-0.824455675476544,-3.29377280567498,
-37.5933589924194));
#31964=CARTESIAN_POINT('Ctrl Pts',(-1.06912127716108,-3.21730834237275,
-37.6075128512475));
#31965=CARTESIAN_POINT('Ctrl Pts',(-1.12658631302324,-3.19763907741666,
-37.61091853786));
#31966=CARTESIAN_POINT('Ctrl Pts',(-1.20680522870482,-3.16775083396876,
-37.6158282263968));
#31967=CARTESIAN_POINT('Ctrl Pts',(-1.23002490280063,-3.15880719040272,
-37.6172680669754));
#31968=CARTESIAN_POINT('Ctrl Pts',(-1.26969868965705,-3.14302207593275,
-37.6197638466993));
#31969=CARTESIAN_POINT('Ctrl Pts',(-1.28620085178479,-3.13630513316568,
-37.6208127360023));
#31970=CARTESIAN_POINT('Ctrl Pts',(-1.32197039865203,-3.12141590972688,
-37.623110716201));
#31971=CARTESIAN_POINT('Ctrl Pts',(-1.34121534750172,-3.11319520081861,
-37.6243623844137));
#31972=CARTESIAN_POINT('Ctrl Pts',(-1.39767531321073,-3.08845698392812,
-37.6280770738331));
#31973=CARTESIAN_POINT('Ctrl Pts',(-1.43466909143979,-3.07144707079296,
-37.6305659687822));
#31974=CARTESIAN_POINT('Ctrl Pts',(-1.52121557982254,-3.02974793743015,
-37.636504449244));
#31975=CARTESIAN_POINT('Ctrl Pts',(-1.57048714084827,-3.00450311656284,
-37.6399766673075));
#31976=CARTESIAN_POINT('Ctrl Pts',(-1.76205821626018,-2.90034962716536,
-37.6537830714612));
#31977=CARTESIAN_POINT('Ctrl Pts',(-1.89921668415575,-2.81244584686513,
-37.6643368784493));
#31978=CARTESIAN_POINT('Ctrl Pts',(-2.18182813356151,-2.6011894220381,-37.6869842258551));
#31979=CARTESIAN_POINT('Ctrl Pts',(-2.3242943375951,-2.47471899656818,-37.6989877503608));
#31980=CARTESIAN_POINT('Ctrl Pts',(-2.48958259269312,-2.3010518469099,-37.7135210577582));
#31981=CARTESIAN_POINT('Ctrl Pts',(-2.52295880653563,-2.26440728119153,
-37.7164931014224));
#31982=CARTESIAN_POINT('Ctrl Pts',(-2.57711333152257,-2.20226521766441,
-37.7213812921138));
#31983=CARTESIAN_POINT('Ctrl Pts',(-2.59834487820743,-2.17717459548613,
-37.7233156263737));
#31984=CARTESIAN_POINT('Ctrl Pts',(-2.63981483415775,-2.12669613243248,
-37.727131575908));
#31985=CARTESIAN_POINT('Ctrl Pts',(-2.66006006891108,-2.10131847519678,
-37.7290133453237));
#31986=CARTESIAN_POINT('Ctrl Pts',(-2.70896848118451,-2.03817135756529,
-37.7336091891634));
#31987=CARTESIAN_POINT('Ctrl Pts',(-2.7372101902285,-2.00008334806539,-37.73630698418));
#31988=CARTESIAN_POINT('Ctrl Pts',(-2.85547402634553,-1.83338857114872,
-37.7478182860818));
#31989=CARTESIAN_POINT('Ctrl Pts',(-2.93730550228126,-1.69920245896067,
-37.7563325558353));
#31990=CARTESIAN_POINT('Ctrl Pts',(-3.11366602735139,-1.35892806351722,
-37.7768110689235));
#31991=CARTESIAN_POINT('Ctrl Pts',(-3.19740005487362,-1.14813724232075,
-37.7885726330847));
#31992=CARTESIAN_POINT('Ctrl Pts',(-3.27578789840572,-0.873576055458517,
-37.8043542459391));
#31993=CARTESIAN_POINT('Ctrl Pts',(-3.29056750668246,-0.816141003013135,
-37.8076822222157));
#31994=CARTESIAN_POINT('Ctrl Pts',(-3.30883525247797,-0.736555778015129,
-37.8123662693966));
#31995=CARTESIAN_POINT('Ctrl Pts',(-3.31362221438587,-0.714711764245834,
-37.8136593771637));
#31996=CARTESIAN_POINT('Ctrl Pts',(-3.32185796490979,-0.675267603920695,
-37.8160103588926));
#31997=CARTESIAN_POINT('Ctrl Pts',(-3.32538392814486,-0.65768411674763,
-37.8170641235992));
#31998=CARTESIAN_POINT('Ctrl Pts',(-3.33256597997833,-0.620333087254208,
-37.8193159618654));
#31999=CARTESIAN_POINT('Ctrl Pts',(-3.33618597510699,-0.600559943098764,
-37.8205157800357));
#32000=CARTESIAN_POINT('Ctrl Pts',(-3.34333417776632,-0.559454319919173,
-37.8230244000056));
#32001=CARTESIAN_POINT('Ctrl Pts',(-3.3468345659574,-0.538117922550193,
-37.8243345255739));
#32002=CARTESIAN_POINT('Ctrl Pts',(-3.35789266484639,-0.46642741696748,
-37.8287601064496));
#32003=CARTESIAN_POINT('Ctrl Pts',(-3.36451960146333,-0.415938711200474,
-37.8319156636527));
#32004=CARTESIAN_POINT('Ctrl Pts',(-3.38306006936681,-0.244907686121074,
-37.8426953985656));
#32005=CARTESIAN_POINT('Ctrl Pts',(-3.38964942260743,-0.123887546823597,
-37.8504707980399));
#32006=CARTESIAN_POINT('Ctrl Pts',(-3.38974885739846,-0.00278321141980408,
-37.8582646956288));
#32007=CARTESIAN_POINT('Ctrl Pts',(-3.38974881917027,-0.00282938752709428,
-37.858982196792));
#32008=CARTESIAN_POINT('Ctrl Pts',(-3.38983414077145,0.099390189715147,
-37.8649908067786));
#32009=CARTESIAN_POINT('Ctrl Pts',(-3.38529153041335,0.20175593427456,-37.8709994167652));
#32010=CARTESIAN_POINT('Ctrl Pts',(-3.37610800013699,0.303808877274895,
-37.8770080267518));
#32011=CARTESIAN_POINT('Ctrl Pts',(-3.36693292370258,0.405767876070146,
-37.8830111055496));
#32012=CARTESIAN_POINT('Ctrl Pts',(-3.35312545909836,0.507414208856045,
-37.8890141843475));
#32013=CARTESIAN_POINT('Ctrl Pts',(-3.33472467480924,0.608289738297792,
-37.8950172631453));
#32014=CARTESIAN_POINT('Ctrl Pts',(-3.31633295417342,0.709115579595218,
-37.9010173850135));
#32015=CARTESIAN_POINT('Ctrl Pts',(-3.29335248592252,0.809170938964297,
-37.9070175068817));
#32016=CARTESIAN_POINT('Ctrl Pts',(-3.26587398343595,0.908004508147524,
-37.9130176287499));
#32017=CARTESIAN_POINT('Ctrl Pts',(-3.23840142551516,1.00681669615636,-37.9190164525808));
#32018=CARTESIAN_POINT('Ctrl Pts',(-3.20643288476187,1.10440719477424,-37.9250152764118));
#32019=CARTESIAN_POINT('Ctrl Pts',(-3.17010955930962,1.20033763769772,-37.9310141002427));
#32020=CARTESIAN_POINT('Ctrl Pts',(-3.13378405816074,1.2962738266684,-37.9370132833916));
#32021=CARTESIAN_POINT('Ctrl Pts',(-3.09310341155129,1.39054935081851,-37.9430124665404));
#32022=CARTESIAN_POINT('Ctrl Pts',(-3.04825740120946,1.48274471115959,-37.9490116496893));
#32023=CARTESIAN_POINT('Ctrl Pts',(-3.00336872422914,1.57502778646307,-37.9550165404802));
#32024=CARTESIAN_POINT('Ctrl Pts',(-2.95430696324229,1.66522634906806,-37.9610214312712));
#32025=CARTESIAN_POINT('Ctrl Pts',(-2.90130831939265,1.75294469345813,-37.9670263220622));
#32026=CARTESIAN_POINT('Ctrl Pts',(-2.84828370879951,1.84070601554692,-37.973034154956));
#32027=CARTESIAN_POINT('Ctrl Pts',(-2.79131862071423,1.92598433427155,-37.9790419878498));
#32028=CARTESIAN_POINT('Ctrl Pts',(-2.73069194036291,2.00841394870107,-37.9850498207436));
#32029=CARTESIAN_POINT('Ctrl Pts',(-2.66996832526969,2.09097535813164,-37.9910672594368));
#32030=CARTESIAN_POINT('Ctrl Pts',(-2.6055717034346,2.1706786247095,-37.99708469813));
#32031=CARTESIAN_POINT('Ctrl Pts',(-2.53782050305355,2.24719206050151,-38.0031021368232));
#32032=CARTESIAN_POINT('Ctrl Pts',(-2.48520910559784,2.30660766876403,-38.0077749080358));
#32033=CARTESIAN_POINT('Ctrl Pts',(-2.4305756762294,2.36410045382413,-38.0124476792483));
#32034=CARTESIAN_POINT('Ctrl Pts',(-2.37408329179727,2.41953168735379,-38.0171204504608));
#32035=CARTESIAN_POINT('Ctrl Pts',(-2.30038166078931,2.49184890959507,-38.0232166856109));
#32036=CARTESIAN_POINT('Ctrl Pts',(-2.22324734380953,2.56091852646214,-38.0293129207611));
#32037=CARTESIAN_POINT('Ctrl Pts',(-2.1429983172996,2.62639739463606,-38.0354091559112));
#32038=CARTESIAN_POINT('Ctrl Pts',(-2.06285464707167,2.69179029777838,-38.0414973875166));
#32039=CARTESIAN_POINT('Ctrl Pts',(-1.97960472572916,2.75360155518141,-38.0475856191221));
#32040=CARTESIAN_POINT('Ctrl Pts',(-1.89360335282372,2.81152474729901,-38.0536738507275));
#32041=CARTESIAN_POINT('Ctrl Pts',(-1.80769016401156,2.86938854613015,-38.0597558395816));
#32042=CARTESIAN_POINT('Ctrl Pts',(-1.71903148714816,2.92337196890895,-38.0658378284358));
#32043=CARTESIAN_POINT('Ctrl Pts',(-1.62801448641066,2.97320935935178,-38.0719198172899));
#32044=CARTESIAN_POINT('Ctrl Pts',(-1.53706143579025,3.02301173318312,-38.0779975328336));
#32045=CARTESIAN_POINT('Ctrl Pts',(-1.44375373097807,3.06867366194833,-38.0840752483773));
#32046=CARTESIAN_POINT('Ctrl Pts',(-1.34850604205042,3.10997371645702,-38.090152963921));
#32047=CARTESIAN_POINT('Ctrl Pts',(-1.25329301605569,3.15125874087905,-38.0962284676373));
#32048=CARTESIAN_POINT('Ctrl Pts',(-1.15614180181199,3.18818487542941,-38.1023039713536));
#32049=CARTESIAN_POINT('Ctrl Pts',(-1.05748936925174,3.22057778922037,-38.10837947507));
#32050=CARTESIAN_POINT('Ctrl Pts',(-0.958847159831589,3.25296734620311,
-38.1144543491949));
#32051=CARTESIAN_POINT('Ctrl Pts',(-0.85870444862362,3.28082448284244,-38.1205292233197));
#32052=CARTESIAN_POINT('Ctrl Pts',(-0.757514895782916,3.30402425008761,
-38.1266040974446));
#32053=CARTESIAN_POINT('Ctrl Pts',(-0.656309489974358,3.32722765194875,
-38.1326799232961));
#32054=CARTESIAN_POINT('Ctrl Pts',(-0.554057334471316,3.34577213901651,
-38.1387557491475));
#32055=CARTESIAN_POINT('Ctrl Pts',(-0.451222937461346,3.35958374255037,
-38.144831574999));
#32056=CARTESIAN_POINT('Ctrl Pts',(-0.348280532879214,3.37340985249268,
-38.1509137823261));
#32057=CARTESIAN_POINT('Ctrl Pts',(-0.244755091134823,3.38249309473644,
-38.1569959896531));
#32058=CARTESIAN_POINT('Ctrl Pts',(-0.141116870459519,3.3868113457014,-38.1630781969802));
#32059=CARTESIAN_POINT('Ctrl Pts',(-0.037421959047741,3.39113195877587,
-38.1691637313117));
#32060=CARTESIAN_POINT('Ctrl Pts',(0.0663854255811521,3.39068239103628,
-38.1752492656431));
#32061=CARTESIAN_POINT('Ctrl Pts',(0.169836408984024,3.385492675621,-38.1813347999746));
#32062=CARTESIAN_POINT('Ctrl Pts',(0.273456962562488,3.38029445355913,-38.1874303093211));
#32063=CARTESIAN_POINT('Ctrl Pts',(0.376719521140766,3.37034060431963,-38.1935258186677));
#32064=CARTESIAN_POINT('Ctrl Pts',(0.479161483580033,3.35571293992102,-38.1996213280143));
#32065=CARTESIAN_POINT('Ctrl Pts',(0.558010455492585,3.34445411324639,-38.2043130054658));
#32066=CARTESIAN_POINT('Ctrl Pts',(0.636373404964492,3.33042744792137,-38.2090046829173));
#32067=CARTESIAN_POINT('Ctrl Pts',(0.714045197901123,3.31369046802117,-38.2136963603687));
#32068=CARTESIAN_POINT('Ctrl Pts',(0.815268669115325,3.29187849305461,-38.2198106505055));
#32069=CARTESIAN_POINT('Ctrl Pts',(0.915658892897034,3.26538818141388,-38.2259249406422));
#32070=CARTESIAN_POINT('Ctrl Pts',(1.01475235199809,3.23429787227682,-38.232039230779));
#32071=CARTESIAN_POINT('Ctrl Pts',(1.11371593249673,3.2032483122057,-38.2381455071127));
#32072=CARTESIAN_POINT('Ctrl Pts',(1.21138572463981,3.16761086832305,-38.2442517834465));
#32073=CARTESIAN_POINT('Ctrl Pts',(1.30730876727621,3.12751480404214,-38.2503580597803));
#32074=CARTESIAN_POINT('Ctrl Pts',(1.40313321354815,3.08745995328051,-38.2564580596592));
#32075=CARTESIAN_POINT('Ctrl Pts',(1.49721409006694,3.04295575948584,-38.2625580595381));
#32076=CARTESIAN_POINT('Ctrl Pts',(1.58911477883168,2.99418090338556,-38.268658059417));
#32077=CARTESIAN_POINT('Ctrl Pts',(1.68094922156511,2.94544120633237,-38.2747536621495));
#32078=CARTESIAN_POINT('Ctrl Pts',(1.77060622723507,2.89243716882074,-38.280849264882));
#32079=CARTESIAN_POINT('Ctrl Pts',(1.85767106192568,2.83539473234044,-38.2869448676145));
#32080=CARTESIAN_POINT('Ctrl Pts',(1.94470312654783,2.77837376588941,-38.2930381760416));
#32081=CARTESIAN_POINT('Ctrl Pts',(2.0291446037669,2.71731765488788,-38.2991314844687));
#32082=CARTESIAN_POINT('Ctrl Pts',(2.11060785557143,2.65249685061079,-38.3052247928958));
#32083=CARTESIAN_POINT('Ctrl Pts',(2.19206130727747,2.5876838443316,-38.3113173682928));
#32084=CARTESIAN_POINT('Ctrl Pts',(2.2705369129707,2.51910731061273,-38.3174099436897));
#32085=CARTESIAN_POINT('Ctrl Pts',(2.34567909139088,2.44707880190067,-38.3235025190866));
#32086=CARTESIAN_POINT('Ctrl Pts',(2.42083147251851,2.3750405132512,-38.3295959217255));
#32087=CARTESIAN_POINT('Ctrl Pts',(2.49264921977449,2.29954961309818,-38.3356893243644));
#32088=CARTESIAN_POINT('Ctrl Pts',(2.56081333099779,2.22095478258429,-38.3417827270033));
#32089=CARTESIAN_POINT('Ctrl Pts',(2.62904547735814,2.14228150595014,-38.3478822115155));
#32090=CARTESIAN_POINT('Ctrl Pts',(2.69361642534844,2.06049843411023,-38.3539816960276));
#32091=CARTESIAN_POINT('Ctrl Pts',(2.75424727785984,1.9759875998856,-38.3600811805398));
#32092=CARTESIAN_POINT('Ctrl Pts',(2.81490979888174,1.89143262423578,-38.3661838509149));
#32093=CARTESIAN_POINT('Ctrl Pts',(2.87162789227152,1.80414740479087,-38.3722865212901));
#32094=CARTESIAN_POINT('Ctrl Pts',(2.92416691291382,1.71454160868731,-38.3783891916652));
#32095=CARTESIAN_POINT('Ctrl Pts',(2.97678832966248,1.62479528524586,-38.3845014327607));
#32096=CARTESIAN_POINT('Ctrl Pts',(3.02521738248743,1.53272149199777,-38.3906136738563));
#32097=CARTESIAN_POINT('Ctrl Pts',(3.06926606901717,1.43875323112751,-38.3967259149518));
#32098=CARTESIAN_POINT('Ctrl Pts',(3.10180727880631,1.36933366084283,-38.4012413667267));
#32099=CARTESIAN_POINT('Ctrl Pts',(3.13195884762922,1.2988806412099,-38.4057568185016));
#32100=CARTESIAN_POINT('Ctrl Pts',(3.15966238818469,1.2275742972183,-38.4102722702765));
#32101=CARTESIAN_POINT('Ctrl Pts',(3.1971479686723,1.13108988968846,-38.4163821149949));
#32102=CARTESIAN_POINT('Ctrl Pts',(3.23027140246842,1.03272916962564,-38.4224919597134));
#32103=CARTESIAN_POINT('Ctrl Pts',(3.25884355599605,0.932922151116077,-38.4286018044318));
#32104=CARTESIAN_POINT('Ctrl Pts',(3.28737891648419,0.833243656470446,-38.4347037813584));
#32105=CARTESIAN_POINT('Ctrl Pts',(3.31137453285367,0.732122972853293,-38.440805758285));
#32106=CARTESIAN_POINT('Ctrl Pts',(3.33068962614992,0.630009267199531,-38.4469077352115));
#32107=CARTESIAN_POINT('Ctrl Pts',(3.34998532524936,0.5279980934505,-38.453003585171));
#32108=CARTESIAN_POINT('Ctrl Pts',(3.36460976864686,0.424996297323794,-38.4590994351304));
#32109=CARTESIAN_POINT('Ctrl Pts',(3.37447245260414,0.321466528764371,-38.4651952850899));
#32110=CARTESIAN_POINT('Ctrl Pts',(3.38432840853305,0.218007385120252,-38.4712869766426));
#32111=CARTESIAN_POINT('Ctrl Pts',(3.38942902447563,0.114021408496264,-38.4773786681953));
#32112=CARTESIAN_POINT('Ctrl Pts',(3.38973531170907,0.00997893043375072,
-38.483470359748));
#32113=CARTESIAN_POINT('Ctrl Pts',(3.39004149101343,-0.0940268852787506,
-38.4895599047185));
#32114=CARTESIAN_POINT('Ctrl Pts',(3.38555669829589,-0.19808873698997,-38.4956494496891));
#32115=CARTESIAN_POINT('Ctrl Pts',(3.37629402602813,-0.301734506324266,
-38.5017389946596));
#32116=CARTESIAN_POINT('Ctrl Pts',(3.36703223868343,-0.405370373707195,
-38.5078279578565));
#32117=CARTESIAN_POINT('Ctrl Pts',(3.35299351755496,-0.508589813170739,
-38.5139169210534));
#32118=CARTESIAN_POINT('Ctrl Pts',(3.33424290886367,-0.610924943992602,
-38.5200058842503));
#32119=CARTESIAN_POINT('Ctrl Pts',(3.31548927569185,-0.713276581511107,
-38.5260958295993));
#32120=CARTESIAN_POINT('Ctrl Pts',(3.29202232159112,-0.814743207624254,
-38.5321857749483));
#32121=CARTESIAN_POINT('Ctrl Pts',(3.26395820546061,-0.914867146369542,
-38.5382757202974));
#32122=CARTESIAN_POINT('Ctrl Pts',(3.23586487097873,-1.01509532700183,-38.5443720060621));
#32123=CARTESIAN_POINT('Ctrl Pts',(3.20316493152196,-1.11397761737651,-38.5504682918269));
#32124=CARTESIAN_POINT('Ctrl Pts',(3.16602444086707,-1.21107155128522,-38.5565645775916));
#32125=CARTESIAN_POINT('Ctrl Pts',(3.12886369340613,-1.30821844122526,-38.5626641883334));
#32126=CARTESIAN_POINT('Ctrl Pts',(3.08725774069385,-1.40357464094468,-38.5687637990752));
#32127=CARTESIAN_POINT('Ctrl Pts',(3.04142001497191,-1.49671953118421,-38.574863409817));
#32128=CARTESIAN_POINT('Ctrl Pts',(2.99550844485433,-1.59001447747511,-38.5809728470076));
#32129=CARTESIAN_POINT('Ctrl Pts',(2.94535168890258,-1.68109062429625,-38.5870822841983));
#32130=CARTESIAN_POINT('Ctrl Pts',(2.89120828233017,-1.76955353993187,-38.593191721389));
#32131=CARTESIAN_POINT('Ctrl Pts',(2.85086593011768,-1.83546742171807,-38.5977438743207));
#32132=CARTESIAN_POINT('Ctrl Pts',(2.80831121941705,-1.89993105791082,-38.6022960272525));
#32133=CARTESIAN_POINT('Ctrl Pts',(2.76366569239595,-1.96279316362515,-38.6068481801843));
#32134=CARTESIAN_POINT('Ctrl Pts',(2.70438964570048,-2.04625543548805,-38.6128920920329));
#32135=CARTESIAN_POINT('Ctrl Pts',(2.64121868490761,-2.12718573413482,-38.6189360038816));
#32136=CARTESIAN_POINT('Ctrl Pts',(2.57439814735876,-2.20519369701978,-38.6249799157302));
#32137=CARTESIAN_POINT('Ctrl Pts',(2.50766623068107,-2.28309820168843,-38.6310158118286));
#32138=CARTESIAN_POINT('Ctrl Pts',(2.43729463655874,-2.35808774356995,-38.6370517079271));
#32139=CARTESIAN_POINT('Ctrl Pts',(2.36357170776567,-2.42980119449095,-38.6430876040255));
#32140=CARTESIAN_POINT('Ctrl Pts',(2.28992444284467,-2.50144104392237,-38.6491173053176));
#32141=CARTESIAN_POINT('Ctrl Pts',(2.21293299079736,-2.56981118262046,-38.6551470066097));
#32142=CARTESIAN_POINT('Ctrl Pts',(2.1329250015896,-2.63458459725513,-38.6611767079018));
#32143=CARTESIAN_POINT('Ctrl Pts',(2.05297011955903,-2.6993150170184,-38.6672024068384));
#32144=CARTESIAN_POINT('Ctrl Pts',(1.97000301736443,-2.76045318269514,-38.6732281057749));
#32145=CARTESIAN_POINT('Ctrl Pts',(1.8843864639987,-2.81771054524741,-38.6792538047115));
#32146=CARTESIAN_POINT('Ctrl Pts',(1.79879887582025,-2.87494853689343,-38.6852774650762));
#32147=CARTESIAN_POINT('Ctrl Pts',(1.71056397940562,-2.92830809062396,-38.6913011254409));
#32148=CARTESIAN_POINT('Ctrl Pts',(1.62007495157907,-2.97754298268993,-38.6973247858056));
#32149=CARTESIAN_POINT('Ctrl Pts',(1.52959198350284,-3.02677457765835,-38.7033480427858));
#32150=CARTESIAN_POINT('Ctrl Pts',(1.43685556758776,-3.07188185110027,-38.7093712997659));
#32151=CARTESIAN_POINT('Ctrl Pts',(1.34228408306178,-3.11266421299488,-38.715394556746));
#32152=CARTESIAN_POINT('Ctrl Pts',(1.24769326879543,-3.15345491051487,-38.7214190448372));
#32153=CARTESIAN_POINT('Ctrl Pts',(1.15126704190743,-3.18991876770193,-38.7274435329283));
#32154=CARTESIAN_POINT('Ctrl Pts',(1.05344341489572,-3.22190347994983,-38.7334680210194));
#32155=CARTESIAN_POINT('Ctrl Pts',(0.955504118820467,-3.25392601170848,
-38.7394996326135));
#32156=CARTESIAN_POINT('Ctrl Pts',(0.856164539250224,-3.28145868734966,
-38.7455312442075));
#32157=CARTESIAN_POINT('Ctrl Pts',(0.755877434432334,-3.304399244434,-38.7515628558016));
#32158=CARTESIAN_POINT('Ctrl Pts',(0.655529636183558,-3.32735368506916,
-38.7575981177075));
#32159=CARTESIAN_POINT('Ctrl Pts',(0.554233600829645,-3.34571039835397,
-38.7636333796133));
#32160=CARTESIAN_POINT('Ctrl Pts',(0.452449651290486,-3.35941875561043,
-38.7696686415192));
#32161=CARTESIAN_POINT('Ctrl Pts',(0.350479551375543,-3.37315218377312,
-38.7757149411798));
#32162=CARTESIAN_POINT('Ctrl Pts',(0.248020189943388,-3.38222023803654,
-38.7817612408404));
#32163=CARTESIAN_POINT('Ctrl Pts',(0.145534609622456,-3.38662438718882,
-38.787807540501));
#32164=CARTESIAN_POINT('Ctrl Pts',(0.0573004147538147,-3.390416106505,-38.7930130570314));
#32165=CARTESIAN_POINT('Ctrl Pts',(-0.0309530534813594,-3.39075170782255,
-38.7982185735618));
#32166=CARTESIAN_POINT('Ctrl Pts',(-0.118933916524157,-3.38766287962664,
-38.8034240900922));
#32167=CARTESIAN_POINT('Ctrl Pts',(-0.224849347785803,-3.38394440541362,
-38.8096907316002));
#32168=CARTESIAN_POINT('Ctrl Pts',(-0.330736464059233,-3.37524930895149,
-38.8159573731083));
#32169=CARTESIAN_POINT('Ctrl Pts',(-0.43610525559405,-3.36157957938575,
-38.8222240146163));
#32170=CARTESIAN_POINT('Ctrl Pts',(-0.541321542207547,-3.34792963462537,
-38.8284815861364));
#32171=CARTESIAN_POINT('Ctrl Pts',(-0.646020603782136,-3.32931943810331,
-38.8347391576565));
#32172=CARTESIAN_POINT('Ctrl Pts',(-0.749714638658902,-3.30580293167644,
-38.8409967291765));
#32173=CARTESIAN_POINT('Ctrl Pts',(-0.85328208895224,-3.28231513304529,
-38.8472466617607));
#32174=CARTESIAN_POINT('Ctrl Pts',(-0.955846567181931,-3.25393303523451,
-38.8534965943449));
#32175=CARTESIAN_POINT('Ctrl Pts',(-1.05692811526889,-3.22076202499566,
-38.8597465269291));
#32176=CARTESIAN_POINT('Ctrl Pts',(-1.1578921628135,-3.18762957383874,-38.8659891943845));
#32177=CARTESIAN_POINT('Ctrl Pts',(-1.2573763363218,-3.14971942491507,-38.8722318618399));
#32178=CARTESIAN_POINT('Ctrl Pts',(-1.35491429957384,-3.10718720120149,
-38.8784745292952));
#32179=CARTESIAN_POINT('Ctrl Pts',(-1.45238591808696,-3.06468390765195,
-38.8847129505256));
#32180=CARTESIAN_POINT('Ctrl Pts',(-1.54791359598286,-3.01756495602677,
-38.8909513717559));
#32181=CARTESIAN_POINT('Ctrl Pts',(-1.64104963928406,-2.96603458238532,
-38.8971897929862));
#32182=CARTESIAN_POINT('Ctrl Pts',(-1.73414143229932,-2.91452869157229,
-38.9034252502521));
#32183=CARTESIAN_POINT('Ctrl Pts',(-1.82484350394313,-2.85861574463121,
-38.9096607075179));
#32184=CARTESIAN_POINT('Ctrl Pts',(-1.91273200068808,-2.79854629335371,
-38.9158961647838));
#32185=CARTESIAN_POINT('Ctrl Pts',(-2.00059675223758,-2.73849307128611,
-38.9221299373906));
#32186=CARTESIAN_POINT('Ctrl Pts',(-2.08564911350769,-2.67428580704603,
-38.9283637099974));
#32187=CARTESIAN_POINT('Ctrl Pts',(-2.16749398185336,-2.6062185060216,-38.9345974826042));
#32188=CARTESIAN_POINT('Ctrl Pts',(-2.2493552757425,-2.53813754448999,-38.9408325062742));
#32189=CARTESIAN_POINT('Ctrl Pts',(-2.32800748004704,-2.46619525002732,
-38.9470675299442));
#32190=CARTESIAN_POINT('Ctrl Pts',(-2.40308851994954,-2.39072596250318,
-38.9533025536142));
#32191=CARTESIAN_POINT('Ctrl Pts',(-2.47817601732117,-2.31525018411803,
-38.9595381135377));
#32192=CARTESIAN_POINT('Ctrl Pts',(-2.54969146119573,-2.23624709626379,
-38.9657736734613));
#32193=CARTESIAN_POINT('Ctrl Pts',(-2.61731033495177,-2.15408720182231,
-38.9720092333848));
#32194=CARTESIAN_POINT('Ctrl Pts',(-2.68497354999018,-2.07187343077986,
-38.9782488822957));
#32195=CARTESIAN_POINT('Ctrl Pts',(-2.74873484185292,-1.98649903094724,
-38.9844885312067));
#32196=CARTESIAN_POINT('Ctrl Pts',(-2.80831063467403,-1.89836678270475,
-38.9907281801176));
#32197=CARTESIAN_POINT('Ctrl Pts',(-2.83781956101856,-1.85471334732747,
-38.9938187867451));
#32198=CARTESIAN_POINT('Ctrl Pts',(-2.86630228420872,-1.81038376008177,
-38.9969093933725));
#32199=CARTESIAN_POINT('Ctrl Pts',(-2.89372837779135,-1.76542944862293,
-39.));
#32200=CARTESIAN_POINT('Origin',(0.,0.,-25.2396150285955));
#32201=CARTESIAN_POINT('',(-4.08499846294095,-0.00354369441070796,-29.6146150285489));
#32202=CARTESIAN_POINT('Ctrl Pts',(2.48705727606859,3.24064362520075,-28.807442179994));
#32203=CARTESIAN_POINT('Ctrl Pts',(2.58164700590404,3.16804999781167,-28.8132572105571));
#32204=CARTESIAN_POINT('Ctrl Pts',(2.67316058774221,3.09123106367021,-28.8190722411201));
#32205=CARTESIAN_POINT('Ctrl Pts',(2.76120186744336,3.01047990314291,-28.8248872716832));
#32206=CARTESIAN_POINT('Ctrl Pts',(2.84917143199732,2.92979451950324,-28.8306975655389));
#32207=CARTESIAN_POINT('Ctrl Pts',(2.93367402287073,2.84518355732362,-28.8365078593947));
#32208=CARTESIAN_POINT('Ctrl Pts',(3.01434615521614,2.75698064130557,-28.8423181532505));
#32209=CARTESIAN_POINT('Ctrl Pts',(3.09498008804593,2.66881949074692,-28.8481256958413));
#32210=CARTESIAN_POINT('Ctrl Pts',(3.17178689450958,2.57707006898604,-28.853933238432));
#32211=CARTESIAN_POINT('Ctrl Pts',(3.24443994965179,2.48210282081615,-28.8597407810228));
#32212=CARTESIAN_POINT('Ctrl Pts',(3.31707661506872,2.38715699620656,-28.8655470134963));
#32213=CARTESIAN_POINT('Ctrl Pts',(3.38556114487292,2.28899511246094,-28.8713532459698));
#32214=CARTESIAN_POINT('Ctrl Pts',(3.44960762164253,2.18802016825845,-28.8771594784432));
#32215=CARTESIAN_POINT('Ctrl Pts',(3.51365472080847,2.08704424279302,-28.882965767341));
#32216=CARTESIAN_POINT('Ctrl Pts',(3.57326346288696,1.98325554704796,-28.8887720562387));
#32217=CARTESIAN_POINT('Ctrl Pts',(3.62819198975171,1.87708494360312,-28.8945783451365));
#32218=CARTESIAN_POINT('Ctrl Pts',(3.68313397534118,1.77088832597209,-28.9003860567056));
#32219=CARTESIAN_POINT('Ctrl Pts',(3.73339327778706,1.66230900215408,-28.9061937682748));
#32220=CARTESIAN_POINT('Ctrl Pts',(3.77877489615272,1.55180065865626,-28.9120014798439));
#32221=CARTESIAN_POINT('Ctrl Pts',(3.82420481518244,1.44117469867477,-28.9178153726895));
#32222=CARTESIAN_POINT('Ctrl Pts',(3.86474652885717,1.32861599717976,-28.923629265535));
#32223=CARTESIAN_POINT('Ctrl Pts',(3.90025385988548,1.21459657024397,-28.9294431583805));
#32224=CARTESIAN_POINT('Ctrl Pts',(3.93578195114944,1.10051047904186,-28.9352604504617));
#32225=CARTESIAN_POINT('Ctrl Pts',(3.96626969242796,0.984962355085262,-28.9410777425429));
#32226=CARTESIAN_POINT('Ctrl Pts',(3.99162171258813,0.868436010074988,-28.946895034624));
#32227=CARTESIAN_POINT('Ctrl Pts',(4.01701207075936,0.751733450771981,-28.9527211237717));
#32228=CARTESIAN_POINT('Ctrl Pts',(4.03725112819439,0.634050117542279,-28.9585472129194));
#32229=CARTESIAN_POINT('Ctrl Pts',(4.05229515063293,0.515876935089047,-28.9643733020672));
#32230=CARTESIAN_POINT('Ctrl Pts',(4.06112216126169,0.446539366509142,-28.967791732945));
#32231=CARTESIAN_POINT('Ctrl Pts',(4.06816166086629,0.377033218991992,-28.9712101638229));
#32232=CARTESIAN_POINT('Ctrl Pts',(4.07341316753139,0.307457585012765,-28.9746285947007));
#32233=CARTESIAN_POINT('Ctrl Pts',(4.08236103870315,0.188909928265574,-28.9804531477395));
#32234=CARTESIAN_POINT('Ctrl Pts',(4.08614387469233,0.0697810997494614,
-28.9862777007783));
#32235=CARTESIAN_POINT('Ctrl Pts',(4.0847007864651,-0.0494417339034575,
-28.9921022538172));
#32236=CARTESIAN_POINT('Ctrl Pts',(4.08325951286277,-0.168514649680232,
-28.9979194827168));
#32237=CARTESIAN_POINT('Ctrl Pts',(4.07660539043645,-0.287680930906462,
-29.0037367116165));
#32238=CARTESIAN_POINT('Ctrl Pts',(4.06472931976189,-0.406448713945576,
-29.0095539405162));
#32239=CARTESIAN_POINT('Ctrl Pts',(4.05286509059105,-0.525098074891956,
-29.0153653691189));
#32240=CARTESIAN_POINT('Ctrl Pts',(4.03578931186541,-0.64334932428627,-29.0211767977215));
#32241=CARTESIAN_POINT('Ctrl Pts',(4.01354491966947,-0.760711625910505,
-29.0269882263242));
#32242=CARTESIAN_POINT('Ctrl Pts',(3.99054423949725,-0.882064133102252,
-29.0329972379194));
#32243=CARTESIAN_POINT('Ctrl Pts',(3.96201723460135,-1.00246572457672,-29.0390062495145));
#32244=CARTESIAN_POINT('Ctrl Pts',(3.92806967614734,-1.12138022959733,-29.0450152611097));
#32245=CARTESIAN_POINT('Ctrl Pts',(3.89527504687168,-1.23625615249857,-29.050820194264));
#32246=CARTESIAN_POINT('Ctrl Pts',(3.85742219141108,-1.34974393339543,-29.0566251274183));
#32247=CARTESIAN_POINT('Ctrl Pts',(3.81465806888086,-1.46137223783749,-29.0624300605726));
#32248=CARTESIAN_POINT('Ctrl Pts',(3.77190019058608,-1.57298424278892,-29.0682341461152));
#32249=CARTESIAN_POINT('Ctrl Pts',(3.724232617372,-1.68273693020281,-29.0740382316579));
#32250=CARTESIAN_POINT('Ctrl Pts',(3.67185123912532,-1.79017694034246,-29.0798423172005));
#32251=CARTESIAN_POINT('Ctrl Pts',(3.61946516013535,-1.89762659222739,-29.085646923606));
#32252=CARTESIAN_POINT('Ctrl Pts',(3.56236461393751,-2.00276278730165,-29.0914515300115));
#32253=CARTESIAN_POINT('Ctrl Pts',(3.50079213651266,-2.10515543771265,-29.0972561364171));
#32254=CARTESIAN_POINT('Ctrl Pts',(3.43919961752166,-2.20758141647362,-29.103062632196));
#32255=CARTESIAN_POINT('Ctrl Pts',(3.37313248268168,-2.30726172496065,-29.108869127975));
#32256=CARTESIAN_POINT('Ctrl Pts',(3.30287704283458,-2.40379455027178,-29.1146756237539));
#32257=CARTESIAN_POINT('Ctrl Pts',(3.23254417097476,-2.50043376920843,-29.1204885191605));
#32258=CARTESIAN_POINT('Ctrl Pts',(3.15801402041512,-2.59391825050628,-29.1263014145671));
#32259=CARTESIAN_POINT('Ctrl Pts',(3.0796137970976,-2.68387851079853,-29.1321143099737));
#32260=CARTESIAN_POINT('Ctrl Pts',(3.0011620114909,-2.77389793618952,-29.1379310284076));
#32261=CARTESIAN_POINT('Ctrl Pts',(2.91883536487427,-2.86038822961364,-29.1437477468415));
#32262=CARTESIAN_POINT('Ctrl Pts',(2.83299741639933,-2.94301726781796,-29.1495644652754));
#32263=CARTESIAN_POINT('Ctrl Pts',(2.74703775313504,-3.02576347070479,-29.1553894315842));
#32264=CARTESIAN_POINT('Ctrl Pts',(2.65755715590551,-3.10463722190456,-29.1612143978929));
#32265=CARTESIAN_POINT('Ctrl Pts',(2.56495174898386,-3.17934702814661,-29.1670393642017));
#32266=CARTESIAN_POINT('Ctrl Pts',(2.54287925952979,-3.19715410297312,-29.1684277443373));
#32267=CARTESIAN_POINT('Ctrl Pts',(2.5206293729239,-3.21472481756346,-29.169816124473));
#32268=CARTESIAN_POINT('Ctrl Pts',(2.49820767935441,-3.23205559834831,-29.1712045046086));
#32269=CARTESIAN_POINT('Ctrl Pts',(2.40412529591361,-3.30477629440437,-29.1770302069301));
#32270=CARTESIAN_POINT('Ctrl Pts',(2.30671462318317,-3.37350184690707,-29.1828559092517));
#32271=CARTESIAN_POINT('Ctrl Pts',(2.20634918628449,-3.43791335960954,-29.1886816115732));
#32272=CARTESIAN_POINT('Ctrl Pts',(2.1061096874175,-3.50224404907865,-29.1945000038336));
#32273=CARTESIAN_POINT('Ctrl Pts',(2.00292313929499,-3.5622712473514,-29.2003183960939));
#32274=CARTESIAN_POINT('Ctrl Pts',(1.89719547046546,-3.61771673115037,-29.2061367883543));
#32275=CARTESIAN_POINT('Ctrl Pts',(1.79157297222626,-3.67310706160749,-29.2119493928795));
#32276=CARTESIAN_POINT('Ctrl Pts',(1.68341474126908,-3.72392455612287,-29.2177619974047));
#32277=CARTESIAN_POINT('Ctrl Pts',(1.57315446568604,-3.76993501629565,-29.2235746019299));
#32278=CARTESIAN_POINT('Ctrl Pts',(1.45917678316605,-3.81749671151581,-29.2295831774543));
#32279=CARTESIAN_POINT('Ctrl Pts',(1.34295318503273,-3.85992126840636,-29.2355917529787));
#32280=CARTESIAN_POINT('Ctrl Pts',(1.22498937260595,-3.89700218591195,-29.2416003285032));
#32281=CARTESIAN_POINT('Ctrl Pts',(1.11100003196341,-3.93283376213796,-29.2474064613175));
#32282=CARTESIAN_POINT('Ctrl Pts',(0.995386272004685,-3.96367584593016,
-29.2532125941318));
#32283=CARTESIAN_POINT('Ctrl Pts',(0.878622705452774,-3.98939182601344,
-29.2590187269461));
#32284=CARTESIAN_POINT('Ctrl Pts',(0.761876050015233,-4.01510408159692,
-29.2648240188459));
#32285=CARTESIAN_POINT('Ctrl Pts',(0.643980317493258,-4.0356916222519,-29.2706293107457));
#32286=CARTESIAN_POINT('Ctrl Pts',(0.525422027187254,-4.05106858660113,
-29.2764346026455));
#32287=CARTESIAN_POINT('Ctrl Pts',(0.406852989532603,-4.06644694487731,
-29.2822404207969));
#32288=CARTESIAN_POINT('Ctrl Pts',(0.287621679281552,-4.07661373524268,
-29.2880462389484));
#32289=CARTESIAN_POINT('Ctrl Pts',(0.168220844391062,-4.08153485192916,
-29.2938520570999));
#32290=CARTESIAN_POINT('Ctrl Pts',(0.0487810691944442,-4.08645757354403,
-29.2996597687082));
#32291=CARTESIAN_POINT('Ctrl Pts',(-0.0708279331831924,-4.08613120229194,
-29.3054674803166));
#32292=CARTESIAN_POINT('Ctrl Pts',(-0.190112941066558,-4.08057374270323,
-29.311275191925));
#32293=CARTESIAN_POINT('Ctrl Pts',(-0.309529390787627,-4.07501015927117,
-29.3170893031329));
#32294=CARTESIAN_POINT('Ctrl Pts',(-0.428620725640996,-4.06420400086641,
-29.3229034143409));
#32295=CARTESIAN_POINT('Ctrl Pts',(-0.546898218435627,-4.04822520849223,
-29.3287175255488));
#32296=CARTESIAN_POINT('Ctrl Pts',(-0.665253511881017,-4.03223590557698,
-29.3345354611668));
#32297=CARTESIAN_POINT('Ctrl Pts',(-0.78279349654856,-4.0110672646297,-29.3403533967849));
#32298=CARTESIAN_POINT('Ctrl Pts',(-0.899040636338648,-3.98484013910368,
-29.3461713324029));
#32299=CARTESIAN_POINT('Ctrl Pts',(-1.01545243297985,-3.95857586448382,
-29.3519975087653));
#32300=CARTESIAN_POINT('Ctrl Pts',(-1.13056733763087,-3.92723891158967,
-29.3578236851276));
#32301=CARTESIAN_POINT('Ctrl Pts',(-1.24392381923684,-3.89099968284954,
-29.36364986149));
#32302=CARTESIAN_POINT('Ctrl Pts',(-1.27071239828836,-3.88243557226568,
-29.3650267124988));
#32303=CARTESIAN_POINT('Ctrl Pts',(-1.29740286653171,-3.87359788932101,
-29.3664035635076));
#32304=CARTESIAN_POINT('Ctrl Pts',(-1.32398931486147,-3.86448926691906,
-29.3677804145163));
#32305=CARTESIAN_POINT('Ctrl Pts',(-1.43647825555107,-3.82595011071335,
-29.3736059580242));
#32306=CARTESIAN_POINT('Ctrl Pts',(-1.54746295502343,-3.78243370292111,
-29.3794315015321));
#32307=CARTESIAN_POINT('Ctrl Pts',(-1.65647161659419,-3.73407642977722,
-29.38525704504));
#32308=CARTESIAN_POINT('Ctrl Pts',(-1.76534349629072,-3.68577983436626,
-29.3910752787732));
#32309=CARTESIAN_POINT('Ctrl Pts',(-1.87224390013117,-3.63265461935452,
-29.3968935125064));
#32310=CARTESIAN_POINT('Ctrl Pts',(-1.97671716030412,-3.57488660913311,
-29.4027117462395));
#32311=CARTESIAN_POINT('Ctrl Pts',(-2.08108650355432,-3.51717605929769,
-29.408524192722));
#32312=CARTESIAN_POINT('Ctrl Pts',(-2.18303315099799,-3.45483209784832,
-29.4143366392045));
#32313=CARTESIAN_POINT('Ctrl Pts',(-2.2821229182699,-3.38808795427558,-29.420149085687));
#32314=CARTESIAN_POINT('Ctrl Pts',(-2.38455727880139,-3.31909098461538,
-29.4261577206344));
#32315=CARTESIAN_POINT('Ctrl Pts',(-2.48393808422484,-3.24539171838284,
-29.4321663555818));
#32316=CARTESIAN_POINT('Ctrl Pts',(-2.57981460119327,-3.16729878973709,
-29.4381749905292));
#32317=CARTESIAN_POINT('Ctrl Pts',(-2.67245741625451,-3.09183976207444,
-29.4439809675692));
#32318=CARTESIAN_POINT('Ctrl Pts',(-2.76182817335498,-3.01227894803338,
-29.4497869446093));
#32319=CARTESIAN_POINT('Ctrl Pts',(-2.84755165172228,-2.92893745081279,
-29.4555929216494));
#32320=CARTESIAN_POINT('Ctrl Pts',(-2.93326273082004,-2.84560800832572,
-29.4613980588977));
#32321=CARTESIAN_POINT('Ctrl Pts',(-3.01532728789925,-2.75849925454101,
-29.4672031961459));
#32322=CARTESIAN_POINT('Ctrl Pts',(-3.09340592558045,-2.66797016092455,
-29.4730083333942));
#32323=CARTESIAN_POINT('Ctrl Pts',(-3.17149165880314,-2.57743284030824,
-29.4788139981951));
#32324=CARTESIAN_POINT('Ctrl Pts',(-3.2455904859473,-2.48347487083025,-29.484619662996));
#32325=CARTESIAN_POINT('Ctrl Pts',(-3.31540279742206,-2.38648890440455,
-29.490425327797));
#32326=CARTESIAN_POINT('Ctrl Pts',(-3.38523789525339,-2.28947128228993,
-29.4962328875351));
#32327=CARTESIAN_POINT('Ctrl Pts',(-3.45078345666214,-2.18942402861275,
-29.5020404472733));
#32328=CARTESIAN_POINT('Ctrl Pts',(-3.51178312296444,-2.08676886531837,
-29.5078480070114));
#32329=CARTESIAN_POINT('Ctrl Pts',(-3.57285003860565,-1.98400052940707,
-29.5136619693183));
#32330=CARTESIAN_POINT('Ctrl Pts',(-3.62936084713854,-1.8786188959865,-29.5194759316251));
#32331=CARTESIAN_POINT('Ctrl Pts',(-3.68110502949018,-1.77107051295597,
-29.525289893932));
#32332=CARTESIAN_POINT('Ctrl Pts',(-3.7328832629757,-1.66345135589397,-29.531107682215));
#32333=CARTESIAN_POINT('Ctrl Pts',(-3.7798884630376,-1.55366298372032,-29.536925470498));
#32334=CARTESIAN_POINT('Ctrl Pts',(-3.82195878033918,-1.44217061452112,
-29.542743258781));
#32335=CARTESIAN_POINT('Ctrl Pts',(-3.8640887137464,-1.33052025409946,-29.548569291211));
#32336=CARTESIAN_POINT('Ctrl Pts',(-3.90126968056075,-1.2171614635597,-29.5543953236411));
#32337=CARTESIAN_POINT('Ctrl Pts',(-3.93339001154322,-1.10257336131979,
-29.5602213560711));
#32338=CARTESIAN_POINT('Ctrl Pts',(-3.94098903962392,-1.07546410746093,
-29.5615996788555));
#32339=CARTESIAN_POINT('Ctrl Pts',(-3.94830505004656,-1.04828608618615,
-29.5629780016398));
#32340=CARTESIAN_POINT('Ctrl Pts',(-3.95533698646056,-1.0210457010032,-29.5643563244242));
#32341=CARTESIAN_POINT('Ctrl Pts',(-3.9935929449067,-0.872849388883327,
-29.5718548363646));
#32342=CARTESIAN_POINT('Ctrl Pts',(-4.02353545220108,-0.722426523062194,
-29.579353348305));
#32343=CARTESIAN_POINT('Ctrl Pts',(-4.0449536888374,-0.570591495871375,
-29.5868518602454));
#32344=CARTESIAN_POINT('Ctrl Pts',(-4.06597312067764,-0.421583617249565,
-29.5942107508633));
#32345=CARTESIAN_POINT('Ctrl Pts',(-4.07878279064484,-0.271215465179849,
-29.6015696414811));
#32346=CARTESIAN_POINT('Ctrl Pts',(-4.08322889380424,-0.120278014625242,
-29.608928532099));
#32347=CARTESIAN_POINT('Ctrl Pts',(-4.08437411850112,-0.0813996328464814,
-29.6108240309156));
#32348=CARTESIAN_POINT('Ctrl Pts',(-4.08496468297067,-0.0424836002528471,
-29.6127195297322));
#32349=CARTESIAN_POINT('Ctrl Pts',(-4.08499846294095,-0.00354369441070524,
-29.6146150285489));
#32350=CARTESIAN_POINT('Ctrl Pts',(-4.08499846294178,-0.00354369345236866,
-29.6146150285955));
#32351=CARTESIAN_POINT('Ctrl Pts',(-4.08510089553568,0.114535647855257,
-29.620362840432));
#32352=CARTESIAN_POINT('Ctrl Pts',(-4.08007936315259,0.232738167103182,
-29.6261106522686));
#32353=CARTESIAN_POINT('Ctrl Pts',(-4.069928608205,0.350579697236656,-29.6318584641051));
#32354=CARTESIAN_POINT('Ctrl Pts',(-4.0597836237934,0.46835423641281,-29.6376030084059));
#32355=CARTESIAN_POINT('Ctrl Pts',(-4.0445152498184,0.585767779234244,-29.6433475527066));
#32356=CARTESIAN_POINT('Ctrl Pts',(-4.02417029374906,0.702337843852654,
-29.6490920970074));
#32357=CARTESIAN_POINT('Ctrl Pts',(-4.00383097033797,0.818875635148233,
-29.6548350508867));
#32358=CARTESIAN_POINT('Ctrl Pts',(-3.9784179301521,0.934570001073691,-29.660578004766));
#32359=CARTESIAN_POINT('Ctrl Pts',(-3.94802955510798,1.04894596238026,-29.6663209586452));
#32360=CARTESIAN_POINT('Ctrl Pts',(-3.9176420426122,1.16331867722185,-29.6720637495156));
#32361=CARTESIAN_POINT('Ctrl Pts',(-3.88227958379287,1.27637265809959,-29.677806540386));
#32362=CARTESIAN_POINT('Ctrl Pts',(-3.84209096551582,1.38764621308952,-29.6835493312564));
#32363=CARTESIAN_POINT('Ctrl Pts',(-3.80189350162445,1.49894425966425,-29.6892933861293));
#32364=CARTESIAN_POINT('Ctrl Pts',(-3.75686790934974,1.60846070870447,-29.6950374410022));
#32365=CARTESIAN_POINT('Ctrl Pts',(-3.70721154631942,1.71575276506726,-29.7007814958751));
#32366=CARTESIAN_POINT('Ctrl Pts',(-3.65750360539991,1.82315626531071,-29.7065315170775));
#32367=CARTESIAN_POINT('Ctrl Pts',(-3.60315546790751,1.92833038117625,-29.7122815382799));
#32368=CARTESIAN_POINT('Ctrl Pts',(-3.54441101778661,2.03085586317515,-29.7180315594823));
#32369=CARTESIAN_POINT('Ctrl Pts',(-3.48563213688581,2.1334414365069,-29.7237849508365));
#32370=CARTESIAN_POINT('Ctrl Pts',(-3.42245203699577,2.23337493319784,-29.7295383421908));
#32371=CARTESIAN_POINT('Ctrl Pts',(-3.35515760178694,2.33026660860325,-29.735291733545));
#32372=CARTESIAN_POINT('Ctrl Pts',(-3.28776329517689,2.42730208055529,-29.7410536634842));
#32373=CARTESIAN_POINT('Ctrl Pts',(-3.21624271703737,2.52128638831926,-29.7468155934235));
#32374=CARTESIAN_POINT('Ctrl Pts',(-3.14092271218498,2.6118632269092,-29.7525775233627));
#32375=CARTESIAN_POINT('Ctrl Pts',(-3.10451842418982,2.65564157403201,-29.7553624270191));
#32376=CARTESIAN_POINT('Ctrl Pts',(-3.06722711650288,2.6986244687061,-29.7581473306756));
#32377=CARTESIAN_POINT('Ctrl Pts',(-3.02908860636657,2.74077492961028,-29.760932234332));
#32378=CARTESIAN_POINT('Ctrl Pts',(-2.9493100423512,2.82894573731889,-29.7667577270908));
#32379=CARTESIAN_POINT('Ctrl Pts',(-2.86555096101358,2.91377138955036,-29.7725832198497));
#32380=CARTESIAN_POINT('Ctrl Pts',(-2.77812274705242,2.99487211785577,-29.7784087126085));
#32381=CARTESIAN_POINT('Ctrl Pts',(-2.69080426352897,3.07587105729907,-29.7842268938389));
#32382=CARTESIAN_POINT('Ctrl Pts',(-2.59982610353627,3.15315409665027,-29.7900450750693));
#32383=CARTESIAN_POINT('Ctrl Pts',(-2.50553872285622,3.22637578534616,-29.7958632562998));
#32384=CARTESIAN_POINT('Ctrl Pts',(-2.41134515554145,3.2995246204642,-29.801675648599));
#32385=CARTESIAN_POINT('Ctrl Pts',(-2.3138492382938,3.36861989519583,-29.8074880408982));
#32386=CARTESIAN_POINT('Ctrl Pts',(-2.21343651800874,3.43335459583558,-29.8133004331974));
#32387=CARTESIAN_POINT('Ctrl Pts',(-2.10963324299415,3.50027514050781,-29.8193090878242));
#32388=CARTESIAN_POINT('Ctrl Pts',(-2.00271302621213,3.56253511807048,-29.8253177424509));
#32389=CARTESIAN_POINT('Ctrl Pts',(-1.89313725188156,3.61984203322995,-29.8313263970777));
#32390=CARTESIAN_POINT('Ctrl Pts',(-1.78725863023146,3.67521537852613,-29.8371323160752));
#32391=CARTESIAN_POINT('Ctrl Pts',(-1.67890115085158,3.72596430412592,-29.8429382350727));
#32392=CARTESIAN_POINT('Ctrl Pts',(-1.56850786000158,3.77187063578714,-29.8487441540703));
#32393=CARTESIAN_POINT('Ctrl Pts',(-1.45813056223032,3.81777031683063,-29.8545492319431));
#32394=CARTESIAN_POINT('Ctrl Pts',(-1.34571841617986,3.85882864255651,-29.860354309816));
#32395=CARTESIAN_POINT('Ctrl Pts',(-1.23173513987145,3.8948752926385,-29.8661593876888));
#32396=CARTESIAN_POINT('Ctrl Pts',(-1.11774153001839,3.93092521065313,-29.8719649918409));
#32397=CARTESIAN_POINT('Ctrl Pts',(-1.00217689574656,3.96196242663428,-29.877770595993));
#32398=CARTESIAN_POINT('Ctrl Pts',(-0.885520214903857,3.98786646579303,
-29.8835762001451));
#32399=CARTESIAN_POINT('Ctrl Pts',(-0.768825481972242,4.01377895455617,
-29.8893836980196));
#32400=CARTESIAN_POINT('Ctrl Pts',(-0.651038392130681,4.03455484808431,
-29.895191195894));
#32401=CARTESIAN_POINT('Ctrl Pts',(-0.532647580448056,4.05012488141327,
-29.9009986937685));
#32402=CARTESIAN_POINT('Ctrl Pts',(-0.414126277472672,4.0657120761566,-29.9068125927132));
#32403=CARTESIAN_POINT('Ctrl Pts',(-0.295000329181403,4.07608190427893,
-29.9126264916579));
#32404=CARTESIAN_POINT('Ctrl Pts',(-0.175763106651671,4.08121701583488,
-29.9184403906027));
#32405=CARTESIAN_POINT('Ctrl Pts',(-0.0564474366678613,4.08635550583608,
-29.9242581145742));
#32406=CARTESIAN_POINT('Ctrl Pts',(0.0629792462984349,4.08625242074811,
-29.9300758385457));
#32407=CARTESIAN_POINT('Ctrl Pts',(0.182025608117366,4.08094249873598,-29.9358935625172));
#32408=CARTESIAN_POINT('Ctrl Pts',(0.301240648911888,4.07562505299788,-29.9417195297286));
#32409=CARTESIAN_POINT('Ctrl Pts',(0.420073888093814,4.06508608140495,-29.9475454969401));
#32410=CARTESIAN_POINT('Ctrl Pts',(0.538041007510124,4.04941191708592,-29.9533714641515));
#32411=CARTESIAN_POINT('Ctrl Pts',(0.565961535053325,4.04570214661131,-29.9547503575143));
#32412=CARTESIAN_POINT('Ctrl Pts',(0.593833599717153,4.04170493758397,-29.9561292508771));
#32413=CARTESIAN_POINT('Ctrl Pts',(0.621650892464621,4.0374218466613,-29.9575081442399));
#32414=CARTESIAN_POINT('Ctrl Pts',(0.739170385986166,4.01932710679901,-29.9633335439683));
#32415=CARTESIAN_POINT('Ctrl Pts',(0.856087170397083,3.99606810769409,-29.9691589436968));
#32416=CARTESIAN_POINT('Ctrl Pts',(0.971912817304395,3.96769586480106,-29.9749843434252));
#32417=CARTESIAN_POINT('Ctrl Pts',(1.08759851749451,3.93935790276343,-29.9808027045953));
#32418=CARTESIAN_POINT('Ctrl Pts',(1.20219530906337,3.90591907906435,-29.9866210657655));
#32419=CARTESIAN_POINT('Ctrl Pts',(1.31522185004862,3.86748193081166,-29.9924394269356));
#32420=CARTESIAN_POINT('Ctrl Pts',(1.42812074180017,3.82908819247382,-29.9982512170001));
#32421=CARTESIAN_POINT('Ctrl Pts',(1.53945252905253,3.78570749722147,-30.0040630070645));
#32422=CARTESIAN_POINT('Ctrl Pts',(1.64874884363787,3.73749277599339,-30.009874797129));
#32423=CARTESIAN_POINT('Ctrl Pts',(1.75797285251911,3.68930995153494,-30.0156827423651));
#32424=CARTESIAN_POINT('Ctrl Pts',(1.86516369482128,3.63629962515944,-30.0214906876011));
#32425=CARTESIAN_POINT('Ctrl Pts',(1.96987115601415,3.57866352549433,-30.0272986328372));
#32426=CARTESIAN_POINT('Ctrl Pts',(2.07454021434151,3.52104856464166,-30.0331044479315));
#32427=CARTESIAN_POINT('Ctrl Pts',(2.17672734503127,3.45881139899725,-30.0389102630258));
#32428=CARTESIAN_POINT('Ctrl Pts',(2.27600570578405,3.3922003223923,-30.04471607812));
#32429=CARTESIAN_POINT('Ctrl Pts',(2.34793368652654,3.34394005500928,-30.0489224384299));
#32430=CARTESIAN_POINT('Ctrl Pts',(2.41833528000595,3.29338485814733,-30.0531287987397));
#32431=CARTESIAN_POINT('Ctrl Pts',(2.48705727606859,3.24064362520075,-30.0573351590495));
#32432=CARTESIAN_POINT('',(-4.08499876708699,0.00317378287634478,-29.5103849714406));
#32433=CARTESIAN_POINT('Ctrl Pts',(-4.08499876708699,0.00317378287634033,
-29.5103849714406));
#32434=CARTESIAN_POINT('Ctrl Pts',(-4.08488929600371,0.144074801529089,
-29.5172304279821));
#32435=CARTESIAN_POINT('Ctrl Pts',(-4.07748594560271,0.284674789363894,
-29.5240758845235));
#32436=CARTESIAN_POINT('Ctrl Pts',(-4.06290522156446,0.424294898136044,
-29.530921341065));
#32437=CARTESIAN_POINT('Ctrl Pts',(-4.04810681336837,0.565999477179698,
-29.5378689974313));
#32438=CARTESIAN_POINT('Ctrl Pts',(-4.025915162707,0.706694609343906,-29.5448166537975));
#32439=CARTESIAN_POINT('Ctrl Pts',(-3.99650239142486,0.845691217487437,
-29.5517643101638));
#32440=CARTESIAN_POINT('Ctrl Pts',(-3.96708962014271,0.984687825630963,
-29.5587119665301));
#32441=CARTESIAN_POINT('Ctrl Pts',(-3.93045585216911,1.12198587687786,-29.5656596228963));
#32442=CARTESIAN_POINT('Ctrl Pts',(-3.88682172051456,1.25691762376707,-29.5726072792626));
#32443=CARTESIAN_POINT('Ctrl Pts',(-3.85023392742419,1.37005966760532,-29.5784329804729));
#32444=CARTESIAN_POINT('Ctrl Pts',(-3.80864334589806,1.48178369611155,-29.5842586816833));
#32445=CARTESIAN_POINT('Ctrl Pts',(-3.76217819466759,1.59161560421092,-29.5900843828936));
#32446=CARTESIAN_POINT('Ctrl Pts',(-3.71577134776499,1.70130969557213,-29.5959027740321));
#32447=CARTESIAN_POINT('Ctrl Pts',(-3.66450225477699,1.80911601644211,-29.6017211651706));
#32448=CARTESIAN_POINT('Ctrl Pts',(-3.60854884390259,1.91457573398632,-29.6075395563091));
#32449=CARTESIAN_POINT('Ctrl Pts',(-3.55265109172022,2.01993054729239,-29.6133521597032));
#32450=CARTESIAN_POINT('Ctrl Pts',(-3.49207848178133,2.12294304271336,-29.6191647630973));
#32451=CARTESIAN_POINT('Ctrl Pts',(-3.42705671164646,2.22317504824945,-29.6249773664914));
#32452=CARTESIAN_POINT('Ctrl Pts',(-3.35984272551286,2.32678638667152,-29.6309859424364));
#32453=CARTESIAN_POINT('Ctrl Pts',(-3.28787444324839,2.42742602431081,-29.6369945183813));
#32454=CARTESIAN_POINT('Ctrl Pts',(-3.21145263674161,2.5246379863191,-29.6430030943263));
#32455=CARTESIAN_POINT('Ctrl Pts',(-3.13760567617815,2.61857462891975,-29.6488092259938));
#32456=CARTESIAN_POINT('Ctrl Pts',(-3.05960073089692,2.70931050351429,-29.6546153576614));
#32457=CARTESIAN_POINT('Ctrl Pts',(-2.97775237715265,2.79646487200568,-29.6604214893289));
#32458=CARTESIAN_POINT('Ctrl Pts',(-2.8959158777345,2.88360661768599,-29.6662267800782));
#32459=CARTESIAN_POINT('Ctrl Pts',(-2.81023735611584,2.967167591559,-29.6720320708274));
#32460=CARTESIAN_POINT('Ctrl Pts',(-2.721069871197,3.04680221807454,-29.6778373615767));
#32461=CARTESIAN_POINT('Ctrl Pts',(-2.63189430325336,3.12644406346209,-29.683643178575));
#32462=CARTESIAN_POINT('Ctrl Pts',(-2.53922944748117,3.20215858206116,-29.6894489955734));
#32463=CARTESIAN_POINT('Ctrl Pts',(-2.44346272712173,3.27363939693529,-29.6952548125717));
#32464=CARTESIAN_POINT('Ctrl Pts',(-2.34766477428718,3.34514352390325,-29.7010625230257));
#32465=CARTESIAN_POINT('Ctrl Pts',(-2.24876327173674,3.41241095722145,-29.7068702334797));
#32466=CARTESIAN_POINT('Ctrl Pts',(-2.14717545758527,3.4751780608112,-29.7126779439337));
#32467=CARTESIAN_POINT('Ctrl Pts',(-2.04547570229445,3.53801432841583,-29.7184920539911));
#32468=CARTESIAN_POINT('Ctrl Pts',(-1.94108407419197,3.59634015337465,-29.7243061640485));
#32469=CARTESIAN_POINT('Ctrl Pts',(-1.83444342769416,3.64993730228201,-29.7301202741059));
#32470=CARTESIAN_POINT('Ctrl Pts',(-1.72773263500741,3.7035697063745,-29.7359382085743));
#32471=CARTESIAN_POINT('Ctrl Pts',(-1.61877024903109,3.75246707315416,-29.7417561430428));
#32472=CARTESIAN_POINT('Ctrl Pts',(-1.50801863533895,3.79645950794559,-29.7475740775112));
#32473=CARTESIAN_POINT('Ctrl Pts',(-1.39711014864572,3.84051425537555,-29.7534002527339));
#32474=CARTESIAN_POINT('Ctrl Pts',(-1.28440776002582,3.87965007109166,-29.7592264279567));
#32475=CARTESIAN_POINT('Ctrl Pts',(-1.17038860321449,3.91374699200979,-29.7650526031795));
#32476=CARTESIAN_POINT('Ctrl Pts',(-1.14344319942173,3.9218048949791,-29.7664294651765));
#32477=CARTESIAN_POINT('Ctrl Pts',(-1.11642429684647,3.92958160727636,-29.7678063271735));
#32478=CARTESIAN_POINT('Ctrl Pts',(-1.08933825928154,3.93707596534096,-29.7691831891705));
#32479=CARTESIAN_POINT('Ctrl Pts',(-0.974731543651779,3.96878616885371,
-29.7750089815543));
#32480=CARTESIAN_POINT('Ctrl Pts',(-0.858555805965655,3.99553869464658,
-29.7808347739381));
#32481=CARTESIAN_POINT('Ctrl Pts',(-0.741277505723837,4.01717968972112,
-29.7866605663218));
#32482=CARTESIAN_POINT('Ctrl Pts',(-0.624147580059496,4.03879330570256,
-29.7924789882076));
#32483=CARTESIAN_POINT('Ctrl Pts',(-0.505918264273633,4.05530818077743,
-29.7982974100933));
#32484=CARTESIAN_POINT('Ctrl Pts',(-0.387070608536924,4.0666203835626,-29.804115831979));
#32485=CARTESIAN_POINT('Ctrl Pts',(-0.268342398844149,4.07792121718898,
-29.8099284061476));
#32486=CARTESIAN_POINT('Ctrl Pts',(-0.148997489524003,4.08402974303888,
-29.8157409803162));
#32487=CARTESIAN_POINT('Ctrl Pts',(-0.0295259523632294,4.08489329335994,
-29.8215535544847));
#32488=CARTESIAN_POINT('Ctrl Pts',(0.0898546208102128,4.08575618618565,
-29.8273617030392));
#32489=CARTESIAN_POINT('Ctrl Pts',(0.209361223302048,4.08138204855642,-29.8331698515936));
#32490=CARTESIAN_POINT('Ctrl Pts',(0.328500470335767,4.0717701851884,-29.838978000148));
#32491=CARTESIAN_POINT('Ctrl Pts',(0.447591693800847,4.06216219624456,-29.8447838075091));
#32492=CARTESIAN_POINT('Ctrl Pts',(0.566315450295777,4.04732071319067,-29.8505896148701));
#32493=CARTESIAN_POINT('Ctrl Pts',(0.684180624496516,4.02729709272405,-29.8563954222311));
#32494=CARTESIAN_POINT('Ctrl Pts',(0.802026048285521,4.0072768275721,-29.8622002567256));
#32495=CARTESIAN_POINT('Ctrl Pts',(0.919012774035862,3.9820762212117,-29.8680050912201));
#32496=CARTESIAN_POINT('Ctrl Pts',(1.03465769411707,3.9517981294601,-29.8738099257145));
#32497=CARTESIAN_POINT('Ctrl Pts',(1.15031047185885,3.92151798041998,-29.8796151546268));
#32498=CARTESIAN_POINT('Ctrl Pts',(1.26462086834682,3.8861597644006,-29.8854203835391));
#32499=CARTESIAN_POINT('Ctrl Pts',(1.37711942230712,3.84587663565857,-29.8912256124514));
#32500=CARTESIAN_POINT('Ctrl Pts',(1.48970655940519,3.80556178734489,-29.8970354124926));
#32501=CARTESIAN_POINT('Ctrl Pts',(1.60047862020886,3.7603144193227,-29.9028452125339));
#32502=CARTESIAN_POINT('Ctrl Pts',(1.7089846065242,3.71033645572249,-29.9086550125751));
#32503=CARTESIAN_POINT('Ctrl Pts',(1.81753764560202,3.66033681957378,-29.9144673319901));
#32504=CARTESIAN_POINT('Ctrl Pts',(1.92382228891063,3.60560268585826,-29.9202796514051));
#32505=CARTESIAN_POINT('Ctrl Pts',(2.0274120530472,3.54638201088926,-29.9260919708202));
#32506=CARTESIAN_POINT('Ctrl Pts',(2.13113213206795,3.48708683690518,-29.9319116020747));
#32507=CARTESIAN_POINT('Ctrl Pts',(2.23215021574526,3.42329406624566,-29.9377312333293));
#32508=CARTESIAN_POINT('Ctrl Pts',(2.33006853975684,3.35529515840789,-29.9435508645839));
#32509=CARTESIAN_POINT('Ctrl Pts',(2.38333476514479,3.31830468509675,-29.9467166641746));
#32510=CARTESIAN_POINT('Ctrl Pts',(2.43568426306117,3.2800702455178,-29.9498824637653));
#32511=CARTESIAN_POINT('Ctrl Pts',(2.4870572760686,3.24064362520074,-29.953048263356));
#32512=CARTESIAN_POINT('Ctrl Pts',(2.48705727606861,3.24064362520074,-28.7030585997167));
#32513=CARTESIAN_POINT('Ctrl Pts',(2.5820429500745,3.16774612736371,-28.7088749448307));
#32514=CARTESIAN_POINT('Ctrl Pts',(2.67379681749158,3.09068757207375,-28.7146912899448));
#32515=CARTESIAN_POINT('Ctrl Pts',(2.76194772936773,3.0097956309757,-28.7205076350588));
#32516=CARTESIAN_POINT('Ctrl Pts',(2.85019138505813,2.92881858324633,-28.7263300995654));
#32517=CARTESIAN_POINT('Ctrl Pts',(2.93482421452443,2.84400037004034,-28.7321525640719));
#32518=CARTESIAN_POINT('Ctrl Pts',(3.01551131907359,2.75570616803372,-28.7379750285785));
#32519=CARTESIAN_POINT('Ctrl Pts',(3.09624297403552,2.6673632154471,-28.7438007078887));
#32520=CARTESIAN_POINT('Ctrl Pts',(3.17302430283473,2.57554076189417,-28.7496263871989));
#32521=CARTESIAN_POINT('Ctrl Pts',(3.24556126143353,2.48063643008845,-28.7554520665091));
#32522=CARTESIAN_POINT('Ctrl Pts',(3.31821166631927,2.38558366989167,-28.7612868570599));
#32523=CARTESIAN_POINT('Ctrl Pts',(3.38660420697483,2.28743973558254,-28.7671216476108));
#32524=CARTESIAN_POINT('Ctrl Pts',(3.45048838246255,2.1866309525137,-28.7729564381616));
#32525=CARTESIAN_POINT('Ctrl Pts',(3.49920049723502,2.10976357536697,-28.7774055053182));
#32526=CARTESIAN_POINT('Ctrl Pts',(3.54529227459696,2.03134740200414,-28.7818545724747));
#32527=CARTESIAN_POINT('Ctrl Pts',(3.58867117582947,1.95157992195316,-28.7863036396313));
#32528=CARTESIAN_POINT('Ctrl Pts',(3.64540504598989,1.84725459955786,-28.7921224315145));
#32529=CARTESIAN_POINT('Ctrl Pts',(3.69767873305401,1.7402825949867,-28.7979412233978));
#32530=CARTESIAN_POINT('Ctrl Pts',(3.74523652803682,1.63108195657322,-28.803760015281));
#32531=CARTESIAN_POINT('Ctrl Pts',(3.79273386794356,1.52202013310909,-28.8095714103641));
#32532=CARTESIAN_POINT('Ctrl Pts',(3.8355270769139,1.41073568209517,-28.8153828054471));
#32533=CARTESIAN_POINT('Ctrl Pts',(3.87340569200842,1.29767227955165,-28.8211942005302));
#32534=CARTESIAN_POINT('Ctrl Pts',(3.91124607595361,1.18472299268568,-28.8269997301318));
#32535=CARTESIAN_POINT('Ctrl Pts',(3.94418160439638,1.06999871173745,-28.8328052597335));
#32536=CARTESIAN_POINT('Ctrl Pts',(3.97204964984305,0.953963615229478,-28.8386107893351));
#32537=CARTESIAN_POINT('Ctrl Pts',(4.00090495850115,0.833817818448801,-28.844621987677));
#32538=CARTESIAN_POINT('Ctrl Pts',(4.02432690494964,0.712267018809643,-28.8506331860188));
#32539=CARTESIAN_POINT('Ctrl Pts',(4.04219101456488,0.589844726831512,-28.8566443843606));
#32540=CARTESIAN_POINT('Ctrl Pts',(4.0594242412896,0.471745859367154,-28.8624432932424));
#32541=CARTESIAN_POINT('Ctrl Pts',(4.07148548363172,0.352836451920664,-28.8682422021241));
#32542=CARTESIAN_POINT('Ctrl Pts',(4.07831501460774,0.233605739709209,-28.8740411110058));
#32543=CARTESIAN_POINT('Ctrl Pts',(4.08514350486473,0.114393196486407,-28.87983913622));
#32544=CARTESIAN_POINT('Ctrl Pts',(4.08674184577814,-0.00514014580494544,
-28.8856371614342));
#32545=CARTESIAN_POINT('Ctrl Pts',(4.0831023036904,-0.124501315648307,-28.8914351866484));
#32546=CARTESIAN_POINT('Ctrl Pts',(4.07946245324251,-0.243872598364953,
-28.8972337031002));
#32547=CARTESIAN_POINT('Ctrl Pts',(4.07058385001204,-0.363071270689855,
-28.903032219552));
#32548=CARTESIAN_POINT('Ctrl Pts',(4.05651084924008,-0.481606405685688,
-28.9088307360038));
#32549=CARTESIAN_POINT('Ctrl Pts',(4.04243331929281,-0.600179689361881,
-28.9146311186175));
#32550=CARTESIAN_POINT('Ctrl Pts',(4.02315811549969,-0.718088604982401,
-28.9204315012311));
#32551=CARTESIAN_POINT('Ctrl Pts',(3.99878111898172,-0.834850023941597,
-28.9262318838448));
#32552=CARTESIAN_POINT('Ctrl Pts',(3.97437724410051,-0.951740185415469,
-28.9320386620286));
#32553=CARTESIAN_POINT('Ctrl Pts',(3.94486043195975,-1.06747992407829,-28.9378454402124));
#32554=CARTESIAN_POINT('Ctrl Pts',(3.91037712731112,-1.18159879917086,-28.9436522183963));
#32555=CARTESIAN_POINT('Ctrl Pts',(3.87587117640201,-1.29579261968403,-28.9494628100722));
#32556=CARTESIAN_POINT('Ctrl Pts',(3.83639237272657,-1.40836307167021,-28.9552734017482));
#32557=CARTESIAN_POINT('Ctrl Pts',(3.79213564343457,-1.51885886829325,-28.9610839934241));
#32558=CARTESIAN_POINT('Ctrl Pts',(3.74781584900742,-1.62951211966858,-28.9669028651008));
#32559=CARTESIAN_POINT('Ctrl Pts',(3.69870470839285,-1.7380844439387,-28.9727217367774));
#32560=CARTESIAN_POINT('Ctrl Pts',(3.64504351654909,-1.84414824850483,-28.9785406084541));
#32561=CARTESIAN_POINT('Ctrl Pts',(3.63170572170372,-1.87051101118706,-28.9799869221491));
#32562=CARTESIAN_POINT('Ctrl Pts',(3.61808703583387,-1.89671893567489,-28.9814332358441));
#32563=CARTESIAN_POINT('Ctrl Pts',(3.60419157521962,-1.92276573953145,-28.9828795495391));
#32564=CARTESIAN_POINT('Ctrl Pts',(3.54821053207587,-2.02770124983436,-28.988706355257));
#32565=CARTESIAN_POINT('Ctrl Pts',(3.48755364954155,-2.13035724183415,-28.9945331609749));
#32566=CARTESIAN_POINT('Ctrl Pts',(3.42243093206937,-2.23028955860327,-29.0003599666929));
#32567=CARTESIAN_POINT('Ctrl Pts',(3.35738987472761,-2.33009656601281,-29.0061794659326));
#32568=CARTESIAN_POINT('Ctrl Pts',(3.28789434159158,-2.42718635272648,-29.0119989651723));
#32569=CARTESIAN_POINT('Ctrl Pts',(3.21420056746468,-2.5211385745551,-29.0178184644121));
#32570=CARTESIAN_POINT('Ctrl Pts',(3.14058005737015,-2.61499739203983,-29.0236321780887));
#32571=CARTESIAN_POINT('Ctrl Pts',(3.06276985998779,-2.70572453117917,-29.0294458917653));
#32572=CARTESIAN_POINT('Ctrl Pts',(2.98106958028543,-2.79292841968727,-29.0352596054419));
#32573=CARTESIAN_POINT('Ctrl Pts',(2.89663673280179,-2.88304895103929,-29.0412677660255));
#32574=CARTESIAN_POINT('Ctrl Pts',(2.80804926529348,-2.96940604873364,-29.047275926609));
#32575=CARTESIAN_POINT('Ctrl Pts',(2.71568353120819,-3.05160416147387,-29.0532840871926));
#32576=CARTESIAN_POINT('Ctrl Pts',(2.62640662530868,-3.13105346427971,-29.0590913272081));
#32577=CARTESIAN_POINT('Ctrl Pts',(2.53360044283256,-3.20661720742733,-29.0648985672237));
#32578=CARTESIAN_POINT('Ctrl Pts',(2.43764192380558,-3.27797602970269,-29.0707058072392));
#32579=CARTESIAN_POINT('Ctrl Pts',(2.34169734481314,-3.34932448557748,-29.0765122036285));
#32580=CARTESIAN_POINT('Ctrl Pts',(2.24260166717051,-3.41646899216351,-29.0823186000178));
#32581=CARTESIAN_POINT('Ctrl Pts',(2.14076350622285,-3.47913158854684,-29.0881249964071));
#32582=CARTESIAN_POINT('Ctrl Pts',(2.03891618486954,-3.54179982146952,-29.0939319150854));
#32583=CARTESIAN_POINT('Ctrl Pts',(1.93432623706127,-3.59998512891101,-29.0997388337636));
#32584=CARTESIAN_POINT('Ctrl Pts',(1.82742918978747,-3.6534541951847,-29.1055457524419));
#32585=CARTESIAN_POINT('Ctrl Pts',(1.72049738272784,-3.70694064803118,-29.1113545593598));
#32586=CARTESIAN_POINT('Ctrl Pts',(1.61125734871256,-3.7557076273608,-29.1171633662778));
#32587=CARTESIAN_POINT('Ctrl Pts',(1.50016642568618,-3.79956914600115,-29.1229721731957));
#32588=CARTESIAN_POINT('Ctrl Pts',(1.38895336717806,-3.84347888683252,-29.1287873664269));
#32589=CARTESIAN_POINT('Ctrl Pts',(1.27588573739614,-3.88247225210961,-29.1346025596581));
#32590=CARTESIAN_POINT('Ctrl Pts',(1.16143808384948,-3.9164124626224,-29.1404177528893));
#32591=CARTESIAN_POINT('Ctrl Pts',(1.04691529150172,-3.95037495604486,-29.1462367639938));
#32592=CARTESIAN_POINT('Ctrl Pts',(0.931011065705889,-3.97927758902914,
-29.1520557750984));
#32593=CARTESIAN_POINT('Ctrl Pts',(0.814210640603455,-4.0030346029891,-29.1578747862029));
#32594=CARTESIAN_POINT('Ctrl Pts',(0.69724516002812,-4.02682518896021,-29.1637020203908));
#32595=CARTESIAN_POINT('Ctrl Pts',(0.579381353782573,-4.0454555794725,-29.1695292545787));
#32596=CARTESIAN_POINT('Ctrl Pts',(0.461110193239268,-4.05889176865938,
-29.1753564887666));
#32597=CARTESIAN_POINT('Ctrl Pts',(0.433378911481162,-4.06204217951512,
-29.1767228123267));
#32598=CARTESIAN_POINT('Ctrl Pts',(0.405625235287611,-4.06490725385444,
-29.1780891358869));
#32599=CARTESIAN_POINT('Ctrl Pts',(0.377855485250725,-4.06748696768237,
-29.179455459447));
#32600=CARTESIAN_POINT('Ctrl Pts',(0.259436741077086,-4.07848765985374,
-29.1852818828001));
#32601=CARTESIAN_POINT('Ctrl Pts',(0.140348538711738,-4.08433021474692,
-29.1911083061533));
#32602=CARTESIAN_POINT('Ctrl Pts',(0.0210772652008093,-4.08494562373744,
-29.1969347295064));
#32603=CARTESIAN_POINT('Ctrl Pts',(-0.0980447236284092,-4.08556026245753,
-29.2027538602758));
#32604=CARTESIAN_POINT('Ctrl Pts',(-0.217348923508945,-4.08096076647072,
-29.2085729910451));
#32605=CARTESIAN_POINT('Ctrl Pts',(-0.33634339722807,-4.07112983324544,
-29.2143921218145));
#32606=CARTESIAN_POINT('Ctrl Pts',(-0.455219855369642,-4.0613086500802,
-29.2202054813236));
#32607=CARTESIAN_POINT('Ctrl Pts',(-0.57378679427682,-4.04626638506521,
-29.2260188408327));
#32608=CARTESIAN_POINT('Ctrl Pts',(-0.691552442077824,-4.0260377817224,
-29.2318322003417));
#32609=CARTESIAN_POINT('Ctrl Pts',(-0.813267121606498,-4.00513085326611,
-29.2378404990506));
#32610=CARTESIAN_POINT('Ctrl Pts',(-0.934125382280565,-3.97868364374994,
-29.2438487977595));
#32611=CARTESIAN_POINT('Ctrl Pts',(-1.0535897799802,-3.94679282145912,-29.2498570964684));
#32612=CARTESIAN_POINT('Ctrl Pts',(-1.16905020009331,-3.91597085432622,
-29.2556640205935));
#32613=CARTESIAN_POINT('Ctrl Pts',(-1.28320826895366,-3.88006443957004,
-29.2614709447186));
#32614=CARTESIAN_POINT('Ctrl Pts',(-1.39558996935444,-3.83921263248563,
-29.2672778688437));
#32615=CARTESIAN_POINT('Ctrl Pts',(-1.5079556297809,-3.79836665608304,-29.2730839641602));
#32616=CARTESIAN_POINT('Ctrl Pts',(-1.61854504275882,-3.75257683041765,
-29.2788900594768));
#32617=CARTESIAN_POINT('Ctrl Pts',(-1.7269013388541,-3.70203143771956,-29.2846961547933));
#32618=CARTESIAN_POINT('Ctrl Pts',(-1.83526766642404,-3.65148136559956,
-29.2905027876301));
#32619=CARTESIAN_POINT('Ctrl Pts',(-1.94140009642179,-3.59617502350045,
-29.2963094204668));
#32620=CARTESIAN_POINT('Ctrl Pts',(-2.04486423824582,-3.53634772712517,
-29.3021160533036));
#32621=CARTESIAN_POINT('Ctrl Pts',(-2.14836230419483,-3.47650081440124,
-29.3079245900361));
#32622=CARTESIAN_POINT('Ctrl Pts',(-2.24918998908878,-3.41213020333553,
-29.3137331267685));
#32623=CARTESIAN_POINT('Ctrl Pts',(-2.34694042848864,-3.34351545908278,
-29.319541663501));
#32624=CARTESIAN_POINT('Ctrl Pts',(-2.44479875690645,-3.27482498343262,
-29.3253566112259));
#32625=CARTESIAN_POINT('Ctrl Pts',(-2.53957272641626,-3.20188125889247,
-29.3311715589508));
#32626=CARTESIAN_POINT('Ctrl Pts',(-2.6308870983957,-3.12500529207473,-29.3369865066757));
#32627=CARTESIAN_POINT('Ctrl Pts',(-2.72226164629221,-3.04807866420874,
-29.3428052864349));
#32628=CARTESIAN_POINT('Ctrl Pts',(-2.81017175667237,-2.96721490870144,
-29.3486240661942));
#32629=CARTESIAN_POINT('Ctrl Pts',(-2.8942789213397,-2.88277202107428,-29.3544428459534));
#32630=CARTESIAN_POINT('Ctrl Pts',(-2.97850527091434,-2.7982094728002,-29.3602698712733));
#32631=CARTESIAN_POINT('Ctrl Pts',(-3.05891764516055,-2.71005796986689,
-29.3660968965932));
#32632=CARTESIAN_POINT('Ctrl Pts',(-3.13521759930363,-2.61870876674303,
-29.3719239219131));
#32633=CARTESIAN_POINT('Ctrl Pts',(-3.15314544608915,-2.59724486763618,
-29.3732930710603));
#32634=CARTESIAN_POINT('Ctrl Pts',(-3.1708464403585,-2.57560455290277,-29.3746622202076));
#32635=CARTESIAN_POINT('Ctrl Pts',(-3.18831706365248,-2.55379312036477,
-29.3760313693548));
#32636=CARTESIAN_POINT('Ctrl Pts',(-3.26237872775687,-2.46132984855801,
-29.381835481924));
#32637=CARTESIAN_POINT('Ctrl Pts',(-3.33254054271542,-2.36548514299076,
-29.3876395944932));
#32638=CARTESIAN_POINT('Ctrl Pts',(-3.39847713634306,-2.26662263152769,
-29.3934437070624));
#32639=CARTESIAN_POINT('Ctrl Pts',(-3.46433414477886,-2.16787944670112,
-29.3992408140921));
#32640=CARTESIAN_POINT('Ctrl Pts',(-3.52597584417932,-2.06612603520603,
-29.4050379211218));
#32641=CARTESIAN_POINT('Ctrl Pts',(-3.58311662522096,-1.96175947813823,
-29.4108350281515));
#32642=CARTESIAN_POINT('Ctrl Pts',(-3.64020214125889,-1.85749386155564,
-29.4166265283775));
#32643=CARTESIAN_POINT('Ctrl Pts',(-3.69279519861236,-1.75062048281814,
-29.4224180286035));
#32644=CARTESIAN_POINT('Ctrl Pts',(-3.74065347945115,-1.64156527335042,
-29.4282095288295));
#32645=CARTESIAN_POINT('Ctrl Pts',(-3.78847694820317,-1.53258939058119,
-29.4339968163215));
#32646=CARTESIAN_POINT('Ctrl Pts',(-3.83157232612829,-1.4214352085985,-29.4397841038135));
#32647=CARTESIAN_POINT('Ctrl Pts',(-3.86974356700218,-1.30855253071677,
-29.4455713913055));
#32648=CARTESIAN_POINT('Ctrl Pts',(-3.90790030706425,-1.19571273565552,
-29.4513564802741));
#32649=CARTESIAN_POINT('Ctrl Pts',(-3.94113649529612,-1.08114613798668,
-29.4571415692426));
#32650=CARTESIAN_POINT('Ctrl Pts',(-3.9693047037138,-0.965321277645671,
-29.4629266582112));
#32651=CARTESIAN_POINT('Ctrl Pts',(-3.99746607423578,-0.84952453404903,
-29.4687103428364));
#32652=CARTESIAN_POINT('Ctrl Pts',(-4.02056181862068,-0.732470535382498,
-29.4744940274617));
#32653=CARTESIAN_POINT('Ctrl Pts',(-4.03849496394938,-0.61464089203007,
-29.4802777120869));
#32654=CARTESIAN_POINT('Ctrl Pts',(-4.05643362708318,-0.496774993966302,
-29.4860631762798));
#32655=CARTESIAN_POINT('Ctrl Pts',(-4.06920645404034,-0.378133380728452,
-29.4918486404727));
#32656=CARTESIAN_POINT('Ctrl Pts',(-4.07676802272873,-0.259205495421065,
-29.4976341046655));
#32657=CARTESIAN_POINT('Ctrl Pts',(-4.08232312608598,-0.171835172916947,
-29.5018843935785));
#32658=CARTESIAN_POINT('Ctrl Pts',(-4.08506673678685,-0.08431052717293,
-29.5061346824915));
#32659=CARTESIAN_POINT('Ctrl Pts',(-4.08499876708757,0.00317378213280428,
-29.5103849714045));
#32660=CARTESIAN_POINT('Ctrl Pts',(2.56728386697198,2.20447077508736,-28.0032546584631));
#32661=CARTESIAN_POINT('Ctrl Pts',(3.29391280982238,1.35834294948386,-28.0688249167149));
#32662=CARTESIAN_POINT('Ctrl Pts',(3.8330717178654,-1.09327735402418,-28.1999204782692));
#32663=CARTESIAN_POINT('Ctrl Pts',(1.19130828931765,-3.80720619125929,-28.3965413431262));
#32664=CARTESIAN_POINT('Ctrl Pts',(-2.52138985036123,-3.08713556078082,
-28.593117253034));
#32665=CARTESIAN_POINT('Ctrl Pts',(-3.96617369173339,0.405202913805355,
-28.7896931629418));
#32666=CARTESIAN_POINT('Ctrl Pts',(-1.84365258781347,3.53532882910493,-28.9862690728496));
#32667=CARTESIAN_POINT('Ctrl Pts',(1.93714903006732,3.48448758973885,-29.1828449827575));
#32668=CARTESIAN_POINT('Ctrl Pts',(3.97558571389243,0.300131850383572,-29.3794208926653));
#32669=CARTESIAN_POINT('Ctrl Pts',(2.43821705627172,-3.15447164483265,-29.5759968025731));
#32670=CARTESIAN_POINT('Ctrl Pts',(-1.29219047376943,-3.77165820795234,
-29.772572712481));
#32671=CARTESIAN_POINT('Ctrl Pts',(-3.86034553203149,-0.996531969245317,
-29.9691486223888));
#32672=CARTESIAN_POINT('Ctrl Pts',(-2.95634241771665,2.67495669448989,-30.1657245322966));
#32673=CARTESIAN_POINT('Ctrl Pts',(0.606721126975111,3.94045560524475,-30.3623004422045));
#32674=CARTESIAN_POINT('Ctrl Pts',(3.62407370691447,1.66175139044748,-30.5588763521123));
#32675=CARTESIAN_POINT('Ctrl Pts',(3.3817804106626,-2.11160786060308,-30.7554522620201));
#32676=CARTESIAN_POINT('Ctrl Pts',(0.0977699855536051,-3.98569458351054,
-30.9520281719279));
#32677=CARTESIAN_POINT('Ctrl Pts',(-3.27417889645636,-2.27487948951289,
-31.1486040818358));
#32678=CARTESIAN_POINT('Ctrl Pts',(-3.70119208770647,1.48205962121795,-31.3451799917436));
#32679=CARTESIAN_POINT('Ctrl Pts',(-0.799195750105958,3.90597094842635,
-31.5417559016514));
#32680=CARTESIAN_POINT('Ctrl Pts',(2.82163122020526,2.81668611762427,-31.7383318115593));
#32681=CARTESIAN_POINT('Ctrl Pts',(3.90456310915817,-0.806046051412663,
-31.9349077214671));
#32682=CARTESIAN_POINT('Ctrl Pts',(1.47556493170961,-3.70378608599469,-32.1314836313749));
#32683=CARTESIAN_POINT('Ctrl Pts',(-2.28061907953618,-3.27018346938094,
-32.3280595412828));
#32684=CARTESIAN_POINT('Ctrl Pts',(-3.9855173287882,0.104761205677251,-32.5246354511906));
#32685=CARTESIAN_POINT('Ctrl Pts',(-2.10567184542122,3.38547919224393,-32.7212113610984));
#32686=CARTESIAN_POINT('Ctrl Pts',(1.66810441974091,3.62115326045451,-32.9177872710062));
#32687=CARTESIAN_POINT('Ctrl Pts',(3.9415166492128,0.599808128823799,-33.1143631809141));
#32688=CARTESIAN_POINT('Ctrl Pts',(2.66976122810008,-2.96102993432676,-33.3109390908219));
#32689=CARTESIAN_POINT('Ctrl Pts',(-1.00329094829934,-3.85859178472063,
-33.5075150007297));
#32690=CARTESIAN_POINT('Ctrl Pts',(-3.77394059016891,-1.28557213310189,
-33.7040909106375));
#32691=CARTESIAN_POINT('Ctrl Pts',(-3.15014761363694,2.44374575198617,-33.9006668205454));
#32692=CARTESIAN_POINT('Ctrl Pts',(0.30702205740443,3.97505481010171,-34.0972427304532));
#32693=CARTESIAN_POINT('Ctrl Pts',(3.48804303651859,1.93103057014098,-34.2938186403611));
#32694=CARTESIAN_POINT('Ctrl Pts',(3.53176981253407,-1.84984466432527,-34.4903945502688));
#32695=CARTESIAN_POINT('Ctrl Pts',(0.398872662601994,-3.96689095901879,
-34.6869704601767));
#32696=CARTESIAN_POINT('Ctrl Pts',(-3.09278751656281,-2.51594687258676,
-34.8835463700845));
#32697=CARTESIAN_POINT('Ctrl Pts',(-3.80266311499646,1.19794680316039,-35.0801222799923));
#32698=CARTESIAN_POINT('Ctrl Pts',(-1.092261827831,3.83435618298071,-35.2766981899002));
#32699=CARTESIAN_POINT('Ctrl Pts',(2.6005661715146,3.02198261046796,-35.473274099808));
#32700=CARTESIAN_POINT('Ctrl Pts',(3.95433441888669,-0.508490640683108,
-35.6698500097158));
#32701=CARTESIAN_POINT('Ctrl Pts',(1.75140611463455,-3.58160571790905,-35.8664259196237));
#32702=CARTESIAN_POINT('Ctrl Pts',(-2.02681120527418,-3.43327248104789,
-36.0630018295315));
#32703=CARTESIAN_POINT('Ctrl Pts',(-3.98202856408726,-0.196907726104969,
-36.2595777394393));
#32704=CARTESIAN_POINT('Ctrl Pts',(-2.35563972507278,3.21656365843416,-36.4561536493472));
#32705=CARTESIAN_POINT('Ctrl Pts',(1.38951083230835,3.73692201548276,-36.6527295592549));
#32706=CARTESIAN_POINT('Ctrl Pts',(3.88487784518938,0.896131711725264,-36.8493054691628));
#32707=CARTESIAN_POINT('Ctrl Pts',(2.88601746641837,-2.75067338779994,-37.0458813790706));
#32708=CARTESIAN_POINT('Ctrl Pts',(-0.708643658991017,-3.92341407103033,
-37.2424572889785));
#32709=CARTESIAN_POINT('Ctrl Pts',(-3.66593245019103,-1.56725328617931,
-37.4390331988863));
#32710=CARTESIAN_POINT('Ctrl Pts',(-3.32590237765776,2.19853024368671,-37.6356091087942));
#32711=CARTESIAN_POINT('Ctrl Pts',(0.00553985079000487,3.98692401251902,
-37.832185018702));
#32712=CARTESIAN_POINT('Ctrl Pts',(3.33208928316455,2.18918749885435,-38.0287609286098));
#32713=CARTESIAN_POINT('Ctrl Pts',(3.66143934028185,-1.57735921247231,-38.2253368385177));
#32714=CARTESIAN_POINT('Ctrl Pts',(0.697881833191951,-3.9256293433477,-38.4219127484254));
#32715=CARTESIAN_POINT('Ctrl Pts',(-2.89406083608174,-2.74210412483044,
-38.6184886583333));
#32716=CARTESIAN_POINT('Ctrl Pts',(-3.88162410493238,0.90598402643207,-38.8150645682411));
#32717=CARTESIAN_POINT('Ctrl Pts',(-1.38054113569662,3.74274506153031,-39.0116404781489));
#32718=CARTESIAN_POINT('Ctrl Pts',(2.36774286239059,3.20596553681761,-39.2082163880568));
#32719=CARTESIAN_POINT('Ctrl Pts',(3.43742279325449,0.936456751147026,-39.339266994662));
#32720=CARTESIAN_POINT('Ctrl Pts',(3.37926985666995,-0.176560176875435,
-39.4047922979646));
#32721=CARTESIAN_POINT('Ctrl Pts',(2.74548793878474,2.35749073262566,-27.8676427113695));
#32722=CARTESIAN_POINT('Ctrl Pts',(3.52255471516762,1.45263024183603,-27.9332129696212));
#32723=CARTESIAN_POINT('Ctrl Pts',(4.09913851182676,-1.1691655246368,-28.0643085311756));
#32724=CARTESIAN_POINT('Ctrl Pts',(1.27400112693951,-4.07147756936497,-28.2609293960326));
#32725=CARTESIAN_POINT('Ctrl Pts',(-2.69640825940523,-3.30142434054789,
-28.4575053059404));
#32726=CARTESIAN_POINT('Ctrl Pts',(-4.24147955505312,0.433329452549069,
-28.6540812158482));
#32727=CARTESIAN_POINT('Ctrl Pts',(-1.97162690432098,3.78072825713415,-28.8506571257561));
#32728=CARTESIAN_POINT('Ctrl Pts',(2.07161325870492,3.72635795112,-29.0472330356639));
#32729=CARTESIAN_POINT('Ctrl Pts',(4.25154489829376,0.320965042422498,-29.2438089455717));
#32730=CARTESIAN_POINT('Ctrl Pts',(2.60746215338809,-3.37343445559113,-29.4403848554795));
#32731=CARTESIAN_POINT('Ctrl Pts',(-1.38188589348746,-4.03346207732183,
-29.6369607653874));
#32732=CARTESIAN_POINT('Ctrl Pts',(-4.12830549596942,-1.06570470736585,
-29.8335366752952));
#32733=CARTESIAN_POINT('Ctrl Pts',(-3.16155239207421,2.86063471047149,-30.0301125852031));
#32734=CARTESIAN_POINT('Ctrl Pts',(0.648835743388491,4.21397628703841,-30.2266884951108));
#32735=CARTESIAN_POINT('Ctrl Pts',(3.87563322451603,1.7770993143479,-30.4232644050187));
#32736=CARTESIAN_POINT('Ctrl Pts',(3.61652151074496,-2.25818188136967,-30.6198403149265));
#32737=CARTESIAN_POINT('Ctrl Pts',(0.104556539136899,-4.26235545959098,
-30.8164162248343));
#32738=CARTESIAN_POINT('Ctrl Pts',(-3.50145100247405,-2.43278675996705,
-31.0129921347422));
#32739=CARTESIAN_POINT('Ctrl Pts',(-3.95810465942314,1.58493451657646,-31.20956804465));
#32740=CARTESIAN_POINT('Ctrl Pts',(-0.854670697257917,4.17709793066106,
-31.4061439545578));
#32741=CARTESIAN_POINT('Ctrl Pts',(3.01749042341354,3.0122020641219,-31.6027198644657));
#32742=CARTESIAN_POINT('Ctrl Pts',(4.17559236838947,-0.861996501722528,
-31.7992957743735));
#32743=CARTESIAN_POINT('Ctrl Pts',(1.57798900815773,-3.96087871612375,-31.9958716842813));
#32744=CARTESIAN_POINT('Ctrl Pts',(-2.43892475482816,-3.49717823895654,
-32.1924475941892));
#32745=CARTESIAN_POINT('Ctrl Pts',(-4.26216590100397,0.112033044081982,
-32.3890235040969));
#32746=CARTESIAN_POINT('Ctrl Pts',(-2.2518338267989,3.62047703757641,-32.5855994140048));
#32747=CARTESIAN_POINT('Ctrl Pts',(1.78389332942519,3.87251005974457,-32.7821753239126));
#32748=CARTESIAN_POINT('Ctrl Pts',(4.21511098174603,0.64144289007397,-32.9787512338205));
#32749=CARTESIAN_POINT('Ctrl Pts',(2.85507860875126,-3.1665652854599,-33.1753271437283));
#32750=CARTESIAN_POINT('Ctrl Pts',(-1.07293285058369,-4.12643001497894,
-33.3719030536361));
#32751=CARTESIAN_POINT('Ctrl Pts',(-4.03590288759914,-1.37480815085398,
-33.5684789635439));
#32752=CARTESIAN_POINT('Ctrl Pts',(-3.36881027840236,2.6133746150354,-33.7650548734518));
#32753=CARTESIAN_POINT('Ctrl Pts',(0.328333522595203,4.25097714263074,-33.9616307833595));
#32754=CARTESIAN_POINT('Ctrl Pts',(3.73016019378445,2.06507009526757,-34.1582066932675));
#32755=CARTESIAN_POINT('Ctrl Pts',(3.77692219688698,-1.97824879432617,-34.3547826031752));
#32756=CARTESIAN_POINT('Ctrl Pts',(0.426559796668051,-4.24224661034696,
-34.5513585130831));
#32757=CARTESIAN_POINT('Ctrl Pts',(-3.30746861817128,-2.69058746567722,
-34.7479344229909));
#32758=CARTESIAN_POINT('Ctrl Pts',(-4.06661914243173,1.28110044303818,-34.9445103328988));
#32759=CARTESIAN_POINT('Ctrl Pts',(-1.16807950725057,4.10051213611788,-35.1410862428066));
#32760=CARTESIAN_POINT('Ctrl Pts',(2.78108048344732,3.23174889812353,-35.3376621527144));
#32761=CARTESIAN_POINT('Ctrl Pts',(4.22881847724137,-0.54378673856078,-35.5342380626223));
#32762=CARTESIAN_POINT('Ctrl Pts',(1.87297728369805,-3.83021738519307,-35.7308139725301));
#32763=CARTESIAN_POINT('Ctrl Pts',(-2.16749919627598,-3.67158782421524,
-35.9273898824379));
#32764=CARTESIAN_POINT('Ctrl Pts',(-4.25843496905253,-0.210575773886802,
-36.1239657923457));
#32765=CARTESIAN_POINT('Ctrl Pts',(-2.51915284340472,3.43983649107734,-36.3205417022536));
#32766=CARTESIAN_POINT('Ctrl Pts',(1.48596159544011,3.99631472533188,-36.5171176121614));
#32767=CARTESIAN_POINT('Ctrl Pts',(4.15454068201641,0.958335319968377,-36.7136935220692));
#32768=CARTESIAN_POINT('Ctrl Pts',(3.08634594214907,-2.94160716191005,-36.910269431977));
#32769=CARTESIAN_POINT('Ctrl Pts',(-0.757833071631014,-4.19575184086556,
-37.1068453418849));
#32770=CARTESIAN_POINT('Ctrl Pts',(-3.92039752825235,-1.67604176911731,
-37.3034212517927));
#32771=CARTESIAN_POINT('Ctrl Pts',(-3.55676478978729,2.35113784834968,-37.4999971617006));
#32772=CARTESIAN_POINT('Ctrl Pts',(0.00592439103532244,4.26367022752833,
-37.6965730716083));
#32773=CARTESIAN_POINT('Ctrl Pts',(3.56338114985008,2.34114659121509,-37.8931489815162));
#32774=CARTESIAN_POINT('Ctrl Pts',(3.91559253601055,-1.68684918278303,-38.089724891424));
#32775=CARTESIAN_POINT('Ctrl Pts',(0.746324230201072,-4.19812088291295,
-38.2863008013318));
#32776=CARTESIAN_POINT('Ctrl Pts',(-3.09494762998035,-2.93244307669544,
-38.4828767112397));
#32777=CARTESIAN_POINT('Ctrl Pts',(-4.15106108837021,0.968871517988643,
-38.6794526211475));
#32778=CARTESIAN_POINT('Ctrl Pts',(-1.47636928109619,4.00254196918918,-38.8760285310553));
#32779=CARTESIAN_POINT('Ctrl Pts',(2.53209610143512,3.42850271710462,-39.0726044409632));
#32780=CARTESIAN_POINT('Ctrl Pts',(3.67602622397774,1.00145946014927,-39.2036550475684));
#32781=CARTESIAN_POINT('Ctrl Pts',(3.61383669049771,-0.188815830737465,
-39.269180350871));
#32782=CARTESIAN_POINT('Ctrl Pts',(2.92369201059751,2.51051069016395,-27.7320307642759));
#32783=CARTESIAN_POINT('Ctrl Pts',(3.75119662051287,1.54691753418819,-27.7976010225276));
#32784=CARTESIAN_POINT('Ctrl Pts',(4.36520530578812,-1.24505369524941,-27.9286965840819));
#32785=CARTESIAN_POINT('Ctrl Pts',(1.35669396456135,-4.33574894747066,-28.125317448939));
#32786=CARTESIAN_POINT('Ctrl Pts',(-2.87142666844923,-3.51571312031497,
-28.3218933588468));
#32787=CARTESIAN_POINT('Ctrl Pts',(-4.51678541837286,0.461455991292788,
-28.5184692687547));
#32788=CARTESIAN_POINT('Ctrl Pts',(-2.0996012208285,4.02612768516337,-28.7150451786624));
#32789=CARTESIAN_POINT('Ctrl Pts',(2.20607748734252,3.96822831250115,-28.9116210885703));
#32790=CARTESIAN_POINT('Ctrl Pts',(4.52750408269509,0.341798234461419,-29.1081969984781));
#32791=CARTESIAN_POINT('Ctrl Pts',(2.77670725050445,-3.59239726634962,-29.304772908386));
#32792=CARTESIAN_POINT('Ctrl Pts',(-1.47158131320549,-4.29526594669133,
-29.5013488182938));
#32793=CARTESIAN_POINT('Ctrl Pts',(-4.39626545990734,-1.13487744548638,
-29.6979247282016));
#32794=CARTESIAN_POINT('Ctrl Pts',(-3.36676236643178,3.04631272645307,-29.8945006381094));
#32795=CARTESIAN_POINT('Ctrl Pts',(0.690950359801877,4.48749696883208,-30.0910765480173));
#32796=CARTESIAN_POINT('Ctrl Pts',(4.12719274211759,1.89244723824832,-30.287652457925));
#32797=CARTESIAN_POINT('Ctrl Pts',(3.85126261082733,-2.40475590213628,-30.484228367833));
#32798=CARTESIAN_POINT('Ctrl Pts',(0.111343092720193,-4.53901633567143,
-30.6808042777407));
#32799=CARTESIAN_POINT('Ctrl Pts',(-3.72872310849174,-2.59069403042121,
-30.8773801876486));
#32800=CARTESIAN_POINT('Ctrl Pts',(-4.2150172311398,1.68780941193497,-31.0739560975564));
#32801=CARTESIAN_POINT('Ctrl Pts',(-0.910145644409873,4.44822491289575,
-31.2705320074642));
#32802=CARTESIAN_POINT('Ctrl Pts',(3.21334962662181,3.20771801061954,-31.4671079173721));
#32803=CARTESIAN_POINT('Ctrl Pts',(4.44662162762077,-0.917946952032398,
-31.6636838272799));
#32804=CARTESIAN_POINT('Ctrl Pts',(1.68041308460585,-4.2179713462528,-31.8602597371878));
#32805=CARTESIAN_POINT('Ctrl Pts',(-2.59723043012015,-3.72417300853216,
-32.0568356470955));
#32806=CARTESIAN_POINT('Ctrl Pts',(-4.53881447321974,0.119304882486721,
-32.2534115570034));
#32807=CARTESIAN_POINT('Ctrl Pts',(-2.39799580817657,3.85547488290889,-32.4499874669112));
#32808=CARTESIAN_POINT('Ctrl Pts',(1.89968223910945,4.12386685903462,-32.6465633768191));
#32809=CARTESIAN_POINT('Ctrl Pts',(4.48870531427926,0.683077651324139,-32.8431392867268));
#32810=CARTESIAN_POINT('Ctrl Pts',(3.04039598940244,-3.37210063659303,-33.0397151966347));
#32811=CARTESIAN_POINT('Ctrl Pts',(-1.14257475286803,-4.39426824523726,
-33.2362911065425));
#32812=CARTESIAN_POINT('Ctrl Pts',(-4.29786518502939,-1.46404416860608,
-33.4328670164504));
#32813=CARTESIAN_POINT('Ctrl Pts',(-3.58747294316779,2.78300347808462,-33.6294429263582));
#32814=CARTESIAN_POINT('Ctrl Pts',(0.349644987785975,4.52689947515976,-33.826018836266));
#32815=CARTESIAN_POINT('Ctrl Pts',(3.97227735105031,2.19910962039414,-34.0225947461739));
#32816=CARTESIAN_POINT('Ctrl Pts',(4.02207458123991,-2.10665292432707,-34.2191706560816));
#32817=CARTESIAN_POINT('Ctrl Pts',(0.454246930734107,-4.51760226167515,
-34.4157465659895));
#32818=CARTESIAN_POINT('Ctrl Pts',(-3.52214971977974,-2.86522805876768,
-34.6123224758973));
#32819=CARTESIAN_POINT('Ctrl Pts',(-4.330575169867,1.36425408291597,-34.8088983858051));
#32820=CARTESIAN_POINT('Ctrl Pts',(-1.24389718667016,4.36666808925506,-35.005474295713));
#32821=CARTESIAN_POINT('Ctrl Pts',(2.96159479538005,3.4415151857791,-35.2020502056208));
#32822=CARTESIAN_POINT('Ctrl Pts',(4.50330253559606,-0.579082836438446,
-35.3986261155287));
#32823=CARTESIAN_POINT('Ctrl Pts',(1.99454845276156,-4.0788290524771,-35.5952020254364));
#32824=CARTESIAN_POINT('Ctrl Pts',(-2.30818718727777,-3.9099031673826,-35.7917779353443));
#32825=CARTESIAN_POINT('Ctrl Pts',(-4.53484137401781,-0.224243821668637,
-35.9883538452521));
#32826=CARTESIAN_POINT('Ctrl Pts',(-2.68266596173667,3.6631093237205,-36.18492975516));
#32827=CARTESIAN_POINT('Ctrl Pts',(1.58241235857187,4.25570743518099,-36.3815056650678));
#32828=CARTESIAN_POINT('Ctrl Pts',(4.42420351884345,1.02053892821149,-36.5780815749756));
#32829=CARTESIAN_POINT('Ctrl Pts',(3.28667441787977,-3.13254093602017,-36.7746574848834));
#32830=CARTESIAN_POINT('Ctrl Pts',(-0.807022484271015,-4.46808961070079,
-36.9712333947913));
#32831=CARTESIAN_POINT('Ctrl Pts',(-4.17486260631367,-1.78483025205532,
-37.1678093046991));
#32832=CARTESIAN_POINT('Ctrl Pts',(-3.78762720191682,2.50374545301266,-37.364385214607));
#32833=CARTESIAN_POINT('Ctrl Pts',(0.00630893128064401,4.54041644253765,
-37.5609611245147));
#32834=CARTESIAN_POINT('Ctrl Pts',(3.79467301653562,2.49310568357585,-37.7575370344226));
#32835=CARTESIAN_POINT('Ctrl Pts',(4.16974573173925,-1.79633915309375,-37.9541129443304));
#32836=CARTESIAN_POINT('Ctrl Pts',(0.794766627210192,-4.4706124224782,-38.1506888542383));
#32837=CARTESIAN_POINT('Ctrl Pts',(-3.29583442387897,-3.12278202856045,
-38.3472647641461));
#32838=CARTESIAN_POINT('Ctrl Pts',(-4.42049807180803,1.03175900954522,-38.5438406740539));
#32839=CARTESIAN_POINT('Ctrl Pts',(-1.57219742649575,4.26233887684804,-38.7404165839617));
#32840=CARTESIAN_POINT('Ctrl Pts',(2.69644934047965,3.65103989739164,-38.9369924938696));
#32841=CARTESIAN_POINT('Ctrl Pts',(3.91462965470099,1.06646216915153,-39.0680431004748));
#32842=CARTESIAN_POINT('Ctrl Pts',(3.84840352432548,-0.201071484599496,
-39.1335684037774));
#32843=CARTESIAN_POINT('Ctrl Pts',(3.10189608241027,2.66353064770225,-27.5964188171822));
#32844=CARTESIAN_POINT('Ctrl Pts',(3.97983852585811,1.64120482654036,-27.661989075434));
#32845=CARTESIAN_POINT('Ctrl Pts',(4.63127209974949,-1.32094186586204,-27.7930846369884));
#32846=CARTESIAN_POINT('Ctrl Pts',(1.4393868021832,-4.60002032557634,-27.9897055018454));
#32847=CARTESIAN_POINT('Ctrl Pts',(-3.04644507749322,-3.73000190008205,
-28.1862814117532));
#32848=CARTESIAN_POINT('Ctrl Pts',(-4.7920912816926,0.489582530036508,-28.3828573216609));
#32849=CARTESIAN_POINT('Ctrl Pts',(-2.22757553733602,4.27152711319258,-28.5794332315689));
#32850=CARTESIAN_POINT('Ctrl Pts',(2.34054171598012,4.2100986738823,-28.7760091414767));
#32851=CARTESIAN_POINT('Ctrl Pts',(4.80346326709643,0.362631426500339,-28.9725850513845));
#32852=CARTESIAN_POINT('Ctrl Pts',(2.94595234762082,-3.81136007710809,-29.1691609612924));
#32853=CARTESIAN_POINT('Ctrl Pts',(-1.56127673292352,-4.55706981606083,
-29.3657368712001));
#32854=CARTESIAN_POINT('Ctrl Pts',(-4.66422542384527,-1.2040501836069,-29.562312781108));
#32855=CARTESIAN_POINT('Ctrl Pts',(-3.57197234078933,3.23199074243467,-29.7588886910158));
#32856=CARTESIAN_POINT('Ctrl Pts',(0.73306497621526,4.76101765062574,-29.9554646009237));
#32857=CARTESIAN_POINT('Ctrl Pts',(4.37875225971916,2.00779516214874,-30.1520405108315));
#32858=CARTESIAN_POINT('Ctrl Pts',(4.0860037109097,-2.55132992290288,-30.3486164207393));
#32859=CARTESIAN_POINT('Ctrl Pts',(0.118129646303484,-4.81567721175188,
-30.5451923306472));
#32860=CARTESIAN_POINT('Ctrl Pts',(-3.95599521450942,-2.74860130087537,
-30.7417682405549));
#32861=CARTESIAN_POINT('Ctrl Pts',(-4.47192980285647,1.79068430729347,-30.9383441504629));
#32862=CARTESIAN_POINT('Ctrl Pts',(-0.965620591561828,4.71935189513045,
-31.1349200603706));
#32863=CARTESIAN_POINT('Ctrl Pts',(3.40920882983009,3.40323395711717,-31.3314959702785));
#32864=CARTESIAN_POINT('Ctrl Pts',(4.71765088685207,-0.973897402342265,
-31.5280718801863));
#32865=CARTESIAN_POINT('Ctrl Pts',(1.78283716105399,-4.47506397638186,-31.7246477900941));
#32866=CARTESIAN_POINT('Ctrl Pts',(-2.75553610541214,-3.95116777810775,
-31.921223700002));
#32867=CARTESIAN_POINT('Ctrl Pts',(-4.81546304543552,0.126576720891454,
-32.1177996099098));
#32868=CARTESIAN_POINT('Ctrl Pts',(-2.54415778955425,4.09047272824138,-32.3143755198176));
#32869=CARTESIAN_POINT('Ctrl Pts',(2.01547114879372,4.37522365832467,-32.5109514297255));
#32870=CARTESIAN_POINT('Ctrl Pts',(4.7622996468125,0.724712412574313,-32.7075273396332));
#32871=CARTESIAN_POINT('Ctrl Pts',(3.22571337005362,-3.57763598772617,-32.9041032495411));
#32872=CARTESIAN_POINT('Ctrl Pts',(-1.21221665515238,-4.66210647549557,
-33.1006791594489));
#32873=CARTESIAN_POINT('Ctrl Pts',(-4.55982748245962,-1.55328018635817,
-33.2972550693568));
#32874=CARTESIAN_POINT('Ctrl Pts',(-3.80613560793321,2.95263234113385,-33.4938309792646));
#32875=CARTESIAN_POINT('Ctrl Pts',(0.370956452976748,4.80282180768878,-33.6904068891724));
#32876=CARTESIAN_POINT('Ctrl Pts',(4.21439450831618,2.33314914552072,-33.8869827990801));
#32877=CARTESIAN_POINT('Ctrl Pts',(4.26722696559284,-2.23505705432797,-34.0835587089881));
#32878=CARTESIAN_POINT('Ctrl Pts',(0.48193406480016,-4.79295791300333,-34.2801346188959));
#32879=CARTESIAN_POINT('Ctrl Pts',(-3.73683082138821,-3.03986865185813,
-34.4767105288038));
#32880=CARTESIAN_POINT('Ctrl Pts',(-4.59453119730227,1.44740772279378,-34.6732864387115));
#32881=CARTESIAN_POINT('Ctrl Pts',(-1.31971486608973,4.63282404239223,-34.8698623486193));
#32882=CARTESIAN_POINT('Ctrl Pts',(3.14210910731277,3.65128147343468,-35.0664382585272));
#32883=CARTESIAN_POINT('Ctrl Pts',(4.77778659395074,-0.614378934316126,
-35.263014168435));
#32884=CARTESIAN_POINT('Ctrl Pts',(2.11611962182505,-4.32744071976112,-35.4595900783428));
#32885=CARTESIAN_POINT('Ctrl Pts',(-2.44887517827956,-4.14821851054996,
-35.6561659882507));
#32886=CARTESIAN_POINT('Ctrl Pts',(-4.81124777898309,-0.237911869450464,
-35.8527418981585));
#32887=CARTESIAN_POINT('Ctrl Pts',(-2.84617908006861,3.88638215636366,-36.0493178080664));
#32888=CARTESIAN_POINT('Ctrl Pts',(1.67886312170362,4.51510014503012,-36.2458937179742));
#32889=CARTESIAN_POINT('Ctrl Pts',(4.69386635567049,1.0827425364546,-36.442469627882));
#32890=CARTESIAN_POINT('Ctrl Pts',(3.48700289361047,-3.32347471013028,-36.6390455377899));
#32891=CARTESIAN_POINT('Ctrl Pts',(-0.856211896911012,-4.74042738053602,
-36.8356214476976));
#32892=CARTESIAN_POINT('Ctrl Pts',(-4.42932768437499,-1.89361873499331,
-37.0321973576056));
#32893=CARTESIAN_POINT('Ctrl Pts',(-4.01848961404635,2.65635305767562,-37.2287732675133));
#32894=CARTESIAN_POINT('Ctrl Pts',(0.00669347152596622,4.81716265754697,
-37.4253491774212));
#32895=CARTESIAN_POINT('Ctrl Pts',(4.02596488322114,2.64506477593659,-37.621925087329));
#32896=CARTESIAN_POINT('Ctrl Pts',(4.42389892746796,-1.90582912340446,-37.8185009972368));
#32897=CARTESIAN_POINT('Ctrl Pts',(0.843209024219307,-4.74310396204345,
-38.0150769071447));
#32898=CARTESIAN_POINT('Ctrl Pts',(-3.49672121777756,-3.31312098042544,
-38.2116528170525));
#32899=CARTESIAN_POINT('Ctrl Pts',(-4.68993505524586,1.09464650110178,-38.4082287269604));
#32900=CARTESIAN_POINT('Ctrl Pts',(-1.66802557189533,4.52213578450691,-38.6048046368681));
#32901=CARTESIAN_POINT('Ctrl Pts',(2.86080257952418,3.87357707767866,-38.801380546776));
#32902=CARTESIAN_POINT('Ctrl Pts',(4.15323308542423,1.13146487815378,-38.9324311533812));
#32903=CARTESIAN_POINT('Ctrl Pts',(4.08297035815325,-0.213327138461527,
-38.9979564566838));
#32904=CARTESIAN_POINT('Ctrl Pts',(4.07943565862452,-0.213142457391218,
-39.));
#32905=CARTESIAN_POINT('Ctrl Pts',(4.07547862263307,-0.0893448369054089,
-39.));
#32906=CARTESIAN_POINT('Ctrl Pts',(4.06544764788375,0.0339030770314181,
-39.));
#32907=CARTESIAN_POINT('Ctrl Pts',(4.04961725587858,0.156269764503743,-39.));
#32908=CARTESIAN_POINT('Ctrl Pts',(4.03355455981531,0.280432129434245,-39.));
#32909=CARTESIAN_POINT('Ctrl Pts',(4.01152059276709,0.403687980955931,-39.));
#32910=CARTESIAN_POINT('Ctrl Pts',(3.98374860021197,0.525679242089098,-39.));
#32911=CARTESIAN_POINT('Ctrl Pts',(3.9558662643795,0.648155197128751,-39.));
#32912=CARTESIAN_POINT('Ctrl Pts',(3.9221997260414,0.769357256097345,-39.));
#32913=CARTESIAN_POINT('Ctrl Pts',(3.88293829909243,0.888899762117013,-39.));
#32914=CARTESIAN_POINT('Ctrl Pts',(3.84594470302387,1.00153721634053,-39.));
#32915=CARTESIAN_POINT('Ctrl Pts',(3.80398315981906,1.11270162038201,-39.));
#32916=CARTESIAN_POINT('Ctrl Pts',(3.75718016985247,1.22204245191786,-39.));
#32917=CARTESIAN_POINT('Ctrl Pts',(3.74832861001601,1.24272140669402,-39.));
#32918=CARTESIAN_POINT('Ctrl Pts',(3.73930380307158,1.26333504411753,-39.));
#32919=CARTESIAN_POINT('Ctrl Pts',(3.73010649791783,1.28388085829669,-39.));
#32920=CARTESIAN_POINT('Ctrl Pts',(3.72331964578407,1.29904197347889,-39.));
#32921=CARTESIAN_POINT('Ctrl Pts',(3.71643932891027,1.31416499535076,-39.));
#32922=CARTESIAN_POINT('Ctrl Pts',(3.70947119635962,1.32923777417663,-39.));
#32923=CARTESIAN_POINT('Ctrl Pts',(3.65772911496908,1.44116115438239,-39.));
#32924=CARTESIAN_POINT('Ctrl Pts',(3.60107392087828,1.55048480765739,-39.));
#32925=CARTESIAN_POINT('Ctrl Pts',(3.53972500093587,1.65686661310373,-39.));
#32926=CARTESIAN_POINT('Ctrl Pts',(3.47866871745544,1.76274097367257,-39.));
#32927=CARTESIAN_POINT('Ctrl Pts',(3.41296282504321,1.86570215783094,-39.));
#32928=CARTESIAN_POINT('Ctrl Pts',(3.34278310915447,1.96538145265714,-39.));
#32929=CARTESIAN_POINT('Ctrl Pts',(3.27420369022065,2.06278777629846,-39.));
#32930=CARTESIAN_POINT('Ctrl Pts',(3.20135157516031,2.15706065609363,-39.));
#32931=CARTESIAN_POINT('Ctrl Pts',(3.12436054260474,2.2478176249695,-39.));
#32932=CARTESIAN_POINT('Ctrl Pts',(3.05951101564277,2.32426219656105,-39.));
#32933=CARTESIAN_POINT('Ctrl Pts',(2.99172440946438,2.39821187176379,-39.));
#32934=CARTESIAN_POINT('Ctrl Pts',(2.92106768956024,2.46941240302989,-39.));
#32935=CARTESIAN_POINT('Ctrl Pts',(2.90675811120593,2.48383211544229,-39.));
#32936=CARTESIAN_POINT('Ctrl Pts',(2.89233078089546,2.4981389856815,-39.));
#32937=CARTESIAN_POINT('Ctrl Pts',(2.87778620684771,2.51233076884828,-39.));
#32938=CARTESIAN_POINT('Ctrl Pts',(2.86578714363673,2.52403878468538,-39.));
#32939=CARTESIAN_POINT('Ctrl Pts',(2.85370820051999,2.5356684616658,-39.));
#32940=CARTESIAN_POINT('Ctrl Pts',(2.84156035651544,2.54720861596515,-39.));
#32941=CARTESIAN_POINT('Ctrl Pts',(2.75684747169488,2.62768378189632,-39.));
#32942=CARTESIAN_POINT('Ctrl Pts',(2.66865995789381,2.7039333039484,-39.));
#32943=CARTESIAN_POINT('Ctrl Pts',(2.5771544005093,2.77562846691384,-39.));
#32944=CARTESIAN_POINT('Ctrl Pts',(2.48616555011133,2.84691878680019,-39.));
#32945=CARTESIAN_POINT('Ctrl Pts',(2.39189554495299,2.91370656208833,-39.));
#32946=CARTESIAN_POINT('Ctrl Pts',(2.29447234532102,2.97562460420606,-39.));
#32947=CARTESIAN_POINT('Ctrl Pts',(2.27139641425051,2.99029068453731,-39.));
#32948=CARTESIAN_POINT('Ctrl Pts',(2.24814347894285,3.0046833385606,-39.));
#32949=CARTESIAN_POINT('Ctrl Pts',(2.22471506914856,3.01879727283302,-39.));
#32950=CARTESIAN_POINT('Ctrl Pts',(2.12317225035552,3.07996952834948,-39.));
#32951=CARTESIAN_POINT('Ctrl Pts',(2.01833364786956,3.13591009017389,-39.));
#32952=CARTESIAN_POINT('Ctrl Pts',(1.91064248930382,3.18656524692859,-39.));
#32953=CARTESIAN_POINT('Ctrl Pts',(1.85027201234174,3.21496196969207,-39.));
#32954=CARTESIAN_POINT('Ctrl Pts',(1.78900493758425,3.24169676584405,-39.));
#32955=CARTESIAN_POINT('Ctrl Pts',(1.72691930409674,3.26675302213736,-39.));
#32956=CARTESIAN_POINT('Ctrl Pts',(1.7081799729301,3.2743157618261,-39.));
#32957=CARTESIAN_POINT('Ctrl Pts',(1.68936607397445,3.28172554844747,-39.));
#32958=CARTESIAN_POINT('Ctrl Pts',(1.67047976756002,3.28898183330933,-39.));
#32959=CARTESIAN_POINT('Ctrl Pts',(1.65401551208684,3.29530754491912,-39.));
#32960=CARTESIAN_POINT('Ctrl Pts',(1.63749558785105,3.30151676005302,-39.));
#32961=CARTESIAN_POINT('Ctrl Pts',(1.62093733317381,3.30760347428902,-39.));
#32962=CARTESIAN_POINT('Ctrl Pts',(1.51232751810485,3.34752778518023,-39.));
#32963=CARTESIAN_POINT('Ctrl Pts',(1.40192140847811,3.3822442337368,-39.));
#32964=CARTESIAN_POINT('Ctrl Pts',(1.29014212257712,3.41176730634751,-39.));
#32965=CARTESIAN_POINT('Ctrl Pts',(1.1774449041267,3.44153282270878,-39.));
#32966=CARTESIAN_POINT('Ctrl Pts',(1.06335174640429,3.46601902640531,-39.));
#32967=CARTESIAN_POINT('Ctrl Pts',(0.948291874745636,3.48518748998652,-39.));
#32968=CARTESIAN_POINT('Ctrl Pts',(0.834769919331161,3.50409974355208,-39.));
#32969=CARTESIAN_POINT('Ctrl Pts',(0.720306022442315,3.51783531415529,-39.));
#32970=CARTESIAN_POINT('Ctrl Pts',(0.605319480240082,3.52630781742824,-39.));
#32971=CARTESIAN_POINT('Ctrl Pts',(0.521444284469331,3.53248795692175,-39.));
#32972=CARTESIAN_POINT('Ctrl Pts',(0.437291099039107,3.53586672787097,-39.));
#32973=CARTESIAN_POINT('Ctrl Pts',(0.353029136599959,3.53639426684562,-39.));
#32974=CARTESIAN_POINT('Ctrl Pts',(0.327898163577327,3.53655160436016,-39.));
#32975=CARTESIAN_POINT('Ctrl Pts',(0.302757563702177,3.53645522658894,-39.));
#32976=CARTESIAN_POINT('Ctrl Pts',(0.277611962535154,3.53610357479034,-39.));
#32977=CARTESIAN_POINT('Ctrl Pts',(0.258741040287152,3.53583967202238,-39.));
#32978=CARTESIAN_POINT('Ctrl Pts',(0.239875829455418,3.53543209444648,-39.));
#32979=CARTESIAN_POINT('Ctrl Pts',(0.221022502202154,3.53488072125031,-39.));
#32980=CARTESIAN_POINT('Ctrl Pts',(0.107579683538356,3.53156304004373,-39.));
#32981=CARTESIAN_POINT('Ctrl Pts',(-0.00548437432396109,3.52304246054611,
-39.));
#32982=CARTESIAN_POINT('Ctrl Pts',(-0.117759280560823,3.50925106599073,
-39.));
#32983=CARTESIAN_POINT('Ctrl Pts',(-0.227468089891742,3.49577488038169,
-39.));
#32984=CARTESIAN_POINT('Ctrl Pts',(-0.336424125111459,3.47726582969332,
-39.));
#32985=CARTESIAN_POINT('Ctrl Pts',(-0.444223733781713,3.45361539240257,
-39.));
#32986=CARTESIAN_POINT('Ctrl Pts',(-0.469784016719349,3.44800765526691,
-39.));
#32987=CARTESIAN_POINT('Ctrl Pts',(-0.495279164302631,3.44211066994351,
-39.));
#32988=CARTESIAN_POINT('Ctrl Pts',(-0.520703552750254,3.43592262669056,
-39.));
#32989=CARTESIAN_POINT('Ctrl Pts',(-0.544842672211385,3.43004740512441,
-39.));
#32990=CARTESIAN_POINT('Ctrl Pts',(-0.568920339517025,3.42390906587648,
-39.));
#32991=CARTESIAN_POINT('Ctrl Pts',(-0.592909343325201,3.41751225292074,
-39.));
#32992=CARTESIAN_POINT('Ctrl Pts',(-0.696930171154229,3.38977447004135,
-39.));
#32993=CARTESIAN_POINT('Ctrl Pts',(-0.79937645949779,3.35715927661756,-39.));
#32994=CARTESIAN_POINT('Ctrl Pts',(-0.899875244423881,3.31958176012196,
-39.));
#32995=CARTESIAN_POINT('Ctrl Pts',(-0.994995238784878,3.28401542805347,
-39.));
#32996=CARTESIAN_POINT('Ctrl Pts',(-1.0883709659824,3.24400334859258,-39.));
#32997=CARTESIAN_POINT('Ctrl Pts',(-1.17966135005092,3.19943835339881,-39.));
#32998=CARTESIAN_POINT('Ctrl Pts',(-1.22188181501936,3.17882769612537,-39.));
#32999=CARTESIAN_POINT('Ctrl Pts',(-1.26365583302969,3.15724268359402,-39.));
#33000=CARTESIAN_POINT('Ctrl Pts',(-1.30496166320995,3.13470830288176,-39.));
#33001=CARTESIAN_POINT('Ctrl Pts',(2.57323442701465,2.20655152809233,-28.));
#33002=CARTESIAN_POINT('Ctrl Pts',(2.65146086060648,2.13210309013611,-28.));
#33003=CARTESIAN_POINT('Ctrl Pts',(2.72559006808564,2.05386847221022,-28.));
#33004=CARTESIAN_POINT('Ctrl Pts',(2.79562474081432,1.97228873410646,-28.));
#33005=CARTESIAN_POINT('Ctrl Pts',(2.8662200815952,1.89005590302633,-28.));
#33006=CARTESIAN_POINT('Ctrl Pts',(2.93265540757401,1.8044236111313,-28.));
#33007=CARTESIAN_POINT('Ctrl Pts',(2.99490662467184,1.71579430777158,-28.));
#33008=CARTESIAN_POINT('Ctrl Pts',(3.05871119030977,1.62495344606167,-28.));
#33009=CARTESIAN_POINT('Ctrl Pts',(3.11812071413516,1.5309636073814,-28.));
#33010=CARTESIAN_POINT('Ctrl Pts',(3.17307474355074,1.43421476081748,-28.));
#33011=CARTESIAN_POINT('Ctrl Pts',(3.22407555773482,1.34442571352461,-28.));
#33012=CARTESIAN_POINT('Ctrl Pts',(3.27123873365936,1.25225942026066,-28.));
#33013=CARTESIAN_POINT('Ctrl Pts',(3.31448495636522,1.15800209474407,-28.));
#33014=CARTESIAN_POINT('Ctrl Pts',(3.32156241408425,1.1425764183656,-28.));
#33015=CARTESIAN_POINT('Ctrl Pts',(3.32853559102356,1.12709311608126,-28.));
#33016=CARTESIAN_POINT('Ctrl Pts',(3.33540186900274,1.11155835104982,-28.));
#33017=CARTESIAN_POINT('Ctrl Pts',(3.38154819417809,1.00715355986056,-28.));
#33018=CARTESIAN_POINT('Ctrl Pts',(3.42271638561207,0.900775643276435,-28.));
#33019=CARTESIAN_POINT('Ctrl Pts',(3.45888174339864,0.79286061108879,-28.));
#33020=CARTESIAN_POINT('Ctrl Pts',(3.49551139265451,0.683560163909538,-28.));
#33021=CARTESIAN_POINT('Ctrl Pts',(3.52700936086568,0.572682160975876,-28.));
#33022=CARTESIAN_POINT('Ctrl Pts',(3.55331100085337,0.460641756070989,-28.));
#33023=CARTESIAN_POINT('Ctrl Pts',(3.57965805345284,0.348407901350266,-28.));
#33024=CARTESIAN_POINT('Ctrl Pts',(3.60079119852265,0.235006803316379,-28.));
#33025=CARTESIAN_POINT('Ctrl Pts',(3.61660057879941,0.12082976881976,-28.));
#33026=CARTESIAN_POINT('Ctrl Pts',(3.62981203276487,0.0254152358805882,
-28.));
#33027=CARTESIAN_POINT('Ctrl Pts',(3.63930497467244,-0.0705418771992364,
-28.));
#33028=CARTESIAN_POINT('Ctrl Pts',(3.64498836398506,-0.166820713555591,
-28.));
#33029=CARTESIAN_POINT('Ctrl Pts',(3.6461235777139,-0.186051677830032,-28.));
#33030=CARTESIAN_POINT('Ctrl Pts',(3.6471067185271,-0.20529548900737,-28.));
#33031=CARTESIAN_POINT('Ctrl Pts',(3.64793693432402,-0.224550399084413,
-28.));
#33032=CARTESIAN_POINT('Ctrl Pts',(3.64860254404802,-0.23998765699922,-28.));
#33033=CARTESIAN_POINT('Ctrl Pts',(3.64916964547777,-0.255427938226552,
-28.));
#33034=CARTESIAN_POINT('Ctrl Pts',(3.64963779664493,-0.270862333203369,
-28.));
#33035=CARTESIAN_POINT('Ctrl Pts',(3.65323277593957,-0.38938458468805,-28.));
#33036=CARTESIAN_POINT('Ctrl Pts',(3.65100280640831,-0.507698311102713,
-28.));
#33037=CARTESIAN_POINT('Ctrl Pts',(3.64288169923472,-0.625376302714804,
-28.));
#33038=CARTESIAN_POINT('Ctrl Pts',(3.63479002186308,-0.742627845086358,
-28.));
#33039=CARTESIAN_POINT('Ctrl Pts',(3.62085014760366,-0.859249136162332,
-28.));
#33040=CARTESIAN_POINT('Ctrl Pts',(3.60094836490086,-0.974834987561213,
-28.));
#33041=CARTESIAN_POINT('Ctrl Pts',(3.59783401431466,-0.992922556370264,
-28.));
#33042=CARTESIAN_POINT('Ctrl Pts',(3.59457356725438,-1.01098478869548,-28.));
#33043=CARTESIAN_POINT('Ctrl Pts',(3.59116647252837,-1.02902014863058,-28.));
#33044=CARTESIAN_POINT('Ctrl Pts',(3.5698067929562,-1.14208701062335,-28.));
#33045=CARTESIAN_POINT('Ctrl Pts',(3.54268787530998,-1.25409799710567,-28.));
#33046=CARTESIAN_POINT('Ctrl Pts',(3.51011097433732,-1.36479007515236,-28.));
#33047=CARTESIAN_POINT('Ctrl Pts',(3.48961584669467,-1.43442985674183,-28.));
#33048=CARTESIAN_POINT('Ctrl Pts',(3.46695931768047,-1.50354758632599,-28.));
#33049=CARTESIAN_POINT('Ctrl Pts',(3.44220601927238,-1.57207614745179,-28.));
#33050=CARTESIAN_POINT('Ctrl Pts',(3.43518503142662,-1.59151348411776,-28.));
#33051=CARTESIAN_POINT('Ctrl Pts',(3.42799530994855,-1.61090340968787,-28.));
#33052=CARTESIAN_POINT('Ctrl Pts',(3.42063822020598,-1.63024436076578,-28.));
#33053=CARTESIAN_POINT('Ctrl Pts',(3.41481803847106,-1.64554495572091,-28.));
#33054=CARTESIAN_POINT('Ctrl Pts',(3.40889428943117,-1.6608116772918,-28.));
#33055=CARTESIAN_POINT('Ctrl Pts',(3.40287157324905,-1.67603450368239,-28.));
#33056=CARTESIAN_POINT('Ctrl Pts',(3.35899814626558,-1.7869275861277,-28.));
#33057=CARTESIAN_POINT('Ctrl Pts',(3.30982303933651,-1.89563557342822,-28.));
#33058=CARTESIAN_POINT('Ctrl Pts',(3.25572869869663,-2.0018849375163,-28.));
#33059=CARTESIAN_POINT('Ctrl Pts',(3.20129011712566,-2.10881044220593,-28.));
#33060=CARTESIAN_POINT('Ctrl Pts',(3.1418691079394,-2.21324660722471,-28.));
#33061=CARTESIAN_POINT('Ctrl Pts',(3.07779972161007,-2.31491110313074,-28.));
#33062=CARTESIAN_POINT('Ctrl Pts',(3.01270127986138,-2.41820849122544,-28.));
#33063=CARTESIAN_POINT('Ctrl Pts',(2.94280360348117,-2.51864522862981,-28.));
#33064=CARTESIAN_POINT('Ctrl Pts',(2.86840510375314,-2.61591053169999,-28.));
#33065=CARTESIAN_POINT('Ctrl Pts',(2.79774779990573,-2.70828476099175,-28.));
#33066=CARTESIAN_POINT('Ctrl Pts',(2.72303020373738,-2.79779894671307,-28.));
#33067=CARTESIAN_POINT('Ctrl Pts',(2.64447016582119,-2.88416524587393,-28.));
#33068=CARTESIAN_POINT('Ctrl Pts',(2.63081639884696,-2.89917574427043,-28.));
#33069=CARTESIAN_POINT('Ctrl Pts',(2.6170454616123,-2.91409207965698,-28.));
#33070=CARTESIAN_POINT('Ctrl Pts',(2.60317113657109,-2.92889936528399,-28.));
#33071=CARTESIAN_POINT('Ctrl Pts',(2.51751513814057,-3.02031518772295,-28.));
#33072=CARTESIAN_POINT('Ctrl Pts',(2.42781771358721,-3.10769309042211,-28.));
#33073=CARTESIAN_POINT('Ctrl Pts',(2.33441120260619,-3.19071846015963,-28.));
#33074=CARTESIAN_POINT('Ctrl Pts',(2.24083730371898,-3.27389261441609,-28.));
#33075=CARTESIAN_POINT('Ctrl Pts',(2.14354049917036,-3.35269940049145,-28.));
#33076=CARTESIAN_POINT('Ctrl Pts',(2.04281067096056,-3.42679563159201,-28.));
#33077=CARTESIAN_POINT('Ctrl Pts',(2.01620424429062,-3.44636715250426,-28.));
#33078=CARTESIAN_POINT('Ctrl Pts',(1.98935808664189,-3.46560984606407,-28.));
#33079=CARTESIAN_POINT('Ctrl Pts',(1.96227709625951,-3.4845169684059,-28.));
#33080=CARTESIAN_POINT('Ctrl Pts',(1.94383437408304,-3.49739311508973,-28.));
#33081=CARTESIAN_POINT('Ctrl Pts',(1.92528081035815,-3.51011491576498,-28.));
#33082=CARTESIAN_POINT('Ctrl Pts',(1.90662413024797,-3.52267600831012,-28.));
#33083=CARTESIAN_POINT('Ctrl Pts',(1.79806977795192,-3.59576303436816,-28.));
#33084=CARTESIAN_POINT('Ctrl Pts',(1.68620253668162,-3.66329638779482,-28.));
#33085=CARTESIAN_POINT('Ctrl Pts',(1.57136880162434,-3.72490971212853,-28.));
#33086=CARTESIAN_POINT('Ctrl Pts',(1.45653506656706,-3.78652303646223,-28.));
#33087=CARTESIAN_POINT('Ctrl Pts',(1.33873418968137,-3.84221725159107,-28.));
#33088=CARTESIAN_POINT('Ctrl Pts',(1.21827111413391,-3.89158314773214,-28.));
#33089=CARTESIAN_POINT('Ctrl Pts',(1.166391910295,-3.91284330049641,-28.));
#33090=CARTESIAN_POINT('Ctrl Pts',(1.11401847832268,-3.93292910513849,-28.));
#33091=CARTESIAN_POINT('Ctrl Pts',(1.06118740155668,-3.95185074745288,-28.));
#33092=CARTESIAN_POINT('Ctrl Pts',(-1.05882113085931,-3.94905752896967,
-28.0020436944626));
#33093=CARTESIAN_POINT('Ctrl Pts',(-2.35950680140507,-3.60031774422942,
-28.0675689977652));
#33094=CARTESIAN_POINT('Ctrl Pts',(-4.5680262281043,-1.52377528117773,-28.1986196043704));
#33095=CARTESIAN_POINT('Ctrl Pts',(-3.78535991995299,2.98379941052452,-28.3951955142783));
#33096=CARTESIAN_POINT('Ctrl Pts',(0.408199144658901,4.79866122549394,-28.5917714241861));
#33097=CARTESIAN_POINT('Ctrl Pts',(4.23151248292971,2.30176772412023,-28.7883473340939));
#33098=CARTESIAN_POINT('Ctrl Pts',(4.25039471757788,-2.26763872001778,-28.9849232440017));
#33099=CARTESIAN_POINT('Ctrl Pts',(0.445491442266795,-4.79631292568449,
-29.1814991539096));
#33100=CARTESIAN_POINT('Ctrl Pts',(-3.75969845785261,-3.01155046772413,
-29.3780750638174));
#33101=CARTESIAN_POINT('Ctrl Pts',(-4.58346317448722,1.48221938381933,-29.5746509737252));
#33102=CARTESIAN_POINT('Ctrl Pts',(-1.28456058010556,4.64266995936712,-29.7712268836331));
#33103=CARTESIAN_POINT('Ctrl Pts',(3.16967659691989,3.62738124137317,-29.9678027935409));
#33104=CARTESIAN_POINT('Ctrl Pts',(4.7729992922858,-0.650566816687759,-30.1643787034487));
#33105=CARTESIAN_POINT('Ctrl Pts',(2.08326953584618,-4.34334784652524,-30.3609546133566));
#33106=CARTESIAN_POINT('Ctrl Pts',(-2.48023430202747,-4.12954713239435,
-30.5575305232643));
#33107=CARTESIAN_POINT('Ctrl Pts',(-4.81291358150149,-0.201451079063452,
-30.7541064331722));
#33108=CARTESIAN_POINT('Ctrl Pts',(-2.81665191682384,3.90783605333626,-30.9506823430801));
#33109=CARTESIAN_POINT('Ctrl Pts',(1.71302529420149,4.50225061230501,-31.1472582529878));
#33110=CARTESIAN_POINT('Ctrl Pts',(4.70193520370772,1.04714888338313,-31.3438341628957));
#33111=CARTESIAN_POINT('Ctrl Pts',(3.46172444128033,-3.34980272978597,-31.5404100728035));
#33112=CARTESIAN_POINT('Ctrl Pts',(-0.892108337079269,-4.73379952267849,
-31.7369859827114));
#33113=CARTESIAN_POINT('Ctrl Pts',(-4.44354101170039,-1.86001567550251,
-31.9335618926191));
#33114=CARTESIAN_POINT('Ctrl Pts',(-3.99826394800999,2.68674530490854,-32.1301378025271));
#33115=CARTESIAN_POINT('Ctrl Pts',(0.043221683045428,4.81693335226694,-32.3267137124348));
#33116=CARTESIAN_POINT('Ctrl Pts',(4.04583190312332,2.6145667356681,-32.5232896223427));
#33117=CARTESIAN_POINT('Ctrl Pts',(4.4094488939688,-1.93945235711869,-32.7198655322504));
#33118=CARTESIAN_POINT('Ctrl Pts',(0.807020081006245,-4.74904554580652,
-32.9164414421584));
#33119=CARTESIAN_POINT('Ctrl Pts',(-3.52127690491969,-3.28714526013178,
-33.1130173520661));
#33120=CARTESIAN_POINT('Ctrl Pts',(-4.68238773251868,1.13135322695175,-33.309593261974));
#33121=CARTESIAN_POINT('Ctrl Pts',(-1.63195995882842,4.53226452184925,-33.5061691718818));
#33122=CARTESIAN_POINT('Ctrl Pts',(2.8863219858102,3.85666441328645,-33.7027450817896));
#33123=CARTESIAN_POINT('Ctrl Pts',(4.80852322250443,-0.287783637249186,
-33.8993209916975));
#33124=CARTESIAN_POINT('Ctrl Pts',(2.40573423502515,-4.17338684909552,-34.0958969016053));
#33125=CARTESIAN_POINT('Ctrl Pts',(-2.16087440442547,-4.30526849460362,
-34.2924728115131));
#33126=CARTESIAN_POINT('Ctrl Pts',(-4.78390073438757,-0.564808614327262,
-34.4890487214209));
#33127=CARTESIAN_POINT('Ctrl Pts',(-3.10408335123885,3.68366414628393,-34.6856246313288));
#33128=CARTESIAN_POINT('Ctrl Pts',(1.36767856671707,4.61889276144569,-34.8822005412366));
#33129=CARTESIAN_POINT('Ctrl Pts',(4.60929224090002,1.39969284918004,-35.0787764511445));
#33130=CARTESIAN_POINT('Ctrl Pts',(3.70511249281298,-3.07845031582542,-35.2753523610522));
#33131=CARTESIAN_POINT('Ctrl Pts',(-0.531602930013868,-4.78770439360861,
-35.4719282709601));
#33132=CARTESIAN_POINT('Ctrl Pts',(-4.29017212852273,-2.19069356908814,
-35.6685041808679));
#33133=CARTESIAN_POINT('Ctrl Pts',(-4.1899780121579,2.3767201546401,-35.8650800907758));
#33134=CARTESIAN_POINT('Ctrl Pts',(-0.32113973386512,4.8064107934268,-36.0616560006836));
#33135=CARTESIAN_POINT('Ctrl Pts',(3.83654567111785,2.91301107927893,-36.2582319105914));
#33136=CARTESIAN_POINT('Ctrl Pts',(4.54347800750842,-1.60047437829833,-36.4548078204993));
#33137=CARTESIAN_POINT('Ctrl Pts',(1.16381458360049,-4.67442566474814,-36.6513837304071));
#33138=CARTESIAN_POINT('Ctrl Pts',(-3.2626361586303,-3.54399873137932,-36.8479596403149));
#33139=CARTESIAN_POINT('Ctrl Pts',(-4.75452733360971,0.774049293558451,
-37.0445355502227));
#33140=CARTESIAN_POINT('Ctrl Pts',(-1.97000605283459,4.39588848572516,-37.2411114601306));
#33141=CARTESIAN_POINT('Ctrl Pts',(2.58644514433784,4.0638708043759,-37.4376873700384));
#33142=CARTESIAN_POINT('Ctrl Pts',(4.81649301369077,0.0766504053415182,
-37.6342632799463));
#33143=CARTESIAN_POINT('Ctrl Pts',(2.71446985731166,-3.9795429847404,-37.830839189854));
#33144=CARTESIAN_POINT('Ctrl Pts',(-1.82923482333114,-4.45630661812464,
-38.0274150997619));
#33145=CARTESIAN_POINT('Ctrl Pts',(-4.72731037414528,-0.924995639297582,
-38.2239910096697));
#33146=CARTESIAN_POINT('Ctrl Pts',(-3.37410476784824,3.43852550307855,-38.4205669195776));
#33147=CARTESIAN_POINT('Ctrl Pts',(1.01521569000634,4.70883952282901,-38.6171428294853));
#33148=CARTESIAN_POINT('Ctrl Pts',(4.48884927255114,1.74470865965533,-38.8137187393932));
#33149=CARTESIAN_POINT('Ctrl Pts',(3.93008090951081,-2.7904251809593,-39.010294649301));
#33150=CARTESIAN_POINT('Ctrl Pts',(-0.174843701399625,-4.81279159986601,
-39.2069155208212));
#33151=CARTESIAN_POINT('Ctrl Pts',(-2.79071673421448,-3.27789123761485,
-39.3380110890387));
#33152=CARTESIAN_POINT('Ctrl Pts',(-3.49170722037164,-2.12700203220468,
-39.4035813539536));
#33153=CARTESIAN_POINT('Ctrl Pts',(-0.997991714641228,-3.72218364338343,
-27.8664315295235));
#33154=CARTESIAN_POINT('Ctrl Pts',(-2.22395281866996,-3.3934790061289,-27.9319568328261));
#33155=CARTESIAN_POINT('Ctrl Pts',(-4.30559250759574,-1.43623418655831,
-28.0630074394313));
#33156=CARTESIAN_POINT('Ctrl Pts',(-3.56789048399717,2.81237973352319,-28.2595833493392));
#33157=CARTESIAN_POINT('Ctrl Pts',(0.384748048957611,4.52297749340006,-28.456159259247));
#33158=CARTESIAN_POINT('Ctrl Pts',(3.98841152229129,2.16953085913224,-28.6527351691548));
#33159=CARTESIAN_POINT('Ctrl Pts',(4.00620897002213,-2.13736257090065,-28.8493110790626));
#33160=CARTESIAN_POINT('Ctrl Pts',(0.419897899057805,-4.52076410373015,
-29.0458869889705));
#33161=CARTESIAN_POINT('Ctrl Pts',(-3.54370327634202,-2.8385364887584,-29.2424628988783));
#33162=CARTESIAN_POINT('Ctrl Pts',(-4.32014259933502,1.39706568108611,-29.4390388087861));
#33163=CARTESIAN_POINT('Ctrl Pts',(-1.21076240220069,4.37594794646929,-29.635614718694));
#33164=CARTESIAN_POINT('Ctrl Pts',(2.98757825058798,3.41898770172583,-29.8321906286018));
#33165=CARTESIAN_POINT('Ctrl Pts',(4.49878984170234,-0.613191665666869,
-30.0287665385096));
#33166=CARTESIAN_POINT('Ctrl Pts',(1.96358542112927,-4.09382192922343,-30.2253424484175));
#33167=CARTESIAN_POINT('Ctrl Pts',(-2.33774450816214,-3.892304094843,-30.4219183583252));
#33168=CARTESIAN_POINT('Ctrl Pts',(-4.53641104964019,-0.189877687506765,
-30.6184942682331));
#33169=CARTESIAN_POINT('Ctrl Pts',(-2.6548348857915,3.68333034706318,-30.8150701781409));
#33170=CARTESIAN_POINT('Ctrl Pts',(1.61461176090855,4.24359570976092,-31.0116460880488));
#33171=CARTESIAN_POINT('Ctrl Pts',(4.43180839456038,0.986990039350689,-31.2082219979566));
#33172=CARTESIAN_POINT('Ctrl Pts',(3.26284790705395,-3.15735611292137,-31.4047979078644));
#33173=CARTESIAN_POINT('Ctrl Pts',(-0.840856593261335,-4.46184210412537,
-31.6013738177723));
#33174=CARTESIAN_POINT('Ctrl Pts',(-4.18825898359853,-1.753157525056,-31.7979497276801));
#33175=CARTESIAN_POINT('Ctrl Pts',(-3.76856314703911,2.53239142618341,-31.9945256375879));
#33176=CARTESIAN_POINT('Ctrl Pts',(0.0407385915477348,4.54019988403512,
-32.1911015474957));
#33177=CARTESIAN_POINT('Ctrl Pts',(3.81339831674055,2.46435952544285,-32.3876774574036));
#33178=CARTESIAN_POINT('Ctrl Pts',(4.15612546261083,-1.82803055864119,-32.5842533673114));
#33179=CARTESIAN_POINT('Ctrl Pts',(0.760656668931118,-4.47621224117645,
-32.7808292772193));
#33180=CARTESIAN_POINT('Ctrl Pts',(-3.31897907365649,-3.0982983233167,-32.977405187127));
#33181=CARTESIAN_POINT('Ctrl Pts',(-4.41338392821731,1.06635683206863,-33.1739810970349));
#33182=CARTESIAN_POINT('Ctrl Pts',(-1.53820363994361,4.27188531616954,-33.3705570069427));
#33183=CARTESIAN_POINT('Ctrl Pts',(2.72050239995459,3.63509852460902,-33.5671329168505));
#33184=CARTESIAN_POINT('Ctrl Pts',(4.53227291735735,-0.27125042862614,-33.7637088267584));
#33185=CARTESIAN_POINT('Ctrl Pts',(2.26752448001801,-3.93362521392992,-33.9602847366662));
#33186=CARTESIAN_POINT('Ctrl Pts',(-2.03673187958264,-4.05793024118558,
-34.156860646574));
#33187=CARTESIAN_POINT('Ctrl Pts',(-4.50906499449078,-0.532360283553406,
-34.3534365564819));
#33188=CARTESIAN_POINT('Ctrl Pts',(-2.92575334568362,3.472037146188,-34.5500124663897));
#33189=CARTESIAN_POINT('Ctrl Pts',(1.28910524931466,4.35353675176285,-34.7465883762975));
#33190=CARTESIAN_POINT('Ctrl Pts',(4.34448778241235,1.31928030694909,-34.9431642862054));
#33191=CARTESIAN_POINT('Ctrl Pts',(3.49225328232741,-2.90159293159843,-35.1397401961131));
#33192=CARTESIAN_POINT('Ctrl Pts',(-0.501062270264922,-4.51265013297856,
-35.336316106021));
#33193=CARTESIAN_POINT('Ctrl Pts',(-4.0437011633642,-2.0648379292293,-35.5328920159288));
#33194=CARTESIAN_POINT('Ctrl Pts',(-3.94926321244538,2.24017726244907,-35.7294679258367));
#33195=CARTESIAN_POINT('Ctrl Pts',(-0.302690213010174,4.53028184761403,
-35.9260438357445));
#33196=CARTESIAN_POINT('Ctrl Pts',(3.61613560688092,2.74565820141793,-36.1226197456523));
#33197=CARTESIAN_POINT('Ctrl Pts',(4.28245458557109,-1.50852691024499,-36.3191956555602));
#33198=CARTESIAN_POINT('Ctrl Pts',(1.09695327941679,-4.40587928230987,-36.515771565468));
#33199=CARTESIAN_POINT('Ctrl Pts',(-3.07519727298922,-3.34039552813339,
-36.7123474753758));
#33200=CARTESIAN_POINT('Ctrl Pts',(-4.48137909953387,0.729580057651749,
-36.9089233852837));
#33201=CARTESIAN_POINT('Ctrl Pts',(-1.8568289404334,4.1433441016426,-37.1054992951915));
#33202=CARTESIAN_POINT('Ctrl Pts',(2.4378535233126,3.83040088069267,-37.3020752050993));
#33203=CARTESIAN_POINT('Ctrl Pts',(4.53978484296931,0.0722468292568363,
-37.4986511150071));
#33204=CARTESIAN_POINT('Ctrl Pts',(2.55852319932624,-3.75091770562448,-37.695227024915));
#33205=CARTESIAN_POINT('Ctrl Pts',(-1.72414503697722,-4.20029120421869,
-37.8918029348228));
#33206=CARTESIAN_POINT('Ctrl Pts',(-4.4557257580472,-0.871854515548868,
-38.0883788447306));
#33207=CARTESIAN_POINT('Ctrl Pts',(-3.18026199563204,3.24098175096857,-38.2849547546384));
#33208=CARTESIAN_POINT('Ctrl Pts',(0.956891412223545,4.43831605962057,-38.4815306645463));
#33209=CARTESIAN_POINT('Ctrl Pts',(4.23096427877636,1.64447491276048,-38.6781065744541));
#33210=CARTESIAN_POINT('Ctrl Pts',(3.70429723326195,-2.63011487942588,-38.8746824843619));
#33211=CARTESIAN_POINT('Ctrl Pts',(-0.164798907264359,-4.53629607586606,
-39.0713033558821));
#33212=CARTESIAN_POINT('Ctrl Pts',(-2.63038968290739,-3.08957594563662,
-39.2023989240996));
#33213=CARTESIAN_POINT('Ctrl Pts',(-3.29110817145834,-2.00480547969662,
-39.2679691890145));
#33214=CARTESIAN_POINT('Ctrl Pts',(-0.937162298423141,-3.49530975779719,
-27.7308193645844));
#33215=CARTESIAN_POINT('Ctrl Pts',(-2.08839883593485,-3.18664026802839,
-27.796344667887));
#33216=CARTESIAN_POINT('Ctrl Pts',(-4.04315878708718,-1.34869309193889,
-27.9273952744922));
#33217=CARTESIAN_POINT('Ctrl Pts',(-3.35042104804134,2.64096005652187,-28.1239711844001));
#33218=CARTESIAN_POINT('Ctrl Pts',(0.361296953256328,4.24729376130616,-28.3205470943079));
#33219=CARTESIAN_POINT('Ctrl Pts',(3.74531056165287,2.03729399414426,-28.5171230042157));
#33220=CARTESIAN_POINT('Ctrl Pts',(3.76202322246639,-2.0070864217835,-28.7136989141235));
#33221=CARTESIAN_POINT('Ctrl Pts',(0.39430435584881,-4.2452152817758,-28.9102748240314));
#33222=CARTESIAN_POINT('Ctrl Pts',(-3.32770809483142,-2.66552250979267,
-29.1068507339392));
#33223=CARTESIAN_POINT('Ctrl Pts',(-4.05682202418285,1.31191197835287,-29.303426643847));
#33224=CARTESIAN_POINT('Ctrl Pts',(-1.13696422429583,4.10922593357146,-29.5000025537548));
#33225=CARTESIAN_POINT('Ctrl Pts',(2.80547990425606,3.2105941620785,-29.6965784636627));
#33226=CARTESIAN_POINT('Ctrl Pts',(4.22458039111889,-0.575816514645981,
-29.8931543735705));
#33227=CARTESIAN_POINT('Ctrl Pts',(1.84390130641238,-3.84429601192161,-30.0897302834784));
#33228=CARTESIAN_POINT('Ctrl Pts',(-2.1952547142968,-3.65506105729165,-30.2863061933862));
#33229=CARTESIAN_POINT('Ctrl Pts',(-4.2599085177789,-0.178304295950073,
-30.482882103294));
#33230=CARTESIAN_POINT('Ctrl Pts',(-2.49301785475917,3.4588246407901,-30.6794580132018));
#33231=CARTESIAN_POINT('Ctrl Pts',(1.51619822761561,3.98494080721683,-30.8760339231097));
#33232=CARTESIAN_POINT('Ctrl Pts',(4.16168158541303,0.926831195318249,-31.0726098330175));
#33233=CARTESIAN_POINT('Ctrl Pts',(3.06397137282756,-2.96490949605675,-31.2691857429253));
#33234=CARTESIAN_POINT('Ctrl Pts',(-0.789604849443395,-4.18988468557226,
-31.4657616528332));
#33235=CARTESIAN_POINT('Ctrl Pts',(-3.93297695549669,-1.6462993746095,-31.662337562741));
#33236=CARTESIAN_POINT('Ctrl Pts',(-3.53886234606824,2.37803754745827,-31.8589134726488));
#33237=CARTESIAN_POINT('Ctrl Pts',(0.0382555000500392,4.26346641580331,
-32.0554893825566));
#33238=CARTESIAN_POINT('Ctrl Pts',(3.58096473035777,2.3141523152176,-32.2520652924645));
#33239=CARTESIAN_POINT('Ctrl Pts',(3.90280203125285,-1.71660876016369,-32.4486412023723));
#33240=CARTESIAN_POINT('Ctrl Pts',(0.714293256855994,-4.20337893654636,
-32.6452171122801));
#33241=CARTESIAN_POINT('Ctrl Pts',(-3.11668124239328,-2.90945138650161,
-32.8417930221879));
#33242=CARTESIAN_POINT('Ctrl Pts',(-4.14438012391592,1.00136043718551,-33.0383689320958));
#33243=CARTESIAN_POINT('Ctrl Pts',(-1.44444732105879,4.01150611048984,-33.2349448420036));
#33244=CARTESIAN_POINT('Ctrl Pts',(2.55468281409898,3.4135326359316,-33.4315207519115));
#33245=CARTESIAN_POINT('Ctrl Pts',(4.25602261221028,-0.254717220003096,
-33.6280966618193));
#33246=CARTESIAN_POINT('Ctrl Pts',(2.12931472501088,-3.69386357876432,-33.8246725717271));
#33247=CARTESIAN_POINT('Ctrl Pts',(-1.91258935473982,-3.81059198776754,
-34.0212484816349));
#33248=CARTESIAN_POINT('Ctrl Pts',(-4.23422925459399,-0.499911952779544,
-34.2178243915428));
#33249=CARTESIAN_POINT('Ctrl Pts',(-2.74742334012838,3.26041014609205,-34.4144003014506));
#33250=CARTESIAN_POINT('Ctrl Pts',(1.21053193191224,4.08818074208003,-34.6109762113584));
#33251=CARTESIAN_POINT('Ctrl Pts',(4.07968332392467,1.23886776471814,-34.8075521212663));
#33252=CARTESIAN_POINT('Ctrl Pts',(3.27939407184185,-2.72473554737144,-35.0041280311741));
#33253=CARTESIAN_POINT('Ctrl Pts',(-0.470521610515976,-4.23759587234851,
-35.2007039410819));
#33254=CARTESIAN_POINT('Ctrl Pts',(-3.79723019820567,-1.93898228937048,
-35.3972798509897));
#33255=CARTESIAN_POINT('Ctrl Pts',(-3.70854841273286,2.10363437025803,-35.5938557608975));
#33256=CARTESIAN_POINT('Ctrl Pts',(-0.284240692155229,4.25415290180127,
-35.7904316708054));
#33257=CARTESIAN_POINT('Ctrl Pts',(3.39572554264398,2.57830532355692,-35.9870075807132));
#33258=CARTESIAN_POINT('Ctrl Pts',(4.02143116363375,-1.41657944219165,-36.1835834906211));
#33259=CARTESIAN_POINT('Ctrl Pts',(1.03009197523309,-4.13733289987159,-36.3801594005289));
#33260=CARTESIAN_POINT('Ctrl Pts',(-2.88775838734814,-3.13679232488744,
-36.5767353104367));
#33261=CARTESIAN_POINT('Ctrl Pts',(-4.20823086545802,0.685110821745049,
-36.7733112203445));
#33262=CARTESIAN_POINT('Ctrl Pts',(-1.74365182803221,3.89079971756003,-36.9698871302524));
#33263=CARTESIAN_POINT('Ctrl Pts',(2.28926190228734,3.59693095700945,-37.1664630401602));
#33264=CARTESIAN_POINT('Ctrl Pts',(4.26307667224786,0.0678432531721597,
-37.363038950068));
#33265=CARTESIAN_POINT('Ctrl Pts',(2.40257654134081,-3.52229242650857,-37.5596148599759));
#33266=CARTESIAN_POINT('Ctrl Pts',(-1.61905525062328,-3.94427579031274,
-37.7561907698837));
#33267=CARTESIAN_POINT('Ctrl Pts',(-4.18414114194912,-0.818713391800153,
-37.9527666797915));
#33268=CARTESIAN_POINT('Ctrl Pts',(-2.98641922341583,3.0434379988586,-38.1493425896994));
#33269=CARTESIAN_POINT('Ctrl Pts',(0.898567134440758,4.16779259641213,-38.3459184996071));
#33270=CARTESIAN_POINT('Ctrl Pts',(3.97307928500157,1.54424116586562,-38.542494409515));
#33271=CARTESIAN_POINT('Ctrl Pts',(3.47851355701309,-2.46980457789247,-38.7390703194228));
#33272=CARTESIAN_POINT('Ctrl Pts',(-0.154754113129096,-4.25980055186612,
-38.935691190943));
#33273=CARTESIAN_POINT('Ctrl Pts',(-2.47006263160031,-2.90126065365839,
-39.0667867591605));
#33274=CARTESIAN_POINT('Ctrl Pts',(-3.09050912254503,-1.88260892718855,
-39.1323570240753));
#33275=CARTESIAN_POINT('Ctrl Pts',(-0.876332882205054,-3.26843587221096,
-27.5952071996452));
#33276=CARTESIAN_POINT('Ctrl Pts',(-1.95284485319974,-2.97980152992788,
-27.6607325029478));
#33277=CARTESIAN_POINT('Ctrl Pts',(-3.78072506657861,-1.26115199731948,
-27.791783109553));
#33278=CARTESIAN_POINT('Ctrl Pts',(-3.13295161208552,2.46954037952055,-27.9883590194609));
#33279=CARTESIAN_POINT('Ctrl Pts',(0.337845857555048,3.97161002921227,-28.1849349293687));
#33280=CARTESIAN_POINT('Ctrl Pts',(3.50220960101444,1.90505712915628,-28.3815108392765));
#33281=CARTESIAN_POINT('Ctrl Pts',(3.51783747491063,-1.87681027266635,-28.5780867491843));
#33282=CARTESIAN_POINT('Ctrl Pts',(0.368710812639818,-3.96966645982145,
-28.7746626590923));
#33283=CARTESIAN_POINT('Ctrl Pts',(-3.11171291332083,-2.49250853082694,
-28.971238569));
#33284=CARTESIAN_POINT('Ctrl Pts',(-3.79350144903066,1.22675827561963,-29.1678144789079));
#33285=CARTESIAN_POINT('Ctrl Pts',(-1.06316604639096,3.84250392067363,-29.3643903888156));
#33286=CARTESIAN_POINT('Ctrl Pts',(2.62338155792415,3.00220062243116,-29.5609662987235));
#33287=CARTESIAN_POINT('Ctrl Pts',(3.95037094053543,-0.538441363625094,
-29.7575422086313));
#33288=CARTESIAN_POINT('Ctrl Pts',(1.72421719169547,-3.5947700946198,-29.9541181185392));
#33289=CARTESIAN_POINT('Ctrl Pts',(-2.05276492043147,-3.4178180197403,-30.1506940284469));
#33290=CARTESIAN_POINT('Ctrl Pts',(-3.98340598591762,-0.166730904393382,
-30.3472699383548));
#33291=CARTESIAN_POINT('Ctrl Pts',(-2.33120082372684,3.23431893451701,-30.5438458482627));
#33292=CARTESIAN_POINT('Ctrl Pts',(1.41778469432266,3.72628590467274,-30.7404217581705));
#33293=CARTESIAN_POINT('Ctrl Pts',(3.89155477626569,0.866672351285809,-30.9369976680783));
#33294=CARTESIAN_POINT('Ctrl Pts',(2.86509483860116,-2.77246287919215,-31.1335735779861));
#33295=CARTESIAN_POINT('Ctrl Pts',(-0.738353105625458,-3.91792726701915,
-31.3301494878941));
#33296=CARTESIAN_POINT('Ctrl Pts',(-3.67769492739484,-1.53944122416299,
-31.5267253978018));
#33297=CARTESIAN_POINT('Ctrl Pts',(-3.30916154509737,2.22368366873312,-31.7233013077096));
#33298=CARTESIAN_POINT('Ctrl Pts',(0.0357724085523446,3.9867329475715,-31.9198772176174));
#33299=CARTESIAN_POINT('Ctrl Pts',(3.34853114397498,2.16394510499236,-32.1164531275253));
#33300=CARTESIAN_POINT('Ctrl Pts',(3.64947859989488,-1.60518696168619,-32.3130290374331));
#33301=CARTESIAN_POINT('Ctrl Pts',(0.667929844780863,-3.93054563191626,
-32.5096049473409));
#33302=CARTESIAN_POINT('Ctrl Pts',(-2.91438341113007,-2.72060444968652,
-32.7061808572487));
#33303=CARTESIAN_POINT('Ctrl Pts',(-3.87537631961455,0.936364042302392,
-32.9027567671566));
#33304=CARTESIAN_POINT('Ctrl Pts',(-1.35069100217398,3.75112690481014,-33.0993326770644));
#33305=CARTESIAN_POINT('Ctrl Pts',(2.38886322824336,3.19196674725417,-33.2959085869722));
#33306=CARTESIAN_POINT('Ctrl Pts',(3.97977230706319,-0.238184011380052,
-33.4924844968801));
#33307=CARTESIAN_POINT('Ctrl Pts',(1.99110497000374,-3.45410194359872,-33.6890604067879));
#33308=CARTESIAN_POINT('Ctrl Pts',(-1.788446829897,-3.56325373434949,-33.8856363166957));
#33309=CARTESIAN_POINT('Ctrl Pts',(-3.9593935146972,-0.467463622005686,
-34.0822122266036));
#33310=CARTESIAN_POINT('Ctrl Pts',(-2.56909333457314,3.04878314599611,-34.2787881365114));
#33311=CARTESIAN_POINT('Ctrl Pts',(1.13195861450983,3.8228247323972,-34.4753640464193));
#33312=CARTESIAN_POINT('Ctrl Pts',(3.814878865437,1.15845522248718,-34.671939956327));
#33313=CARTESIAN_POINT('Ctrl Pts',(3.06653486135627,-2.54787816314444,-34.8685158662349));
#33314=CARTESIAN_POINT('Ctrl Pts',(-0.439980950767031,-3.96254161171846,
-35.0650917761427));
#33315=CARTESIAN_POINT('Ctrl Pts',(-3.55075923304713,-1.81312664951164,
-35.2616676860505));
#33316=CARTESIAN_POINT('Ctrl Pts',(-3.46783361302034,1.96709147806698,-35.4582435959584));
#33317=CARTESIAN_POINT('Ctrl Pts',(-0.265791171300281,3.9780239559885,-35.6548195058662));
#33318=CARTESIAN_POINT('Ctrl Pts',(3.17531547840704,2.4109524456959,-35.851395415774));
#33319=CARTESIAN_POINT('Ctrl Pts',(3.76040774169642,-1.3246319741383,-36.0479713256819));
#33320=CARTESIAN_POINT('Ctrl Pts',(0.96323067104939,-3.86878651743331,-36.2445472355897));
#33321=CARTESIAN_POINT('Ctrl Pts',(-2.70031950170705,-2.93318912164151,
-36.4411231454975));
#33322=CARTESIAN_POINT('Ctrl Pts',(-3.93508263138217,0.640641585838348,
-36.6376990554053));
#33323=CARTESIAN_POINT('Ctrl Pts',(-1.63047471563101,3.63825533347747,-36.8342749653132));
#33324=CARTESIAN_POINT('Ctrl Pts',(2.14067028126209,3.36346103332622,-37.030850875221));
#33325=CARTESIAN_POINT('Ctrl Pts',(3.98636850152641,0.0634396770874798,
-37.2274267851288));
#33326=CARTESIAN_POINT('Ctrl Pts',(2.24662988335538,-3.29366714739265,-37.4240026950367));
#33327=CARTESIAN_POINT('Ctrl Pts',(-1.51396546426936,-3.68826037640678,
-37.6205786049445));
#33328=CARTESIAN_POINT('Ctrl Pts',(-3.91255652585104,-0.765572268051441,
-37.8171545148523));
#33329=CARTESIAN_POINT('Ctrl Pts',(-2.79257645119962,2.84589424674863,-38.0137304247602));
#33330=CARTESIAN_POINT('Ctrl Pts',(0.840242856657966,3.89726913320368,-38.210306334668));
#33331=CARTESIAN_POINT('Ctrl Pts',(3.71519429122678,1.44400741897077,-38.4068822445758));
#33332=CARTESIAN_POINT('Ctrl Pts',(3.25272988076424,-2.30949427635907,-38.6034581544836));
#33333=CARTESIAN_POINT('Ctrl Pts',(-0.144709318993833,-3.98330502786617,
-38.8000790260038));
#33334=CARTESIAN_POINT('Ctrl Pts',(-2.30973558029321,-2.71294536168015,
-38.9311745942213));
#33335=CARTESIAN_POINT('Ctrl Pts',(-2.88991007363174,-1.7604123746805,-38.9967448591362));
#33336=CARTESIAN_POINT('Ctrl Pts',(-2.89372837779135,-1.76542944862293,
-39.));
#33337=CARTESIAN_POINT('Ctrl Pts',(-2.84709705329411,-1.86283293579633,
-39.));
#33338=CARTESIAN_POINT('Ctrl Pts',(-2.79559872548623,-1.95750971474293,
-39.));
#33339=CARTESIAN_POINT('Ctrl Pts',(-2.73965370343092,-2.04932605347633,
-39.));
#33340=CARTESIAN_POINT('Ctrl Pts',(-2.68326084165469,-2.14187738170485,
-39.));
#33341=CARTESIAN_POINT('Ctrl Pts',(-2.62234937512617,-2.23152278993156,
-39.));
#33342=CARTESIAN_POINT('Ctrl Pts',(-2.55729461435447,-2.31811500318715,
-39.));
#33343=CARTESIAN_POINT('Ctrl Pts',(-2.49061650072561,-2.40686800706172,
-39.));
#33344=CARTESIAN_POINT('Ctrl Pts',(-2.41958537665938,-2.49241416222915,
-39.));
#33345=CARTESIAN_POINT('Ctrl Pts',(-2.34455344889113,-2.57457547121683,
-39.));
#33346=CARTESIAN_POINT('Ctrl Pts',(-2.27491905341145,-2.6508263853723,-39.));
#33347=CARTESIAN_POINT('Ctrl Pts',(-2.20183785832801,-2.72416209662977,
-39.));
#33348=CARTESIAN_POINT('Ctrl Pts',(-2.1255575635722,-2.79441872971172,-39.));
#33349=CARTESIAN_POINT('Ctrl Pts',(-2.1130737496862,-2.80591672843419,-39.));
#33350=CARTESIAN_POINT('Ctrl Pts',(-2.10050290352848,-2.81733335528404,
-39.));
#33351=CARTESIAN_POINT('Ctrl Pts',(-2.08785007700729,-2.82866421622847,
-39.));
#33352=CARTESIAN_POINT('Ctrl Pts',(-2.00281517469671,-2.90481468362719,
-39.));
#33353=CARTESIAN_POINT('Ctrl Pts',(-1.91436539047486,-2.97684040078833,
-39.));
#33354=CARTESIAN_POINT('Ctrl Pts',(-1.82290776635402,-3.04458314589731,
-39.));
#33355=CARTESIAN_POINT('Ctrl Pts',(-1.73027595536054,-3.11319561228746,
-39.));
#33356=CARTESIAN_POINT('Ctrl Pts',(-1.63455802419001,-3.17741505746554,
-39.));
#33357=CARTESIAN_POINT('Ctrl Pts',(-1.53612883601075,-3.23705171222188,
-39.));
#33358=CARTESIAN_POINT('Ctrl Pts',(-1.43752959901041,-3.29679139681137,
-39.));
#33359=CARTESIAN_POINT('Ctrl Pts',(-1.33620906279526,-3.35193305880578,
-39.));
#33360=CARTESIAN_POINT('Ctrl Pts',(-1.23250544109713,-3.40225130016081,
-39.));
#33361=CARTESIAN_POINT('Ctrl Pts',(-1.14584321588747,-3.44430085149816,
-39.));
#33362=CARTESIAN_POINT('Ctrl Pts',(-1.0575158871866,-3.48298155408148,-39.));
#33363=CARTESIAN_POINT('Ctrl Pts',(-0.967705373285046,-3.51813857622562,
-39.));
#33364=CARTESIAN_POINT('Ctrl Pts',(-0.949769817206312,-3.52515958874225,
-39.));
#33365=CARTESIAN_POINT('Ctrl Pts',(-0.931775072721506,-3.53203999475971,
-39.));
#33366=CARTESIAN_POINT('Ctrl Pts',(-0.913722538202823,-3.53877844450556,
-39.));
#33367=CARTESIAN_POINT('Ctrl Pts',(-0.899250411794731,-3.54418043924572,
-39.));
#33368=CARTESIAN_POINT('Ctrl Pts',(-0.884744979028471,-3.54948973453049,
-39.));
#33369=CARTESIAN_POINT('Ctrl Pts',(-0.870214583172694,-3.55470315445478,
-39.));
#33370=CARTESIAN_POINT('Ctrl Pts',(-0.7586042886915,-3.59474826669951,-39.));
#33371=CARTESIAN_POINT('Ctrl Pts',(-0.645392298328396,-3.62918911380257,
-39.));
#33372=CARTESIAN_POINT('Ctrl Pts',(-0.530964467386553,-3.65783073729646,
-39.));
#33373=CARTESIAN_POINT('Ctrl Pts',(-0.416951129848167,-3.68636861186927,
-39.));
#33374=CARTESIAN_POINT('Ctrl Pts',(-0.301730002251125,-3.70914977822842,
-39.));
#33375=CARTESIAN_POINT('Ctrl Pts',(-0.185651311893365,-3.72594088561003,
-39.));
#33376=CARTESIAN_POINT('Ctrl Pts',(-0.16747868702798,-3.72856960664901,
-39.));
#33377=CARTESIAN_POINT('Ctrl Pts',(-0.149284994067021,-3.73105142456686,
-39.));
#33378=CARTESIAN_POINT('Ctrl Pts',(-0.131071525139037,-3.73338533923414,
-39.));
#33379=CARTESIAN_POINT('Ctrl Pts',(-0.0169379366033663,-3.74801067268194,
-39.));
#33380=CARTESIAN_POINT('Ctrl Pts',(0.0979711271621422,-3.75683236794301,
-39.));
#33381=CARTESIAN_POINT('Ctrl Pts',(0.213312418309857,-3.76005565158897,
-39.));
#33382=CARTESIAN_POINT('Ctrl Pts',(0.285877101729696,-3.762083516502,-39.));
#33383=CARTESIAN_POINT('Ctrl Pts',(0.358613183455896,-3.76189444895298,
-39.));
#33384=CARTESIAN_POINT('Ctrl Pts',(0.431436860770681,-3.75952917685634,
-39.));
#33385=CARTESIAN_POINT('Ctrl Pts',(0.452092660752138,-3.75885828808594,
-39.));
#33386=CARTESIAN_POINT('Ctrl Pts',(0.472755511053182,-3.7580122701961,-39.));
#33387=CARTESIAN_POINT('Ctrl Pts',(0.49342350284441,-3.75699193862249,-39.));
#33388=CARTESIAN_POINT('Ctrl Pts',(0.509773936527692,-3.75618475503649,
-39.));
#33389=CARTESIAN_POINT('Ctrl Pts',(0.526124157697629,-3.75526860350868,
-39.));
#33390=CARTESIAN_POINT('Ctrl Pts',(0.542463214077932,-3.75424476214021,
-39.));
#33391=CARTESIAN_POINT('Ctrl Pts',(0.659891007300508,-3.74688647719952,
-39.));
#33392=CARTESIAN_POINT('Ctrl Pts',(0.776890688476788,-3.73396289933532,
-39.));
#33393=CARTESIAN_POINT('Ctrl Pts',(0.893098832740734,-3.71574250047003,
-39.));
#33394=CARTESIAN_POINT('Ctrl Pts',(1.01145043029335,-3.6971860272778,-39.));
#33395=CARTESIAN_POINT('Ctrl Pts',(1.1289817363392,-3.67313548364135,-39.));
#33396=CARTESIAN_POINT('Ctrl Pts',(1.24532264134319,-3.64382098539602,-39.));
#33397=CARTESIAN_POINT('Ctrl Pts',(1.36364893407646,-3.6140062276323,-39.));
#33398=CARTESIAN_POINT('Ctrl Pts',(1.48074468032365,-3.57874624629638,-39.));
#33399=CARTESIAN_POINT('Ctrl Pts',(1.59622282744335,-3.53822926970182,-39.));
#33400=CARTESIAN_POINT('Ctrl Pts',(1.67894642587911,-3.50920464309289,-39.));
#33401=CARTESIAN_POINT('Ctrl Pts',(1.76084001244962,-3.47748115701661,-39.));
#33402=CARTESIAN_POINT('Ctrl Pts',(1.84175830671377,-3.44311185638279,-39.));
#33403=CARTESIAN_POINT('Ctrl Pts',(1.86974700891392,-3.43122391275997,-39.));
#33404=CARTESIAN_POINT('Ctrl Pts',(1.8976189921892,-3.41901931236763,-39.));
#33405=CARTESIAN_POINT('Ctrl Pts',(1.9253681103356,-3.40649989145697,-39.));
#33406=CARTESIAN_POINT('Ctrl Pts',(1.94401447908019,-3.39808730920707,-39.));
#33407=CARTESIAN_POINT('Ctrl Pts',(1.96260673881699,-3.38953185050619,-39.));
#33408=CARTESIAN_POINT('Ctrl Pts',(1.98112608404139,-3.38084219828656,-39.));
#33409=CARTESIAN_POINT('Ctrl Pts',(2.09453669000687,-3.3276276428087,-39.));
#33410=CARTESIAN_POINT('Ctrl Pts',(2.20535587450821,-3.26932167429468,-39.));
#33411=CARTESIAN_POINT('Ctrl Pts',(2.31318172936241,-3.20614314300893,-39.));
#33412=CARTESIAN_POINT('Ctrl Pts',(2.42120078697442,-3.14285140820167,-39.));
#33413=CARTESIAN_POINT('Ctrl Pts',(2.52621667759038,-3.07466938567556,-39.));
#33414=CARTESIAN_POINT('Ctrl Pts',(2.6278134383443,-3.00176671616721,-39.));
#33415=CARTESIAN_POINT('Ctrl Pts',(2.65464889975007,-2.98251042532239,-39.));
#33416=CARTESIAN_POINT('Ctrl Pts',(2.68124570868624,-2.96292452198041,-39.));
#33417=CARTESIAN_POINT('Ctrl Pts',(2.70759593777791,-2.94301158064002,-39.));
#33418=CARTESIAN_POINT('Ctrl Pts',(2.72554097494419,-2.92945046619201,-39.));
#33419=CARTESIAN_POINT('Ctrl Pts',(2.74337347257275,-2.91573623922872,-39.));
#33420=CARTESIAN_POINT('Ctrl Pts',(2.76108499265317,-2.90187428087526,-39.));
#33421=CARTESIAN_POINT('Ctrl Pts',(2.86413983193027,-2.82121819468424,-39.));
#33422=CARTESIAN_POINT('Ctrl Pts',(2.96293657097843,-2.73569517853608,-39.));
#33423=CARTESIAN_POINT('Ctrl Pts',(3.05701974862933,-2.64552146010616,-39.));
#33424=CARTESIAN_POINT('Ctrl Pts',(3.15110292628022,-2.55534774167624,-39.));
#33425=CARTESIAN_POINT('Ctrl Pts',(3.24047361764325,-2.46052298890747,-39.));
#33426=CARTESIAN_POINT('Ctrl Pts',(3.3246484150941,-2.36121076386274,-39.));
#33427=CARTESIAN_POINT('Ctrl Pts',(3.36089955029359,-2.31844046911791,-39.));
#33428=CARTESIAN_POINT('Ctrl Pts',(3.39618654382643,-2.27483723891631,-39.));
#33429=CARTESIAN_POINT('Ctrl Pts',(3.43050777773768,-2.23043901384844,-39.));
#33430=CARTESIAN_POINT('Ctrl Pts',(-1.05790442297294,-3.94563850749841,
-28.));
#33431=CARTESIAN_POINT('Ctrl Pts',(-1.17552092509457,-3.90322260833457,
-28.));
#33432=CARTESIAN_POINT('Ctrl Pts',(-1.29069214983657,-3.85509352261539,
-28.));
#33433=CARTESIAN_POINT('Ctrl Pts',(-1.40318092946675,-3.80162495038346,
-28.));
#33434=CARTESIAN_POINT('Ctrl Pts',(-1.51645569700177,-3.74778277954729,
-28.));
#33435=CARTESIAN_POINT('Ctrl Pts',(-1.62701098511845,-3.68852555691594,
-28.));
#33436=CARTESIAN_POINT('Ctrl Pts',(-1.73457653866827,-3.62418713824119,
-28.));
#33437=CARTESIAN_POINT('Ctrl Pts',(-1.84251278075503,-3.55962699882501,
-28.));
#33438=CARTESIAN_POINT('Ctrl Pts',(-1.94743922183795,-3.4899498717791,-28.));
#33439=CARTESIAN_POINT('Ctrl Pts',(-2.04904592292942,-3.41545575870663,
-28.));
#33440=CARTESIAN_POINT('Ctrl Pts',(-2.11167361902161,-3.36953954822009,
-28.));
#33441=CARTESIAN_POINT('Ctrl Pts',(-2.17303933245443,-3.32179259632812,
-28.));
#33442=CARTESIAN_POINT('Ctrl Pts',(-2.2330620984525,-3.27227990388831,-28.));
#33443=CARTESIAN_POINT('Ctrl Pts',(-2.26769437499633,-3.24371178929892,
-28.));
#33444=CARTESIAN_POINT('Ctrl Pts',(-2.30187944275612,-3.21455577193222,
-28.));
#33445=CARTESIAN_POINT('Ctrl Pts',(-2.33560066189846,-3.18482388432906,
-28.));
#33446=CARTESIAN_POINT('Ctrl Pts',(-2.35176548728777,-3.17057141114382,
-28.));
#33447=CARTESIAN_POINT('Ctrl Pts',(-2.36782485329837,-3.15618556031416,
-28.));
#33448=CARTESIAN_POINT('Ctrl Pts',(-2.38377304232987,-3.14167111942472,
-28.));
#33449=CARTESIAN_POINT('Ctrl Pts',(-2.39929945678807,-3.12754053541714,
-28.));
#33450=CARTESIAN_POINT('Ctrl Pts',(-2.4147144303058,-3.11329357780667,-28.));
#33451=CARTESIAN_POINT('Ctrl Pts',(-2.43001123186977,-3.09893695799548,
-28.));
#33452=CARTESIAN_POINT('Ctrl Pts',(-2.51988581706192,-3.01458630175559,
-28.));
#33453=CARTESIAN_POINT('Ctrl Pts',(-2.60575268760725,-2.9263905122201,-28.));
#33454=CARTESIAN_POINT('Ctrl Pts',(-2.68735143209645,-2.83466145344241,
-28.));
#33455=CARTESIAN_POINT('Ctrl Pts',(-2.76850886109889,-2.74342849855061,
-28.));
#33456=CARTESIAN_POINT('Ctrl Pts',(-2.84544466814443,-2.64869965528777,
-28.));
#33457=CARTESIAN_POINT('Ctrl Pts',(-2.91785977185231,-2.55075381811677,
-28.));
#33458=CARTESIAN_POINT('Ctrl Pts',(-2.98860807815616,-2.45506242592718,
-28.));
#33459=CARTESIAN_POINT('Ctrl Pts',(-3.05504166648732,-2.35629973630334,
-28.));
#33460=CARTESIAN_POINT('Ctrl Pts',(-3.1168354308863,-2.25470965775042,-28.));
#33461=CARTESIAN_POINT('Ctrl Pts',(-3.16443730013298,-2.17645131432253,
-28.));
#33462=CARTESIAN_POINT('Ctrl Pts',(-3.20928496516993,-2.0965147583857,-28.));
#33463=CARTESIAN_POINT('Ctrl Pts',(-3.25120884148141,-2.01500844711875,
-28.));
#33464=CARTESIAN_POINT('Ctrl Pts',(-3.26049991453858,-1.9969452058532,-28.));
#33465=CARTESIAN_POINT('Ctrl Pts',(-3.26964731182438,-1.97880486295949,
-28.));
#33466=CARTESIAN_POINT('Ctrl Pts',(-3.27864905600516,-1.96058859515145,
-28.));
#33467=CARTESIAN_POINT('Ctrl Pts',(-3.28607688065843,-1.94555737004687,
-28.));
#33468=CARTESIAN_POINT('Ctrl Pts',(-3.29340549865561,-1.93047437020423,
-28.));
#33469=CARTESIAN_POINT('Ctrl Pts',(-3.30062766338968,-1.91535349873123,
-28.));
#33470=CARTESIAN_POINT('Ctrl Pts',(-3.35136195689617,-1.80913233656823,
-28.));
#33471=CARTESIAN_POINT('Ctrl Pts',(-3.39692754659769,-1.7008825211242,-28.));
#33472=CARTESIAN_POINT('Ctrl Pts',(-3.43705405523292,-1.59086014700212,
-28.));
#33473=CARTESIAN_POINT('Ctrl Pts',(-3.47636174188234,-1.48308289068189,
-28.));
#33474=CARTESIAN_POINT('Ctrl Pts',(-3.51045028631878,-1.37360404476521,
-28.));
#33475=CARTESIAN_POINT('Ctrl Pts',(-3.53901673706831,-1.26265350321925,
-28.));
#33476=CARTESIAN_POINT('Ctrl Pts',(-3.54583445116938,-1.23617387233156,
-28.));
#33477=CARTESIAN_POINT('Ctrl Pts',(-3.55233739955794,-1.20961038884467,
-28.));
#33478=CARTESIAN_POINT('Ctrl Pts',(-3.55852102006359,-1.18296614385692,
-28.));
#33479=CARTESIAN_POINT('Ctrl Pts',(-3.58533465285514,-1.06743043133119,
-28.));
#33480=CARTESIAN_POINT('Ctrl Pts',(-3.60614802893092,-0.950375395504629,
-28.));
#33481=CARTESIAN_POINT('Ctrl Pts',(-3.62104714913887,-0.832239843135369,
-28.));
#33482=CARTESIAN_POINT('Ctrl Pts',(-3.63268207221584,-0.739986203639362,
-28.));
#33483=CARTESIAN_POINT('Ctrl Pts',(-3.64070921633916,-0.647073564177628,
-28.));
#33484=CARTESIAN_POINT('Ctrl Pts',(-3.64514860307971,-0.553717990972986,
-28.));
#33485=CARTESIAN_POINT('Ctrl Pts',(-3.64592450960589,-0.537401503417666,
-28.));
#33486=CARTESIAN_POINT('Ctrl Pts',(-3.64659030245521,-0.521081374381654,
-28.));
#33487=CARTESIAN_POINT('Ctrl Pts',(-3.64714640790116,-0.504759992890122,
-28.));
#33488=CARTESIAN_POINT('Ctrl Pts',(-3.65110332464657,-0.3886267160034,-28.));
#33489=CARTESIAN_POINT('Ctrl Pts',(-3.64951230537173,-0.272408796396214,
-28.));
#33490=CARTESIAN_POINT('Ctrl Pts',(-3.64251723929508,-0.156512198468872,
-28.));
#33491=CARTESIAN_POINT('Ctrl Pts',(-3.63549581042975,-0.0401788130280003,
-28.));
#33492=CARTESIAN_POINT('Ctrl Pts',(-3.62302921007484,0.0758317450340023,
-28.));
#33493=CARTESIAN_POINT('Ctrl Pts',(-3.60521119974026,0.19109879958983,-28.));
#33494=CARTESIAN_POINT('Ctrl Pts',(-3.58767840055076,0.304520785700679,
-28.));
#33495=CARTESIAN_POINT('Ctrl Pts',(-3.56496370537445,0.417223667382557,
-28.));
#33496=CARTESIAN_POINT('Ctrl Pts',(-3.53711222719414,0.528784290151367,
-28.));
#33497=CARTESIAN_POINT('Ctrl Pts',(-3.51189251588176,0.629803226447788,
-28.));
#33498=CARTESIAN_POINT('Ctrl Pts',(-3.48246023862158,0.729885733889866,
-28.));
#33499=CARTESIAN_POINT('Ctrl Pts',(-3.44882098814669,0.828693432313728,
-28.));
#33500=CARTESIAN_POINT('Ctrl Pts',(-3.4427386179877,0.846559020514666,-28.));
#33501=CARTESIAN_POINT('Ctrl Pts',(-3.43652137213233,0.864374779285486,
-28.));
#33502=CARTESIAN_POINT('Ctrl Pts',(-3.43017104275558,0.882134801923077,
-28.));
#33503=CARTESIAN_POINT('Ctrl Pts',(-3.3919499839386,0.989027976993363,-28.));
#33504=CARTESIAN_POINT('Ctrl Pts',(-3.34889518138372,1.09395211482332,-28.));
#33505=CARTESIAN_POINT('Ctrl Pts',(-3.30106890262405,1.19649560051157,-28.));
#33506=CARTESIAN_POINT('Ctrl Pts',(-3.26179920216696,1.28069307669486,-28.));
#33507=CARTESIAN_POINT('Ctrl Pts',(-3.21931172738894,1.36328529314877,-28.));
#33508=CARTESIAN_POINT('Ctrl Pts',(-3.17362084982711,1.44402623804176,-28.));
#33509=CARTESIAN_POINT('Ctrl Pts',(-3.15207647343335,1.48209758619672,-28.));
#33510=CARTESIAN_POINT('Ctrl Pts',(-3.12981961866877,1.51975706275399,-28.));
#33511=CARTESIAN_POINT('Ctrl Pts',(-3.1068505199988,1.55697730019376,-28.));
#33512=CARTESIAN_POINT('Ctrl Pts',(-3.09148427832198,1.58187750076261,-28.));
#33513=CARTESIAN_POINT('Ctrl Pts',(-3.07579848046801,1.60658184767048,-28.));
#33514=CARTESIAN_POINT('Ctrl Pts',(-3.05981013081646,1.63105693002514,-28.));
#33515=CARTESIAN_POINT('Ctrl Pts',(-3.0009759331342,1.72112074930146,-28.));
#33516=CARTESIAN_POINT('Ctrl Pts',(-2.93799599951988,1.80816816462597,-28.));
#33517=CARTESIAN_POINT('Ctrl Pts',(-2.870903420132,1.8918173136697,-28.));
#33518=CARTESIAN_POINT('Ctrl Pts',(-2.81008529796309,1.96764364516987,-28.));
#33519=CARTESIAN_POINT('Ctrl Pts',(-2.74588720662993,2.04067754747659,-28.));
#33520=CARTESIAN_POINT('Ctrl Pts',(-2.67831174925371,2.11060476373359,-28.));
#33521=CARTESIAN_POINT('Ctrl Pts',(-2.64566301465728,2.14438973853489,-28.));
#33522=CARTESIAN_POINT('Ctrl Pts',(-2.6122255718507,2.17744902968664,-28.));
#33523=CARTESIAN_POINT('Ctrl Pts',(-2.57802990330401,2.20976968150249,-28.));
#33524=CARTESIAN_POINT('Origin',(0.,0.,-28.));
#33525=CARTESIAN_POINT('',(1.38777878078145E-16,-5.,-28.));
#33526=CARTESIAN_POINT('',(1.38777878078145E-16,5.,-28.));
#33527=CARTESIAN_POINT('Origin',(0.,0.,-28.));
#33528=CARTESIAN_POINT('Origin',(0.,0.,-28.));
#33529=CARTESIAN_POINT('Origin',(0.,0.,0.));
#33530=CARTESIAN_POINT('',(-5.,-6.12323399573677E-16,-39.));
#33531=CARTESIAN_POINT('Origin',(0.,0.,-39.));
#33532=CARTESIAN_POINT('',(-5.,3.06161699786838E-16,-31.3571312154738));
#33533=CARTESIAN_POINT('',(-5.,6.12323399573677E-16,0.));
#33534=CARTESIAN_POINT('',(-2.7252308025327,4.19203018511639,-30.8799792272101));
#33535=CARTESIAN_POINT('Ctrl Pts',(-2.7252308025327,4.19203018511639,-30.8799792272101));
#33536=CARTESIAN_POINT('Ctrl Pts',(-2.8912176764087,4.08412243600022,-30.8653304951571));
#33537=CARTESIAN_POINT('Ctrl Pts',(-3.04862894705818,3.96746986254389,-30.8620029267808));
#33538=CARTESIAN_POINT('Ctrl Pts',(-3.74387664835538,3.39066664475822,-30.8821120697405));
#33539=CARTESIAN_POINT('Ctrl Pts',(-4.21066500973337,2.79554609173792,-31.0137757194408));
#33540=CARTESIAN_POINT('Ctrl Pts',(-4.83880724780192,1.45969207554558,-31.2576781989471));
#33541=CARTESIAN_POINT('Ctrl Pts',(-5.,0.716580051177333,-31.3571312154738));
#33542=CARTESIAN_POINT('Ctrl Pts',(-5.,6.93889390390723E-17,-31.3571312154738));
#33543=CARTESIAN_POINT('',(2.72523080253269,4.1920301851164,-30.8799792272101));
#33544=CARTESIAN_POINT('Ctrl Pts',(2.72523080253269,4.1920301851164,-30.8799792272101));
#33545=CARTESIAN_POINT('Ctrl Pts',(2.47095718963917,4.35733297434463,-30.9024194716491));
#33546=CARTESIAN_POINT('Ctrl Pts',(2.1983745065567,4.50125462875715,-30.923256490722));
#33547=CARTESIAN_POINT('Ctrl Pts',(1.29915176153723,4.87407242020745,-30.9789098121903));
#33548=CARTESIAN_POINT('Ctrl Pts',(0.62898575038369,5.,-31.));
#33549=CARTESIAN_POINT('Ctrl Pts',(-0.62898575038369,5.,-31.));
#33550=CARTESIAN_POINT('Ctrl Pts',(-1.29915176153723,4.87407242020745,-30.9789098121903));
#33551=CARTESIAN_POINT('Ctrl Pts',(-2.1983745065567,4.50125462875714,-30.923256490722));
#33552=CARTESIAN_POINT('Ctrl Pts',(-2.47095718963918,4.35733297434463,-30.9024194716491));
#33553=CARTESIAN_POINT('Ctrl Pts',(-2.7252308025327,4.19203018511639,-30.8799792272101));
#33554=CARTESIAN_POINT('',(2.72523080253269,-4.1920301851164,-30.8799792272101));
#33555=CARTESIAN_POINT('Ctrl Pts',(2.72523080253269,-4.1920301851164,-30.8799792272101));
#33556=CARTESIAN_POINT('Ctrl Pts',(2.89121767640869,-4.08412243600022,-30.8653304951571));
#33557=CARTESIAN_POINT('Ctrl Pts',(3.04862894705818,-3.9674698625439,-30.8620029267808));
#33558=CARTESIAN_POINT('Ctrl Pts',(3.74387664835538,-3.39066664475823,-30.8821120697405));
#33559=CARTESIAN_POINT('Ctrl Pts',(4.21066500973337,-2.79554609173792,-31.0137757194408));
#33560=CARTESIAN_POINT('Ctrl Pts',(4.83880724780192,-1.45969207554558,-31.2576781989471));
#33561=CARTESIAN_POINT('Ctrl Pts',(5.,-0.716580051177333,-31.3571312154738));
#33562=CARTESIAN_POINT('Ctrl Pts',(5.,0.716580051177333,-31.3571312154738));
#33563=CARTESIAN_POINT('Ctrl Pts',(4.83880724780192,1.45969207554558,-31.2576781989471));
#33564=CARTESIAN_POINT('Ctrl Pts',(4.21066500973337,2.79554609173792,-31.0137757194408));
#33565=CARTESIAN_POINT('Ctrl Pts',(3.74387664835538,3.39066664475823,-30.8821120697405));
#33566=CARTESIAN_POINT('Ctrl Pts',(3.04862894705818,3.9674698625439,-30.8620029267808));
#33567=CARTESIAN_POINT('Ctrl Pts',(2.89121767640869,4.08412243600022,-30.8653304951571));
#33568=CARTESIAN_POINT('Ctrl Pts',(2.72523080253269,4.1920301851164,-30.8799792272101));
#33569=CARTESIAN_POINT('',(-2.7252308025327,-4.19203018511639,-30.8799792272101));
#33570=CARTESIAN_POINT('Ctrl Pts',(-2.7252308025327,-4.19203018511639,-30.8799792272101));
#33571=CARTESIAN_POINT('Ctrl Pts',(-2.47095718963918,-4.35733297434463,
-30.9024194716491));
#33572=CARTESIAN_POINT('Ctrl Pts',(-2.1983745065567,-4.50125462875714,-30.923256490722));
#33573=CARTESIAN_POINT('Ctrl Pts',(-1.29915176153723,-4.87407242020745,
-30.9789098121903));
#33574=CARTESIAN_POINT('Ctrl Pts',(-0.628985750383691,-5.,-31.));
#33575=CARTESIAN_POINT('Ctrl Pts',(0.628985750383688,-5.,-31.));
#33576=CARTESIAN_POINT('Ctrl Pts',(1.29915176153722,-4.87407242020745,-30.9789098121903));
#33577=CARTESIAN_POINT('Ctrl Pts',(2.1983745065567,-4.50125462875715,-30.923256490722));
#33578=CARTESIAN_POINT('Ctrl Pts',(2.47095718963917,-4.35733297434463,-30.9024194716491));
#33579=CARTESIAN_POINT('Ctrl Pts',(2.72523080253269,-4.1920301851164,-30.8799792272101));
#33580=CARTESIAN_POINT('Ctrl Pts',(-5.,6.93889390390723E-17,-31.3571312154738));
#33581=CARTESIAN_POINT('Ctrl Pts',(-5.,-0.716580051177333,-31.3571312154738));
#33582=CARTESIAN_POINT('Ctrl Pts',(-4.83880724780192,-1.45969207554558,
-31.2576781989471));
#33583=CARTESIAN_POINT('Ctrl Pts',(-4.21066500973337,-2.79554609173792,
-31.0137757194408));
#33584=CARTESIAN_POINT('Ctrl Pts',(-3.74387664835538,-3.39066664475822,
-30.8821120697405));
#33585=CARTESIAN_POINT('Ctrl Pts',(-3.04862894705818,-3.96746986254389,
-30.8620029267808));
#33586=CARTESIAN_POINT('Ctrl Pts',(-2.8912176764087,-4.08412243600022,-30.8653304951571));
#33587=CARTESIAN_POINT('Ctrl Pts',(-2.7252308025327,-4.19203018511639,-30.8799792272101));
#33588=CARTESIAN_POINT('Origin',(0.,0.,-39.));
#33589=CARTESIAN_POINT('Origin',(0.,0.,0.));
#33590=CARTESIAN_POINT('Ctrl Pts',(1.52655665885959E-15,5.,-28.));
#33591=CARTESIAN_POINT('Ctrl Pts',(0.629253024152622,5.,-28.));
#33592=CARTESIAN_POINT('Ctrl Pts',(1.29953505458189,4.87396779126795,-27.9766356618315));
#33593=CARTESIAN_POINT('Ctrl Pts',(2.53104134263485,4.3632766282051,-27.8921989820475));
#33594=CARTESIAN_POINT('Ctrl Pts',(3.09237623737018,3.97869157449529,-27.832297423241));
#33595=CARTESIAN_POINT('Ctrl Pts',(3.97870723422023,3.09236057764524,-27.7194782327905));
#33596=CARTESIAN_POINT('Ctrl Pts',(4.36328000904426,2.53103238085929,-27.6591541770631));
#33597=CARTESIAN_POINT('Ctrl Pts',(4.87396226264421,1.29954919562912,-27.5737468441049));
#33598=CARTESIAN_POINT('Ctrl Pts',(5.,0.629275259871354,-27.5499546279118));
#33599=CARTESIAN_POINT('Ctrl Pts',(5.,-0.629275259871354,-27.5499546279118));
#33600=CARTESIAN_POINT('Ctrl Pts',(4.87396226264421,-1.29954919562912,-27.5737468441049));
#33601=CARTESIAN_POINT('Ctrl Pts',(4.36328000904425,-2.53103238085929,-27.6591541770631));
#33602=CARTESIAN_POINT('Ctrl Pts',(3.97870723422023,-3.09236057764524,-27.7194782327905));
#33603=CARTESIAN_POINT('Ctrl Pts',(3.09237623737018,-3.9786915744953,-27.832297423241));
#33604=CARTESIAN_POINT('Ctrl Pts',(2.53104134263485,-4.3632766282051,-27.8921989820475));
#33605=CARTESIAN_POINT('Ctrl Pts',(1.29953505458189,-4.87396779126795,-27.9766356618315));
#33606=CARTESIAN_POINT('Ctrl Pts',(0.629253024152619,-5.,-28.));
#33607=CARTESIAN_POINT('Ctrl Pts',(-8.32667268468867E-16,-5.,-28.));
#33608=CARTESIAN_POINT('Origin',(0.,0.,0.));
#33609=CARTESIAN_POINT('Ctrl Pts',(1.87350135405495E-15,5.,-28.));
#33610=CARTESIAN_POINT('Ctrl Pts',(-0.629253024152618,5.,-28.));
#33611=CARTESIAN_POINT('Ctrl Pts',(-1.29953505458189,4.87396779126795,-27.9766356618315));
#33612=CARTESIAN_POINT('Ctrl Pts',(-2.53104134263485,4.3632766282051,-27.8921989820475));
#33613=CARTESIAN_POINT('Ctrl Pts',(-3.09237623737018,3.9786915744953,-27.832297423241));
#33614=CARTESIAN_POINT('Ctrl Pts',(-3.97870723422023,3.09236057764524,-27.7194782327905));
#33615=CARTESIAN_POINT('Ctrl Pts',(-4.36328000904426,2.53103238085929,-27.6591541770631));
#33616=CARTESIAN_POINT('Ctrl Pts',(-4.87396226264421,1.29954919562912,-27.5737468441049));
#33617=CARTESIAN_POINT('Ctrl Pts',(-5.,0.629275259871354,-27.5499546279118));
#33618=CARTESIAN_POINT('Ctrl Pts',(-5.,0.,-27.5499546279118));
#33619=CARTESIAN_POINT('Ctrl Pts',(-5.,-0.629275259871354,-27.5499546279118));
#33620=CARTESIAN_POINT('Ctrl Pts',(-4.87396226264421,-1.29954919562912,
-27.5737468441049));
#33621=CARTESIAN_POINT('Ctrl Pts',(-4.36328000904425,-2.53103238085929,
-27.6591541770631));
#33622=CARTESIAN_POINT('Ctrl Pts',(-3.97870723422023,-3.09236057764524,
-27.7194782327905));
#33623=CARTESIAN_POINT('Ctrl Pts',(-3.09237623737018,-3.9786915744953,-27.832297423241));
#33624=CARTESIAN_POINT('Ctrl Pts',(-2.53104134263485,-4.3632766282051,-27.8921989820475));
#33625=CARTESIAN_POINT('Ctrl Pts',(-1.29953505458189,-4.87396779126795,
-27.9766356618315));
#33626=CARTESIAN_POINT('Ctrl Pts',(-0.629253024152621,-5.,-28.));
#33627=CARTESIAN_POINT('Ctrl Pts',(-1.45716771982052E-15,-5.,-28.));
#33628=CARTESIAN_POINT('Origin',(0.,0.,0.));
#33629=CARTESIAN_POINT('',(-5.,4.16333634234434E-16,27.5499546279118));
#33630=CARTESIAN_POINT('Ctrl Pts',(-5.,-1.38777878078145E-16,27.5499546279118));
#33631=CARTESIAN_POINT('Ctrl Pts',(-5.,-0.629275259871354,27.5499546279118));
#33632=CARTESIAN_POINT('Ctrl Pts',(-4.87396226264421,-1.29954919562912,
27.5737468441049));
#33633=CARTESIAN_POINT('Ctrl Pts',(-4.36328000904425,-2.53103238085929,
27.6591541770631));
#33634=CARTESIAN_POINT('Ctrl Pts',(-3.97870723422023,-3.09236057764524,
27.7194782327905));
#33635=CARTESIAN_POINT('Ctrl Pts',(-3.09237623737018,-3.9786915744953,27.832297423241));
#33636=CARTESIAN_POINT('Ctrl Pts',(-2.53104134263485,-4.3632766282051,27.8921989820475));
#33637=CARTESIAN_POINT('Ctrl Pts',(-1.29953505458189,-4.87396779126795,
27.9766356618315));
#33638=CARTESIAN_POINT('Ctrl Pts',(-0.629253024152621,-5.,28.));
#33639=CARTESIAN_POINT('Ctrl Pts',(0.629253024152619,-5.,28.));
#33640=CARTESIAN_POINT('Ctrl Pts',(1.29953505458189,-4.87396779126795,27.9766356618315));
#33641=CARTESIAN_POINT('Ctrl Pts',(2.53104134263485,-4.3632766282051,27.8921989820475));
#33642=CARTESIAN_POINT('Ctrl Pts',(3.09237623737018,-3.9786915744953,27.832297423241));
#33643=CARTESIAN_POINT('Ctrl Pts',(3.97870723422023,-3.09236057764524,27.7194782327905));
#33644=CARTESIAN_POINT('Ctrl Pts',(4.36328000904425,-2.53103238085929,27.6591541770631));
#33645=CARTESIAN_POINT('Ctrl Pts',(4.87396226264421,-1.29954919562912,27.5737468441049));
#33646=CARTESIAN_POINT('Ctrl Pts',(5.,-0.629275259871354,27.5499546279118));
#33647=CARTESIAN_POINT('Ctrl Pts',(5.,0.629275259871354,27.5499546279118));
#33648=CARTESIAN_POINT('Ctrl Pts',(4.87396226264421,1.29954919562912,27.5737468441049));
#33649=CARTESIAN_POINT('Ctrl Pts',(4.36328000904426,2.53103238085929,27.6591541770631));
#33650=CARTESIAN_POINT('Ctrl Pts',(3.97870723422023,3.09236057764524,27.7194782327905));
#33651=CARTESIAN_POINT('Ctrl Pts',(3.09237623737018,3.9786915744953,27.832297423241));
#33652=CARTESIAN_POINT('Ctrl Pts',(2.53104134263485,4.3632766282051,27.8921989820475));
#33653=CARTESIAN_POINT('Ctrl Pts',(1.29953505458189,4.87396779126795,27.9766356618315));
#33654=CARTESIAN_POINT('Ctrl Pts',(0.629253024152622,5.,28.));
#33655=CARTESIAN_POINT('Ctrl Pts',(-0.629253024152618,5.,28.));
#33656=CARTESIAN_POINT('Ctrl Pts',(-1.29953505458188,4.87396779126795,27.9766356618315));
#33657=CARTESIAN_POINT('Ctrl Pts',(-2.53104134263485,4.3632766282051,27.8921989820475));
#33658=CARTESIAN_POINT('Ctrl Pts',(-3.09237623737017,3.9786915744953,27.832297423241));
#33659=CARTESIAN_POINT('Ctrl Pts',(-3.97870723422023,3.09236057764525,27.7194782327905));
#33660=CARTESIAN_POINT('Ctrl Pts',(-4.36328000904425,2.5310323808593,27.6591541770631));
#33661=CARTESIAN_POINT('Ctrl Pts',(-4.87396226264421,1.29954919562912,27.5737468441049));
#33662=CARTESIAN_POINT('Ctrl Pts',(-5.,0.629275259871355,27.5499546279118));
#33663=CARTESIAN_POINT('Ctrl Pts',(-5.,-1.38777878078145E-16,27.5499546279118));
#33664=CARTESIAN_POINT('',(-5.,-6.12323399573677E-16,31.3571312154738));
#33665=CARTESIAN_POINT('',(-5.,-6.12323399573677E-16,0.));
#33666=CARTESIAN_POINT('',(-2.7252308025327,-4.19203018511639,30.8799792272101));
#33667=CARTESIAN_POINT('Ctrl Pts',(-2.7252308025327,-4.19203018511639,30.8799792272101));
#33668=CARTESIAN_POINT('Ctrl Pts',(-2.8912176764087,-4.08412243600022,30.8653304951571));
#33669=CARTESIAN_POINT('Ctrl Pts',(-3.04862894705818,-3.96746986254389,
30.8620029267808));
#33670=CARTESIAN_POINT('Ctrl Pts',(-3.74387664835538,-3.39066664475822,
30.8821120697405));
#33671=CARTESIAN_POINT('Ctrl Pts',(-4.21066500973337,-2.79554609173792,
31.0137757194408));
#33672=CARTESIAN_POINT('Ctrl Pts',(-4.83880724780192,-1.45969207554558,
31.2576781989471));
#33673=CARTESIAN_POINT('Ctrl Pts',(-5.,-0.716580051177333,31.3571312154738));
#33674=CARTESIAN_POINT('Ctrl Pts',(-5.,-3.46944695195361E-16,31.3571312154738));
#33675=CARTESIAN_POINT('',(2.7252308025327,-4.1920301851164,30.8799792272101));
#33676=CARTESIAN_POINT('Ctrl Pts',(2.7252308025327,-4.19203018511639,30.8799792272101));
#33677=CARTESIAN_POINT('Ctrl Pts',(2.47095718963918,-4.35733297434463,30.9024194716491));
#33678=CARTESIAN_POINT('Ctrl Pts',(2.1983745065567,-4.50125462875714,30.923256490722));
#33679=CARTESIAN_POINT('Ctrl Pts',(1.29915176153723,-4.87407242020745,30.9789098121903));
#33680=CARTESIAN_POINT('Ctrl Pts',(0.62898575038369,-5.,31.));
#33681=CARTESIAN_POINT('Ctrl Pts',(-0.62898575038369,-5.,31.));
#33682=CARTESIAN_POINT('Ctrl Pts',(-1.29915176153723,-4.87407242020745,
30.9789098121903));
#33683=CARTESIAN_POINT('Ctrl Pts',(-2.1983745065567,-4.50125462875714,30.923256490722));
#33684=CARTESIAN_POINT('Ctrl Pts',(-2.47095718963918,-4.35733297434463,
30.9024194716491));
#33685=CARTESIAN_POINT('Ctrl Pts',(-2.7252308025327,-4.19203018511639,30.8799792272101));
#33686=CARTESIAN_POINT('',(2.7252308025327,4.1920301851164,30.8799792272101));
#33687=CARTESIAN_POINT('Ctrl Pts',(2.7252308025327,4.19203018511639,30.8799792272101));
#33688=CARTESIAN_POINT('Ctrl Pts',(2.89121767640869,4.08412243600022,30.8653304951571));
#33689=CARTESIAN_POINT('Ctrl Pts',(3.04862894705818,3.9674698625439,30.8620029267808));
#33690=CARTESIAN_POINT('Ctrl Pts',(3.74387664835538,3.39066664475823,30.8821120697405));
#33691=CARTESIAN_POINT('Ctrl Pts',(4.21066500973337,2.79554609173792,31.0137757194408));
#33692=CARTESIAN_POINT('Ctrl Pts',(4.83880724780192,1.45969207554558,31.2576781989471));
#33693=CARTESIAN_POINT('Ctrl Pts',(5.,0.716580051177333,31.3571312154738));
#33694=CARTESIAN_POINT('Ctrl Pts',(5.,-0.716580051177333,31.3571312154738));
#33695=CARTESIAN_POINT('Ctrl Pts',(4.83880724780192,-1.45969207554558,31.2576781989471));
#33696=CARTESIAN_POINT('Ctrl Pts',(4.21066500973337,-2.79554609173792,31.0137757194408));
#33697=CARTESIAN_POINT('Ctrl Pts',(3.74387664835538,-3.39066664475823,30.8821120697405));
#33698=CARTESIAN_POINT('Ctrl Pts',(3.04862894705818,-3.9674698625439,30.8620029267808));
#33699=CARTESIAN_POINT('Ctrl Pts',(2.89121767640869,-4.08412243600022,30.8653304951571));
#33700=CARTESIAN_POINT('Ctrl Pts',(2.7252308025327,-4.19203018511639,30.8799792272101));
#33701=CARTESIAN_POINT('',(-2.7252308025327,4.19203018511639,30.8799792272101));
#33702=CARTESIAN_POINT('Ctrl Pts',(-2.7252308025327,4.19203018511639,30.8799792272101));
#33703=CARTESIAN_POINT('Ctrl Pts',(-2.47095718963918,4.35733297434463,30.9024194716491));
#33704=CARTESIAN_POINT('Ctrl Pts',(-2.1983745065567,4.50125462875714,30.923256490722));
#33705=CARTESIAN_POINT('Ctrl Pts',(-1.29915176153723,4.87407242020745,30.9789098121903));
#33706=CARTESIAN_POINT('Ctrl Pts',(-0.62898575038369,5.,31.));
#33707=CARTESIAN_POINT('Ctrl Pts',(0.62898575038369,5.,31.));
#33708=CARTESIAN_POINT('Ctrl Pts',(1.29915176153722,4.87407242020745,30.9789098121903));
#33709=CARTESIAN_POINT('Ctrl Pts',(2.1983745065567,4.50125462875714,30.923256490722));
#33710=CARTESIAN_POINT('Ctrl Pts',(2.47095718963918,4.35733297434463,30.9024194716491));
#33711=CARTESIAN_POINT('Ctrl Pts',(2.7252308025327,4.1920301851164,30.8799792272101));
#33712=CARTESIAN_POINT('Ctrl Pts',(-5.,4.85722573273506E-16,31.3571312154738));
#33713=CARTESIAN_POINT('Ctrl Pts',(-5.,0.716580051177333,31.3571312154738));
#33714=CARTESIAN_POINT('Ctrl Pts',(-4.83880724780192,1.45969207554558,31.2576781989471));
#33715=CARTESIAN_POINT('Ctrl Pts',(-4.21066500973337,2.79554609173792,31.0137757194408));
#33716=CARTESIAN_POINT('Ctrl Pts',(-3.74387664835538,3.39066664475822,30.8821120697405));
#33717=CARTESIAN_POINT('Ctrl Pts',(-3.04862894705818,3.9674698625439,30.8620029267808));
#33718=CARTESIAN_POINT('Ctrl Pts',(-2.8912176764087,4.08412243600022,30.8653304951571));
#33719=CARTESIAN_POINT('Ctrl Pts',(-2.7252308025327,4.19203018511639,30.8799792272101));
#33720=CARTESIAN_POINT('Origin',(-3.07687348673047,0.,34.8644926758824));
#33721=CARTESIAN_POINT('',(-2.7252308025327,5.5,30.8799792272101));
#33722=CARTESIAN_POINT('',(-2.7252308025327,0.,30.8799792272101));
#33723=CARTESIAN_POINT('',(-6.78850072387334,5.5,33.3732437856903));
#33724=CARTESIAN_POINT('Origin',(-3.07687348673047,5.5,34.8644926758824));
#33725=CARTESIAN_POINT('',(-6.78850072387334,-5.5,33.3732437856903));
#33726=CARTESIAN_POINT('',(-6.78850072387334,0.,33.3732437856903));
#33727=CARTESIAN_POINT('',(-2.7252308025327,-5.5,30.8799792272101));
#33728=CARTESIAN_POINT('Origin',(-3.07687348673047,-5.5,34.8644926758824));
#33729=CARTESIAN_POINT('',(-2.7252308025327,0.,30.8799792272101));
#33730=CARTESIAN_POINT('Origin',(0.,0.,0.));
#33731=CARTESIAN_POINT('',(2.7252308025327,5.5,30.8799792272101));
#33732=CARTESIAN_POINT('',(2.7252308025327,0.,30.8799792272101));
#33733=CARTESIAN_POINT('Origin',(0.,5.5,0.));
#33734=CARTESIAN_POINT('Origin',(-3.07687348673047,0.,-34.8644926758824));
#33735=CARTESIAN_POINT('',(-2.7252308025327,-5.5,-30.8799792272101));
#33736=CARTESIAN_POINT('',(-2.7252308025327,0.,-30.8799792272101));
#33737=CARTESIAN_POINT('',(-6.78850072387334,-5.5,-33.3732437856903));
#33738=CARTESIAN_POINT('Origin',(-3.07687348673047,-5.5,-34.8644926758824));
#33739=CARTESIAN_POINT('',(-6.78850072387334,5.5,-33.3732437856903));
#33740=CARTESIAN_POINT('',(-6.78850072387334,0.,-33.3732437856903));
#33741=CARTESIAN_POINT('',(-2.7252308025327,5.5,-30.8799792272101));
#33742=CARTESIAN_POINT('Origin',(-3.07687348673047,5.5,-34.8644926758824));
#33743=CARTESIAN_POINT('',(-2.7252308025327,0.,-30.8799792272101));
#33744=CARTESIAN_POINT('Origin',(0.,0.,0.));
#33745=CARTESIAN_POINT('',(2.72523080253269,-5.5,-30.8799792272101));
#33746=CARTESIAN_POINT('',(2.72523080253269,0.,-30.8799792272101));
#33747=CARTESIAN_POINT('Origin',(0.,-5.5,0.));
#33748=CARTESIAN_POINT('Origin',(-3.07687348673047,5.5,34.8644926758824));
#33749=CARTESIAN_POINT('',(-2.68127546700798,6.,30.3819150461261));
#33750=CARTESIAN_POINT('Origin',(-2.68127546700798,5.5,30.3819150461261));
#33751=CARTESIAN_POINT('',(-7.2524541285162,6.,33.1868376744163));
#33752=CARTESIAN_POINT('Origin',(-3.07687348673047,6.,34.8644926758824));
#33753=CARTESIAN_POINT('Origin',(-7.2524541285162,5.5,33.1868376744163));
#33754=CARTESIAN_POINT('Origin',(-12.8198949842305,5.5,30.9499643391281));
#33755=CARTESIAN_POINT('',(-18.3383784711987,6.,28.5948974602351));
#33756=CARTESIAN_POINT('',(-18.7982520951128,5.5,28.398641886994));
#33757=CARTESIAN_POINT('Origin',(-18.3383784711987,5.5,28.5948974602351));
#33758=CARTESIAN_POINT('Origin',(-12.8198949842305,5.5,30.9499643391281));
#33759=CARTESIAN_POINT('Origin',(-12.8198949842305,6.,30.9499643391281));
#33760=CARTESIAN_POINT('Origin',(-22.4772410864249,5.5,26.8285973010654));
#33761=CARTESIAN_POINT('',(-19.5873100895989,6.,23.3792062194998));
#33762=CARTESIAN_POINT('',(-19.9084135336906,5.5,23.7624718952293));
#33763=CARTESIAN_POINT('Origin',(-19.5873100895989,5.5,23.3792062194998));
#33764=CARTESIAN_POINT('Origin',(-22.4772410864249,5.5,26.8285973010654));
#33765=CARTESIAN_POINT('Origin',(-22.4772410864249,6.,26.8285973010654));
#33766=CARTESIAN_POINT('Origin',(0.,5.5,0.));
#33767=CARTESIAN_POINT('',(-23.3792062194998,6.,19.5873100895989));
#33768=CARTESIAN_POINT('',(-23.7624718952293,5.5,19.9084135336906));
#33769=CARTESIAN_POINT('Origin',(-23.3792062194998,5.5,19.5873100895989));
#33770=CARTESIAN_POINT('Origin',(0.,5.5,0.));
#33771=CARTESIAN_POINT('Origin',(0.,6.,0.));
#33772=CARTESIAN_POINT('Origin',(-26.8285973010653,5.5,22.4772410864249));
#33773=CARTESIAN_POINT('',(-28.5948974602351,6.,18.3383784711987));
#33774=CARTESIAN_POINT('',(-28.398641886994,5.5,18.7982520951128));
#33775=CARTESIAN_POINT('Origin',(-28.5948974602351,5.5,18.3383784711987));
#33776=CARTESIAN_POINT('Origin',(-26.8285973010653,5.5,22.4772410864249));
#33777=CARTESIAN_POINT('Origin',(-26.8285973010653,6.,22.4772410864249));
#33778=CARTESIAN_POINT('Origin',(-30.9499643391281,5.5,12.8198949842305));
#33779=CARTESIAN_POINT('',(-33.1868376744162,6.,7.2524541285162));
#33780=CARTESIAN_POINT('',(-33.3732437856903,5.5,6.78850072387334));
#33781=CARTESIAN_POINT('Origin',(-33.1868376744162,5.5,7.2524541285162));
#33782=CARTESIAN_POINT('Origin',(-30.9499643391281,5.5,12.8198949842305));
#33783=CARTESIAN_POINT('Origin',(-30.9499643391281,6.,12.8198949842305));
#33784=CARTESIAN_POINT('Origin',(-34.8644926758824,5.5,3.07687348673047));
#33785=CARTESIAN_POINT('',(-30.3819150461261,6.,2.68127546700798));
#33786=CARTESIAN_POINT('',(-30.8799792272101,5.5,2.7252308025327));
#33787=CARTESIAN_POINT('Origin',(-30.3819150461261,5.5,2.68127546700798));
#33788=CARTESIAN_POINT('Origin',(-34.8644926758824,5.5,3.07687348673047));
#33789=CARTESIAN_POINT('Origin',(-34.8644926758824,6.,3.07687348673047));
#33790=CARTESIAN_POINT('Origin',(0.,5.5,0.));
#33791=CARTESIAN_POINT('',(-30.3819150461261,6.,-2.68127546700797));
#33792=CARTESIAN_POINT('',(-30.8799792272101,5.5,-2.7252308025327));
#33793=CARTESIAN_POINT('Origin',(-30.3819150461261,5.5,-2.68127546700797));
#33794=CARTESIAN_POINT('Origin',(0.,5.5,0.));
#33795=CARTESIAN_POINT('Origin',(0.,6.,0.));
#33796=CARTESIAN_POINT('Origin',(-34.8644926758824,5.5,-3.07687348673046));
#33797=CARTESIAN_POINT('',(-33.1868376744163,6.,-7.2524541285162));
#33798=CARTESIAN_POINT('',(-33.3732437856903,5.5,-6.78850072387334));
#33799=CARTESIAN_POINT('Origin',(-33.1868376744163,5.5,-7.2524541285162));
#33800=CARTESIAN_POINT('Origin',(-34.8644926758824,5.5,-3.07687348673046));
#33801=CARTESIAN_POINT('Origin',(-34.8644926758824,6.,-3.07687348673046));
#33802=CARTESIAN_POINT('Origin',(-30.9499643391281,5.5,-12.8198949842305));
#33803=CARTESIAN_POINT('',(-28.5948974602351,6.,-18.3383784711987));
#33804=CARTESIAN_POINT('',(-28.398641886994,5.5,-18.7982520951128));
#33805=CARTESIAN_POINT('Origin',(-28.5948974602351,5.5,-18.3383784711987));
#33806=CARTESIAN_POINT('Origin',(-30.9499643391281,5.5,-12.8198949842305));
#33807=CARTESIAN_POINT('Origin',(-30.9499643391281,6.,-12.8198949842305));
#33808=CARTESIAN_POINT('Origin',(-26.8285973010653,5.5,-22.4772410864249));
#33809=CARTESIAN_POINT('',(-23.3792062194998,6.,-19.5873100895989));
#33810=CARTESIAN_POINT('',(-23.7624718952293,5.5,-19.9084135336907));
#33811=CARTESIAN_POINT('Origin',(-23.3792062194998,5.5,-19.5873100895989));
#33812=CARTESIAN_POINT('Origin',(-26.8285973010653,5.5,-22.4772410864249));
#33813=CARTESIAN_POINT('Origin',(-26.8285973010653,6.,-22.4772410864249));
#33814=CARTESIAN_POINT('Origin',(0.,5.5,0.));
#33815=CARTESIAN_POINT('',(-19.5873100895989,6.,-23.3792062194998));
#33816=CARTESIAN_POINT('',(-19.9084135336907,5.5,-23.7624718952293));
#33817=CARTESIAN_POINT('Origin',(-19.5873100895989,5.5,-23.3792062194998));
#33818=CARTESIAN_POINT('Origin',(0.,5.5,0.));
#33819=CARTESIAN_POINT('Origin',(0.,6.,0.));
#33820=CARTESIAN_POINT('Origin',(-22.4772410864249,5.5,-26.8285973010653));
#33821=CARTESIAN_POINT('',(-18.3383784711988,6.,-28.5948974602351));
#33822=CARTESIAN_POINT('',(-18.7982520951128,5.5,-28.398641886994));
#33823=CARTESIAN_POINT('Origin',(-18.3383784711988,5.5,-28.5948974602351));
#33824=CARTESIAN_POINT('Origin',(-22.4772410864249,5.5,-26.8285973010653));
#33825=CARTESIAN_POINT('Origin',(-22.4772410864249,6.,-26.8285973010653));
#33826=CARTESIAN_POINT('Origin',(-12.8198949842305,5.5,-30.9499643391281));
#33827=CARTESIAN_POINT('',(-7.2524541285162,6.,-33.1868376744162));
#33828=CARTESIAN_POINT('Origin',(-7.2524541285162,5.5,-33.1868376744162));
#33829=CARTESIAN_POINT('Origin',(-12.8198949842305,5.5,-30.9499643391281));
#33830=CARTESIAN_POINT('Origin',(-12.8198949842305,6.,-30.9499643391281));
#33831=CARTESIAN_POINT('Origin',(-3.07687348673047,5.5,-34.8644926758824));
#33832=CARTESIAN_POINT('',(-2.68127546700798,6.,-30.3819150461261));
#33833=CARTESIAN_POINT('Origin',(-2.68127546700798,5.5,-30.3819150461261));
#33834=CARTESIAN_POINT('Origin',(-3.07687348673047,6.,-34.8644926758824));
#33835=CARTESIAN_POINT('Origin',(0.,5.5,0.));
#33836=CARTESIAN_POINT('',(2.68127546700797,6.,-30.3819150461261));
#33837=CARTESIAN_POINT('',(2.72523080253269,5.5,-30.8799792272101));
#33838=CARTESIAN_POINT('Origin',(2.68127546700797,5.5,-30.3819150461261));
#33839=CARTESIAN_POINT('Origin',(0.,5.5,0.));
#33840=CARTESIAN_POINT('Origin',(0.,6.,0.));
#33841=CARTESIAN_POINT('Origin',(3.07687348673046,5.5,-34.8644926758824));
#33842=CARTESIAN_POINT('',(7.25245412851619,6.,-33.1868376744163));
#33843=CARTESIAN_POINT('',(6.78850072387333,5.5,-33.3732437856903));
#33844=CARTESIAN_POINT('Origin',(7.25245412851619,5.5,-33.1868376744163));
#33845=CARTESIAN_POINT('Origin',(3.07687348673046,5.5,-34.8644926758824));
#33846=CARTESIAN_POINT('Origin',(3.07687348673046,6.,-34.8644926758824));
#33847=CARTESIAN_POINT('Origin',(12.8198949842305,5.5,-30.9499643391281));
#33848=CARTESIAN_POINT('',(18.3383784711987,6.,-28.5948974602351));
#33849=CARTESIAN_POINT('',(18.7982520951128,5.5,-28.398641886994));
#33850=CARTESIAN_POINT('Origin',(18.3383784711987,5.5,-28.5948974602351));
#33851=CARTESIAN_POINT('Origin',(12.8198949842305,5.5,-30.9499643391281));
#33852=CARTESIAN_POINT('Origin',(12.8198949842305,6.,-30.9499643391281));
#33853=CARTESIAN_POINT('Origin',(22.4772410864249,5.5,-26.8285973010653));
#33854=CARTESIAN_POINT('',(19.5873100895989,6.,-23.3792062194998));
#33855=CARTESIAN_POINT('',(19.9084135336907,5.5,-23.7624718952293));
#33856=CARTESIAN_POINT('Origin',(19.5873100895989,5.5,-23.3792062194998));
#33857=CARTESIAN_POINT('Origin',(22.4772410864249,5.5,-26.8285973010653));
#33858=CARTESIAN_POINT('Origin',(22.4772410864249,6.,-26.8285973010653));
#33859=CARTESIAN_POINT('Origin',(0.,5.5,0.));
#33860=CARTESIAN_POINT('',(23.3792062194998,6.,-19.5873100895989));
#33861=CARTESIAN_POINT('',(23.7624718952293,5.5,-19.9084135336907));
#33862=CARTESIAN_POINT('Origin',(23.3792062194998,5.5,-19.5873100895989));
#33863=CARTESIAN_POINT('Origin',(0.,5.5,0.));
#33864=CARTESIAN_POINT('Origin',(0.,6.,0.));
#33865=CARTESIAN_POINT('Origin',(26.8285973010653,5.5,-22.4772410864249));
#33866=CARTESIAN_POINT('',(28.5948974602351,6.,-18.3383784711987));
#33867=CARTESIAN_POINT('',(28.398641886994,5.5,-18.7982520951128));
#33868=CARTESIAN_POINT('Origin',(28.5948974602351,5.5,-18.3383784711987));
#33869=CARTESIAN_POINT('Origin',(26.8285973010653,5.5,-22.4772410864249));
#33870=CARTESIAN_POINT('Origin',(26.8285973010653,6.,-22.4772410864249));
#33871=CARTESIAN_POINT('Origin',(30.9499643391281,5.5,-12.8198949842305));
#33872=CARTESIAN_POINT('',(33.1868376744162,6.,-7.25245412851619));
#33873=CARTESIAN_POINT('',(33.3732437856903,5.5,-6.78850072387333));
#33874=CARTESIAN_POINT('Origin',(33.1868376744162,5.5,-7.25245412851619));
#33875=CARTESIAN_POINT('Origin',(30.9499643391281,5.5,-12.8198949842305));
#33876=CARTESIAN_POINT('Origin',(30.9499643391281,6.,-12.8198949842305));
#33877=CARTESIAN_POINT('Origin',(34.8644926758824,5.5,-3.07687348673046));
#33878=CARTESIAN_POINT('',(30.3819150461261,6.,-2.68127546700797));
#33879=CARTESIAN_POINT('',(30.8799792272101,5.5,-2.72523080253269));
#33880=CARTESIAN_POINT('Origin',(30.3819150461261,5.5,-2.68127546700797));
#33881=CARTESIAN_POINT('Origin',(34.8644926758824,5.5,-3.07687348673046));
#33882=CARTESIAN_POINT('Origin',(34.8644926758824,6.,-3.07687348673046));
#33883=CARTESIAN_POINT('Origin',(0.,5.5,0.));
#33884=CARTESIAN_POINT('',(30.3819150461261,6.,2.68127546700798));
#33885=CARTESIAN_POINT('',(30.8799792272101,5.5,2.7252308025327));
#33886=CARTESIAN_POINT('Origin',(30.3819150461261,5.5,2.68127546700798));
#33887=CARTESIAN_POINT('Origin',(0.,5.5,0.));
#33888=CARTESIAN_POINT('Origin',(0.,6.,0.));
#33889=CARTESIAN_POINT('Origin',(34.8644926758824,5.5,3.07687348673047));
#33890=CARTESIAN_POINT('',(33.1868376744163,6.,7.2524541285162));
#33891=CARTESIAN_POINT('',(33.3732437856903,5.5,6.78850072387334));
#33892=CARTESIAN_POINT('Origin',(33.1868376744163,5.5,7.2524541285162));
#33893=CARTESIAN_POINT('Origin',(34.8644926758824,5.5,3.07687348673047));
#33894=CARTESIAN_POINT('Origin',(34.8644926758824,6.,3.07687348673047));
#33895=CARTESIAN_POINT('Origin',(30.9499643391281,5.5,12.8198949842305));
#33896=CARTESIAN_POINT('',(28.5948974602351,6.,18.3383784711987));
#33897=CARTESIAN_POINT('',(28.398641886994,5.5,18.7982520951128));
#33898=CARTESIAN_POINT('Origin',(28.5948974602351,5.5,18.3383784711987));
#33899=CARTESIAN_POINT('Origin',(30.9499643391281,5.5,12.8198949842305));
#33900=CARTESIAN_POINT('Origin',(30.9499643391281,6.,12.8198949842305));
#33901=CARTESIAN_POINT('Origin',(26.8285973010654,5.5,22.4772410864249));
#33902=CARTESIAN_POINT('',(23.3792062194998,6.,19.5873100895989));
#33903=CARTESIAN_POINT('',(23.7624718952293,5.5,19.9084135336906));
#33904=CARTESIAN_POINT('Origin',(23.3792062194998,5.5,19.5873100895989));
#33905=CARTESIAN_POINT('Origin',(26.8285973010654,5.5,22.4772410864249));
#33906=CARTESIAN_POINT('Origin',(26.8285973010654,6.,22.4772410864249));
#33907=CARTESIAN_POINT('Origin',(0.,5.5,0.));
#33908=CARTESIAN_POINT('',(19.5873100895989,6.,23.3792062194998));
#33909=CARTESIAN_POINT('',(19.9084135336907,5.5,23.7624718952293));
#33910=CARTESIAN_POINT('Origin',(19.5873100895989,5.5,23.3792062194998));
#33911=CARTESIAN_POINT('Origin',(0.,5.5,0.));
#33912=CARTESIAN_POINT('Origin',(0.,6.,0.));
#33913=CARTESIAN_POINT('Origin',(22.4772410864249,5.5,26.8285973010653));
#33914=CARTESIAN_POINT('',(18.3383784711988,6.,28.5948974602351));
#33915=CARTESIAN_POINT('',(18.7982520951128,5.5,28.398641886994));
#33916=CARTESIAN_POINT('Origin',(18.3383784711988,5.5,28.5948974602351));
#33917=CARTESIAN_POINT('Origin',(22.4772410864249,5.5,26.8285973010653));
#33918=CARTESIAN_POINT('Origin',(22.4772410864249,6.,26.8285973010653));
#33919=CARTESIAN_POINT('Origin',(12.8198949842305,5.5,30.9499643391281));
#33920=CARTESIAN_POINT('',(7.2524541285162,6.,33.1868376744162));
#33921=CARTESIAN_POINT('',(6.78850072387334,5.5,33.3732437856903));
#33922=CARTESIAN_POINT('Origin',(7.2524541285162,5.5,33.1868376744162));
#33923=CARTESIAN_POINT('Origin',(12.8198949842305,5.5,30.9499643391281));
#33924=CARTESIAN_POINT('Origin',(12.8198949842305,6.,30.9499643391281));
#33925=CARTESIAN_POINT('Origin',(3.07687348673046,5.5,34.8644926758824));
#33926=CARTESIAN_POINT('',(2.68127546700797,6.,30.3819150461261));
#33927=CARTESIAN_POINT('Origin',(2.68127546700797,5.5,30.3819150461261));
#33928=CARTESIAN_POINT('Origin',(3.07687348673046,5.5,34.8644926758824));
#33929=CARTESIAN_POINT('Origin',(3.07687348673046,6.,34.8644926758824));
#33930=CARTESIAN_POINT('Origin',(0.,5.5,0.));
#33931=CARTESIAN_POINT('Origin',(0.,6.,0.));
#33932=CARTESIAN_POINT('Origin',(12.8198949842305,0.,-30.9499643391281));
#33933=CARTESIAN_POINT('',(18.7982520951128,-5.5,-28.398641886994));
#33934=CARTESIAN_POINT('',(18.7982520951128,0.,-28.398641886994));
#33935=CARTESIAN_POINT('',(6.78850072387333,-5.5,-33.3732437856903));
#33936=CARTESIAN_POINT('Origin',(12.8198949842305,-5.5,-30.9499643391281));
#33937=CARTESIAN_POINT('',(6.78850072387333,0.,-33.3732437856903));
#33938=CARTESIAN_POINT('Origin',(22.4772410864249,0.,-26.8285973010653));
#33939=CARTESIAN_POINT('',(19.9084135336907,-5.5,-23.7624718952293));
#33940=CARTESIAN_POINT('',(19.9084135336907,0.,-23.7624718952293));
#33941=CARTESIAN_POINT('Origin',(22.4772410864249,-5.5,-26.8285973010653));
#33942=CARTESIAN_POINT('Origin',(0.,0.,0.));
#33943=CARTESIAN_POINT('',(23.7624718952293,-5.5,-19.9084135336907));
#33944=CARTESIAN_POINT('',(23.7624718952293,0.,-19.9084135336907));
#33945=CARTESIAN_POINT('Origin',(0.,-5.5,0.));
#33946=CARTESIAN_POINT('Origin',(26.8285973010653,0.,-22.4772410864249));
#33947=CARTESIAN_POINT('',(28.398641886994,-5.5,-18.7982520951128));
#33948=CARTESIAN_POINT('',(28.398641886994,0.,-18.7982520951128));
#33949=CARTESIAN_POINT('Origin',(26.8285973010653,-5.5,-22.4772410864249));
#33950=CARTESIAN_POINT('Origin',(30.9499643391281,0.,-12.8198949842305));
#33951=CARTESIAN_POINT('',(33.3732437856903,-5.5,-6.78850072387333));
#33952=CARTESIAN_POINT('',(33.3732437856903,0.,-6.78850072387333));
#33953=CARTESIAN_POINT('Origin',(30.9499643391281,-5.5,-12.8198949842305));
#33954=CARTESIAN_POINT('Origin',(34.8644926758824,0.,-3.07687348673046));
#33955=CARTESIAN_POINT('',(30.8799792272101,-5.5,-2.72523080253269));
#33956=CARTESIAN_POINT('',(30.8799792272101,0.,-2.72523080253269));
#33957=CARTESIAN_POINT('Origin',(34.8644926758824,-5.5,-3.07687348673046));
#33958=CARTESIAN_POINT('Origin',(0.,0.,0.));
#33959=CARTESIAN_POINT('',(30.8799792272101,-5.5,2.7252308025327));
#33960=CARTESIAN_POINT('',(30.8799792272101,0.,2.7252308025327));
#33961=CARTESIAN_POINT('Origin',(0.,-5.5,0.));
#33962=CARTESIAN_POINT('Origin',(34.8644926758824,0.,3.07687348673047));
#33963=CARTESIAN_POINT('',(33.3732437856903,-5.5,6.78850072387334));
#33964=CARTESIAN_POINT('',(33.3732437856903,0.,6.78850072387334));
#33965=CARTESIAN_POINT('Origin',(34.8644926758824,-5.5,3.07687348673047));
#33966=CARTESIAN_POINT('Origin',(30.9499643391281,0.,12.8198949842305));
#33967=CARTESIAN_POINT('',(28.398641886994,-5.5,18.7982520951128));
#33968=CARTESIAN_POINT('',(28.398641886994,0.,18.7982520951128));
#33969=CARTESIAN_POINT('Origin',(30.9499643391281,-5.5,12.8198949842305));
#33970=CARTESIAN_POINT('Origin',(26.8285973010654,0.,22.4772410864249));
#33971=CARTESIAN_POINT('',(23.7624718952293,-5.5,19.9084135336906));
#33972=CARTESIAN_POINT('',(23.7624718952293,0.,19.9084135336906));
#33973=CARTESIAN_POINT('Origin',(26.8285973010654,-5.5,22.4772410864249));
#33974=CARTESIAN_POINT('Origin',(0.,0.,0.));
#33975=CARTESIAN_POINT('',(19.9084135336907,-5.5,23.7624718952293));
#33976=CARTESIAN_POINT('',(19.9084135336907,0.,23.7624718952293));
#33977=CARTESIAN_POINT('Origin',(0.,-5.5,0.));
#33978=CARTESIAN_POINT('Origin',(22.4772410864249,0.,26.8285973010653));
#33979=CARTESIAN_POINT('',(18.7982520951128,-5.5,28.398641886994));
#33980=CARTESIAN_POINT('',(18.7982520951128,0.,28.398641886994));
#33981=CARTESIAN_POINT('Origin',(22.4772410864249,-5.5,26.8285973010653));
#33982=CARTESIAN_POINT('Origin',(12.8198949842305,0.,30.9499643391281));
#33983=CARTESIAN_POINT('',(6.78850072387334,-5.5,33.3732437856903));
#33984=CARTESIAN_POINT('',(6.78850072387334,0.,33.3732437856903));
#33985=CARTESIAN_POINT('Origin',(12.8198949842305,-5.5,30.9499643391281));
#33986=CARTESIAN_POINT('Origin',(3.07687348673046,0.,34.8644926758824));
#33987=CARTESIAN_POINT('',(2.7252308025327,-5.5,30.8799792272101));
#33988=CARTESIAN_POINT('',(2.7252308025327,0.,30.8799792272101));
#33989=CARTESIAN_POINT('Origin',(3.07687348673046,-5.5,34.8644926758824));
#33990=CARTESIAN_POINT('Origin',(0.,0.,0.));
#33991=CARTESIAN_POINT('Origin',(0.,-5.5,0.));
#33992=CARTESIAN_POINT('Origin',(0.,6.,0.));
#33993=CARTESIAN_POINT('',(-3.49024337756996E-15,6.,28.5));
#33994=CARTESIAN_POINT('Origin',(0.,6.,0.));
#33995=CARTESIAN_POINT('',(-12.2458698356829,6.,-29.5641450403612));
#33996=CARTESIAN_POINT('Origin',(-12.8198949842305,6.,-30.9499643391281));
#33997=CARTESIAN_POINT('',(-29.5641450403612,6.,12.2458698356829));
#33998=CARTESIAN_POINT('Origin',(-30.9499643391281,6.,12.8198949842305));
#33999=CARTESIAN_POINT('',(-29.5641450403612,6.,-12.2458698356829));
#34000=CARTESIAN_POINT('Origin',(-30.9499643391281,6.,-12.8198949842305));
#34001=CARTESIAN_POINT('',(29.5641450403612,6.,-12.2458698356829));
#34002=CARTESIAN_POINT('Origin',(30.9499643391281,6.,-12.8198949842305));
#34003=CARTESIAN_POINT('',(29.5641450403612,6.,12.2458698356829));
#34004=CARTESIAN_POINT('Origin',(30.9499643391281,6.,12.8198949842305));
#34005=CARTESIAN_POINT('',(12.2458698356829,6.,-29.5641450403612));
#34006=CARTESIAN_POINT('Origin',(12.8198949842305,6.,-30.9499643391281));
#34007=CARTESIAN_POINT('',(12.2458698356829,6.,29.5641450403612));
#34008=CARTESIAN_POINT('Origin',(12.8198949842305,6.,30.9499643391281));
#34009=CARTESIAN_POINT('',(-12.2458698356829,6.,29.5641450403612));
#34010=CARTESIAN_POINT('Origin',(-12.8198949842305,6.,30.9499643391281));
#34011=CARTESIAN_POINT('Origin',(-22.4772410864249,-5.5,26.8285973010654));
#34012=CARTESIAN_POINT('',(-19.9084135336906,-5.5,23.7624718952293));
#34013=CARTESIAN_POINT('',(-19.5873100895989,-6.,23.3792062194998));
#34014=CARTESIAN_POINT('Origin',(-19.5873100895989,-5.5,23.3792062194998));
#34015=CARTESIAN_POINT('',(-18.3383784711987,-6.,28.5948974602351));
#34016=CARTESIAN_POINT('Origin',(-22.4772410864249,-6.,26.8285973010654));
#34017=CARTESIAN_POINT('',(-18.7982520951128,-5.5,28.398641886994));
#34018=CARTESIAN_POINT('Origin',(-18.3383784711987,-5.5,28.5948974602351));
#34019=CARTESIAN_POINT('Origin',(-22.4772410864249,-5.5,26.8285973010654));
#34020=CARTESIAN_POINT('Origin',(-12.8198949842305,-5.5,30.9499643391281));
#34021=CARTESIAN_POINT('',(-7.2524541285162,-6.,33.1868376744163));
#34022=CARTESIAN_POINT('Origin',(-7.2524541285162,-5.5,33.1868376744163));
#34023=CARTESIAN_POINT('Origin',(-12.8198949842305,-5.5,30.9499643391281));
#34024=CARTESIAN_POINT('Origin',(-12.8198949842305,-6.,30.9499643391281));
#34025=CARTESIAN_POINT('Origin',(-3.07687348673047,-5.5,34.8644926758824));
#34026=CARTESIAN_POINT('',(-2.68127546700798,-6.,30.3819150461261));
#34027=CARTESIAN_POINT('Origin',(-2.68127546700798,-5.5,30.3819150461261));
#34028=CARTESIAN_POINT('Origin',(-3.07687348673047,-6.,34.8644926758824));
#34029=CARTESIAN_POINT('Origin',(0.,-5.5,0.));
#34030=CARTESIAN_POINT('',(2.68127546700797,-6.,30.3819150461261));
#34031=CARTESIAN_POINT('Origin',(2.68127546700797,-5.5,30.3819150461261));
#34032=CARTESIAN_POINT('Origin',(0.,-6.,0.));
#34033=CARTESIAN_POINT('Origin',(3.07687348673046,-5.5,34.8644926758824));
#34034=CARTESIAN_POINT('',(7.2524541285162,-6.,33.1868376744163));
#34035=CARTESIAN_POINT('Origin',(7.2524541285162,-5.5,33.1868376744163));
#34036=CARTESIAN_POINT('Origin',(3.07687348673046,-6.,34.8644926758824));
#34037=CARTESIAN_POINT('Origin',(12.8198949842305,-5.5,30.9499643391281));
#34038=CARTESIAN_POINT('',(18.3383784711987,-6.,28.5948974602351));
#34039=CARTESIAN_POINT('Origin',(18.3383784711987,-5.5,28.5948974602351));
#34040=CARTESIAN_POINT('Origin',(12.8198949842305,-6.,30.9499643391281));
#34041=CARTESIAN_POINT('Origin',(22.4772410864249,-5.5,26.8285973010653));
#34042=CARTESIAN_POINT('',(19.5873100895989,-6.,23.3792062194998));
#34043=CARTESIAN_POINT('Origin',(19.5873100895989,-5.5,23.3792062194998));
#34044=CARTESIAN_POINT('Origin',(22.4772410864249,-6.,26.8285973010653));
#34045=CARTESIAN_POINT('Origin',(0.,-5.5,0.));
#34046=CARTESIAN_POINT('',(23.3792062194998,-6.,19.5873100895989));
#34047=CARTESIAN_POINT('Origin',(23.3792062194998,-5.5,19.5873100895989));
#34048=CARTESIAN_POINT('Origin',(0.,-6.,0.));
#34049=CARTESIAN_POINT('Origin',(26.8285973010654,-5.5,22.4772410864249));
#34050=CARTESIAN_POINT('',(28.5948974602351,-6.,18.3383784711987));
#34051=CARTESIAN_POINT('Origin',(28.5948974602351,-5.5,18.3383784711987));
#34052=CARTESIAN_POINT('Origin',(26.8285973010654,-6.,22.4772410864249));
#34053=CARTESIAN_POINT('Origin',(30.9499643391281,-5.5,12.8198949842305));
#34054=CARTESIAN_POINT('',(33.1868376744163,-6.,7.2524541285162));
#34055=CARTESIAN_POINT('Origin',(33.1868376744163,-5.5,7.2524541285162));
#34056=CARTESIAN_POINT('Origin',(30.9499643391281,-6.,12.8198949842305));
#34057=CARTESIAN_POINT('Origin',(34.8644926758824,-5.5,3.07687348673047));
#34058=CARTESIAN_POINT('',(30.3819150461261,-6.,2.68127546700798));
#34059=CARTESIAN_POINT('Origin',(30.3819150461261,-5.5,2.68127546700798));
#34060=CARTESIAN_POINT('Origin',(34.8644926758824,-6.,3.07687348673047));
#34061=CARTESIAN_POINT('Origin',(0.,-5.5,0.));
#34062=CARTESIAN_POINT('',(30.3819150461261,-6.,-2.68127546700797));
#34063=CARTESIAN_POINT('Origin',(30.3819150461261,-5.5,-2.68127546700797));
#34064=CARTESIAN_POINT('Origin',(0.,-6.,0.));
#34065=CARTESIAN_POINT('Origin',(34.8644926758824,-5.5,-3.07687348673046));
#34066=CARTESIAN_POINT('',(33.1868376744163,-6.,-7.25245412851619));
#34067=CARTESIAN_POINT('Origin',(33.1868376744163,-5.5,-7.25245412851619));
#34068=CARTESIAN_POINT('Origin',(34.8644926758824,-6.,-3.07687348673046));
#34069=CARTESIAN_POINT('Origin',(30.9499643391281,-5.5,-12.8198949842305));
#34070=CARTESIAN_POINT('',(28.5948974602351,-6.,-18.3383784711987));
#34071=CARTESIAN_POINT('Origin',(28.5948974602351,-5.5,-18.3383784711987));
#34072=CARTESIAN_POINT('Origin',(30.9499643391281,-6.,-12.8198949842305));
#34073=CARTESIAN_POINT('Origin',(26.8285973010653,-5.5,-22.4772410864249));
#34074=CARTESIAN_POINT('',(23.3792062194998,-6.,-19.5873100895989));
#34075=CARTESIAN_POINT('Origin',(23.3792062194998,-5.5,-19.5873100895989));
#34076=CARTESIAN_POINT('Origin',(26.8285973010653,-6.,-22.4772410864249));
#34077=CARTESIAN_POINT('Origin',(0.,-5.5,0.));
#34078=CARTESIAN_POINT('',(19.5873100895989,-6.,-23.3792062194998));
#34079=CARTESIAN_POINT('Origin',(19.5873100895989,-5.5,-23.3792062194998));
#34080=CARTESIAN_POINT('Origin',(0.,-6.,0.));
#34081=CARTESIAN_POINT('Origin',(22.4772410864249,-5.5,-26.8285973010653));
#34082=CARTESIAN_POINT('',(18.3383784711987,-6.,-28.5948974602351));
#34083=CARTESIAN_POINT('Origin',(18.3383784711987,-5.5,-28.5948974602351));
#34084=CARTESIAN_POINT('Origin',(22.4772410864249,-6.,-26.8285973010653));
#34085=CARTESIAN_POINT('Origin',(12.8198949842305,-5.5,-30.9499643391281));
#34086=CARTESIAN_POINT('',(7.25245412851619,-6.,-33.1868376744163));
#34087=CARTESIAN_POINT('Origin',(7.25245412851619,-5.5,-33.1868376744163));
#34088=CARTESIAN_POINT('Origin',(12.8198949842305,-6.,-30.9499643391281));
#34089=CARTESIAN_POINT('Origin',(3.07687348673046,-5.5,-34.8644926758824));
#34090=CARTESIAN_POINT('',(2.68127546700797,-6.,-30.3819150461261));
#34091=CARTESIAN_POINT('Origin',(2.68127546700797,-5.5,-30.3819150461261));
#34092=CARTESIAN_POINT('Origin',(3.07687348673046,-5.5,-34.8644926758824));
#34093=CARTESIAN_POINT('Origin',(3.07687348673046,-6.,-34.8644926758824));
#34094=CARTESIAN_POINT('Origin',(0.,-5.5,0.));
#34095=CARTESIAN_POINT('',(-2.68127546700798,-6.,-30.3819150461261));
#34096=CARTESIAN_POINT('Origin',(-2.68127546700798,-5.5,-30.3819150461261));
#34097=CARTESIAN_POINT('Origin',(0.,-6.,0.));
#34098=CARTESIAN_POINT('Origin',(-3.07687348673047,-5.5,-34.8644926758824));
#34099=CARTESIAN_POINT('',(-7.2524541285162,-6.,-33.1868376744162));
#34100=CARTESIAN_POINT('Origin',(-7.2524541285162,-5.5,-33.1868376744162));
#34101=CARTESIAN_POINT('Origin',(-3.07687348673047,-6.,-34.8644926758824));
#34102=CARTESIAN_POINT('Origin',(-12.8198949842305,-5.5,-30.9499643391281));
#34103=CARTESIAN_POINT('',(-18.3383784711988,-6.,-28.5948974602351));
#34104=CARTESIAN_POINT('',(-18.7982520951128,-5.5,-28.398641886994));
#34105=CARTESIAN_POINT('Origin',(-18.3383784711988,-5.5,-28.5948974602351));
#34106=CARTESIAN_POINT('Origin',(-12.8198949842305,-5.5,-30.9499643391281));
#34107=CARTESIAN_POINT('Origin',(-12.8198949842305,-6.,-30.9499643391281));
#34108=CARTESIAN_POINT('Origin',(-22.4772410864249,-5.5,-26.8285973010653));
#34109=CARTESIAN_POINT('',(-19.5873100895989,-6.,-23.3792062194998));
#34110=CARTESIAN_POINT('',(-19.9084135336907,-5.5,-23.7624718952293));
#34111=CARTESIAN_POINT('Origin',(-19.5873100895989,-5.5,-23.3792062194998));
#34112=CARTESIAN_POINT('Origin',(-22.4772410864249,-5.5,-26.8285973010653));
#34113=CARTESIAN_POINT('Origin',(-22.4772410864249,-6.,-26.8285973010653));
#34114=CARTESIAN_POINT('Origin',(0.,-5.5,0.));
#34115=CARTESIAN_POINT('',(-23.3792062194998,-6.,-19.5873100895989));
#34116=CARTESIAN_POINT('',(-23.7624718952293,-5.5,-19.9084135336907));
#34117=CARTESIAN_POINT('Origin',(-23.3792062194998,-5.5,-19.5873100895989));
#34118=CARTESIAN_POINT('Origin',(0.,-5.5,0.));
#34119=CARTESIAN_POINT('Origin',(0.,-6.,0.));
#34120=CARTESIAN_POINT('Origin',(-26.8285973010653,-5.5,-22.4772410864249));
#34121=CARTESIAN_POINT('',(-28.5948974602351,-6.,-18.3383784711987));
#34122=CARTESIAN_POINT('',(-28.398641886994,-5.5,-18.7982520951128));
#34123=CARTESIAN_POINT('Origin',(-28.5948974602351,-5.5,-18.3383784711987));
#34124=CARTESIAN_POINT('Origin',(-26.8285973010653,-5.5,-22.4772410864249));
#34125=CARTESIAN_POINT('Origin',(-26.8285973010653,-6.,-22.4772410864249));
#34126=CARTESIAN_POINT('Origin',(-30.9499643391281,-5.5,-12.8198949842305));
#34127=CARTESIAN_POINT('',(-33.1868376744163,-6.,-7.2524541285162));
#34128=CARTESIAN_POINT('',(-33.3732437856903,-5.5,-6.78850072387334));
#34129=CARTESIAN_POINT('Origin',(-33.1868376744163,-5.5,-7.2524541285162));
#34130=CARTESIAN_POINT('Origin',(-30.9499643391281,-5.5,-12.8198949842305));
#34131=CARTESIAN_POINT('Origin',(-30.9499643391281,-6.,-12.8198949842305));
#34132=CARTESIAN_POINT('Origin',(-34.8644926758824,-5.5,-3.07687348673046));
#34133=CARTESIAN_POINT('',(-30.3819150461261,-6.,-2.68127546700797));
#34134=CARTESIAN_POINT('',(-30.8799792272101,-5.5,-2.7252308025327));
#34135=CARTESIAN_POINT('Origin',(-30.3819150461261,-5.5,-2.68127546700797));
#34136=CARTESIAN_POINT('Origin',(-34.8644926758824,-5.5,-3.07687348673046));
#34137=CARTESIAN_POINT('Origin',(-34.8644926758824,-6.,-3.07687348673046));
#34138=CARTESIAN_POINT('Origin',(0.,-5.5,0.));
#34139=CARTESIAN_POINT('',(-30.3819150461261,-6.,2.68127546700798));
#34140=CARTESIAN_POINT('',(-30.8799792272101,-5.5,2.7252308025327));
#34141=CARTESIAN_POINT('Origin',(-30.3819150461261,-5.5,2.68127546700798));
#34142=CARTESIAN_POINT('Origin',(0.,-5.5,0.));
#34143=CARTESIAN_POINT('Origin',(0.,-6.,0.));
#34144=CARTESIAN_POINT('Origin',(-34.8644926758824,-5.5,3.07687348673047));
#34145=CARTESIAN_POINT('',(-33.1868376744162,-6.,7.2524541285162));
#34146=CARTESIAN_POINT('',(-33.3732437856903,-5.5,6.78850072387334));
#34147=CARTESIAN_POINT('Origin',(-33.1868376744162,-5.5,7.2524541285162));
#34148=CARTESIAN_POINT('Origin',(-34.8644926758824,-5.5,3.07687348673047));
#34149=CARTESIAN_POINT('Origin',(-34.8644926758824,-6.,3.07687348673047));
#34150=CARTESIAN_POINT('Origin',(-30.9499643391281,-5.5,12.8198949842305));
#34151=CARTESIAN_POINT('',(-28.5948974602351,-6.,18.3383784711987));
#34152=CARTESIAN_POINT('',(-28.398641886994,-5.5,18.7982520951128));
#34153=CARTESIAN_POINT('Origin',(-28.5948974602351,-5.5,18.3383784711987));
#34154=CARTESIAN_POINT('Origin',(-30.9499643391281,-5.5,12.8198949842305));
#34155=CARTESIAN_POINT('Origin',(-30.9499643391281,-6.,12.8198949842305));
#34156=CARTESIAN_POINT('Origin',(-26.8285973010653,-5.5,22.4772410864249));
#34157=CARTESIAN_POINT('',(-23.3792062194998,-6.,19.5873100895989));
#34158=CARTESIAN_POINT('',(-23.7624718952293,-5.5,19.9084135336906));
#34159=CARTESIAN_POINT('Origin',(-23.3792062194998,-5.5,19.5873100895989));
#34160=CARTESIAN_POINT('Origin',(-26.8285973010653,-5.5,22.4772410864249));
#34161=CARTESIAN_POINT('Origin',(-26.8285973010653,-6.,22.4772410864249));
#34162=CARTESIAN_POINT('Origin',(0.,-5.5,0.));
#34163=CARTESIAN_POINT('Origin',(0.,-6.,0.));
#34164=CARTESIAN_POINT('Origin',(0.,-5.5,0.));
#34165=CARTESIAN_POINT('Origin',(3.07687348673046,0.,-34.8644926758824));
#34166=CARTESIAN_POINT('',(2.72523080253269,0.,-30.8799792272101));
#34167=CARTESIAN_POINT('Origin',(0.,0.,0.));
#34168=CARTESIAN_POINT('Origin',(-12.8198949842305,0.,-30.9499643391281));
#34169=CARTESIAN_POINT('',(-18.7982520951128,0.,-28.398641886994));
#34170=CARTESIAN_POINT('Origin',(-22.4772410864249,0.,-26.8285973010653));
#34171=CARTESIAN_POINT('',(-19.9084135336907,0.,-23.7624718952293));
#34172=CARTESIAN_POINT('Origin',(0.,0.,0.));
#34173=CARTESIAN_POINT('',(-23.7624718952293,0.,-19.9084135336907));
#34174=CARTESIAN_POINT('Origin',(-26.8285973010653,0.,-22.4772410864249));
#34175=CARTESIAN_POINT('',(-28.398641886994,0.,-18.7982520951128));
#34176=CARTESIAN_POINT('Origin',(-30.9499643391281,0.,-12.8198949842305));
#34177=CARTESIAN_POINT('',(-33.3732437856903,0.,-6.78850072387334));
#34178=CARTESIAN_POINT('Origin',(-34.8644926758824,0.,-3.07687348673046));
#34179=CARTESIAN_POINT('',(-30.8799792272101,0.,-2.7252308025327));
#34180=CARTESIAN_POINT('Origin',(0.,0.,0.));
#34181=CARTESIAN_POINT('',(-30.8799792272101,0.,2.7252308025327));
#34182=CARTESIAN_POINT('Origin',(-34.8644926758824,0.,3.07687348673047));
#34183=CARTESIAN_POINT('',(-33.3732437856903,0.,6.78850072387334));
#34184=CARTESIAN_POINT('Origin',(-30.9499643391281,0.,12.8198949842305));
#34185=CARTESIAN_POINT('',(-28.398641886994,0.,18.7982520951128));
#34186=CARTESIAN_POINT('Origin',(-26.8285973010653,0.,22.4772410864249));
#34187=CARTESIAN_POINT('',(-23.7624718952293,0.,19.9084135336906));
#34188=CARTESIAN_POINT('Origin',(0.,0.,0.));
#34189=CARTESIAN_POINT('',(-19.9084135336906,0.,23.7624718952293));
#34190=CARTESIAN_POINT('Origin',(-22.4772410864249,0.,26.8285973010654));
#34191=CARTESIAN_POINT('',(-18.7982520951128,0.,28.398641886994));
#34192=CARTESIAN_POINT('Origin',(0.,-6.,0.));
#34193=CARTESIAN_POINT('',(-3.49024337756996E-15,-6.,-28.5));
#34194=CARTESIAN_POINT('Origin',(0.,-6.,0.));
#34195=CARTESIAN_POINT('',(-12.2458698356829,-6.,-29.5641450403612));
#34196=CARTESIAN_POINT('Origin',(-12.8198949842305,-6.,-30.9499643391281));
#34197=CARTESIAN_POINT('',(29.5641450403612,-6.,12.2458698356829));
#34198=CARTESIAN_POINT('Origin',(30.9499643391281,-6.,12.8198949842305));
#34199=CARTESIAN_POINT('',(29.5641450403612,-6.,-12.2458698356829));
#34200=CARTESIAN_POINT('Origin',(30.9499643391281,-6.,-12.8198949842305));
#34201=CARTESIAN_POINT('',(12.2458698356829,-6.,-29.5641450403612));
#34202=CARTESIAN_POINT('Origin',(12.8198949842305,-6.,-30.9499643391281));
#34203=CARTESIAN_POINT('',(-29.5641450403612,-6.,-12.2458698356829));
#34204=CARTESIAN_POINT('Origin',(-30.9499643391281,-6.,-12.8198949842305));
#34205=CARTESIAN_POINT('',(12.2458698356829,-6.,29.5641450403612));
#34206=CARTESIAN_POINT('Origin',(12.8198949842305,-6.,30.9499643391281));
#34207=CARTESIAN_POINT('',(-29.5641450403612,-6.,12.2458698356829));
#34208=CARTESIAN_POINT('Origin',(-30.9499643391281,-6.,12.8198949842305));
#34209=CARTESIAN_POINT('',(-12.2458698356829,-6.,29.5641450403612));
#34210=CARTESIAN_POINT('Origin',(-12.8198949842305,-6.,30.9499643391281));
#34211=CARTESIAN_POINT('Origin',(0.,5.5,0.));
#34212=CARTESIAN_POINT('',(-3.42901103761259E-15,5.5,28.));
#34213=CARTESIAN_POINT('Origin',(-3.49024337756996E-15,5.5,28.5));
#34214=CARTESIAN_POINT('',(-28.,5.5,-3.42901103761259E-15));
#34215=CARTESIAN_POINT('Origin',(0.,5.5,0.));
#34216=CARTESIAN_POINT('Origin',(0.,5.5,0.));
#34217=CARTESIAN_POINT('Origin',(0.,0.,0.));
#34218=CARTESIAN_POINT('',(-28.,-5.5,-3.42901103761259E-15));
#34219=CARTESIAN_POINT('',(-28.,0.,-3.42901103761259E-15));
#34220=CARTESIAN_POINT('',(-3.42901103761259E-15,-5.5,-28.));
#34221=CARTESIAN_POINT('Origin',(0.,-5.5,0.));
#34222=CARTESIAN_POINT('Origin',(0.,-5.5,0.));
#34223=CARTESIAN_POINT('Origin',(0.,-5.5,0.));
#34224=CARTESIAN_POINT('Origin',(-3.49024337756996E-15,-5.5,-28.5));
#34225=CARTESIAN_POINT('Origin',(-12.8198949842305,0.,30.9499643391281));
#34226=CARTESIAN_POINT('Origin',(-12.8198949842305,0.,-30.9499643391281));
#34227=CARTESIAN_POINT('',(-12.2458698356829,0.,-29.5641450403612));
#34228=CARTESIAN_POINT('Origin',(-12.8198949842305,0.,30.9499643391281));
#34229=CARTESIAN_POINT('',(-12.2458698356829,0.,29.5641450403612));
#34230=CARTESIAN_POINT('Origin',(-30.9499643391281,0.,12.8198949842305));
#34231=CARTESIAN_POINT('',(-29.5641450403612,0.,12.2458698356829));
#34232=CARTESIAN_POINT('Origin',(12.8198949842305,0.,30.9499643391281));
#34233=CARTESIAN_POINT('',(12.2458698356829,0.,29.5641450403612));
#34234=CARTESIAN_POINT('Origin',(-30.9499643391281,0.,-12.8198949842305));
#34235=CARTESIAN_POINT('',(-29.5641450403612,0.,-12.2458698356829));
#34236=CARTESIAN_POINT('Origin',(12.8198949842305,0.,-30.9499643391281));
#34237=CARTESIAN_POINT('',(12.2458698356829,0.,-29.5641450403612));
#34238=CARTESIAN_POINT('Origin',(30.9499643391281,0.,-12.8198949842305));
#34239=CARTESIAN_POINT('',(29.5641450403612,0.,-12.2458698356829));
#34240=CARTESIAN_POINT('Origin',(30.9499643391281,0.,12.8198949842305));
#34241=CARTESIAN_POINT('',(29.5641450403612,0.,12.2458698356829));
#34242=CARTESIAN_POINT('',(0.,0.,0.));
#34243=CARTESIAN_POINT('Origin',(0.830812522453709,0.,65.2859978089105));
#34244=CARTESIAN_POINT('',(0.803379378582617,4.93503612692635,65.2));
#34245=CARTESIAN_POINT('',(7.34788079488412E-16,5.,62.6815549174156));
#34246=CARTESIAN_POINT('Origin',(0.,0.,62.6815549174156));
#34247=CARTESIAN_POINT('',(0.803379378582617,-4.93503612692635,65.2));
#34248=CARTESIAN_POINT('',(0.803379378582612,0.,65.2));
#34249=CARTESIAN_POINT('',(0.,-5.,62.6815549174156));
#34250=CARTESIAN_POINT('Origin',(0.,0.,62.6815549174156));
#34251=CARTESIAN_POINT('',(-0.132842333122278,-5.,62.2651188854115));
#34252=CARTESIAN_POINT('',(-2.71467767788293,-5.,54.1715447890402));
#34253=CARTESIAN_POINT('',(-0.132842333122278,5.,62.2651188854115));
#34254=CARTESIAN_POINT('',(-0.132842333122279,0.,62.2651188854115));
#34255=CARTESIAN_POINT('',(0.0561576033527066,5.,62.8575985697469));
#34256=CARTESIAN_POINT('Origin',(5.37767154318555,0.,-175.976317607651));
#34257=CARTESIAN_POINT('',(-2.50665419388694,5.,65.2));
#34258=CARTESIAN_POINT('',(-2.50665419388694,-5.,65.2));
#34259=CARTESIAN_POINT('',(-2.50665419388694,0.,65.2));
#34260=CARTESIAN_POINT('',(-44.1089505723395,5.,60.2));
#34261=CARTESIAN_POINT('Origin',(5.37767154318555,5.,-175.976317607651));
#34262=CARTESIAN_POINT('',(-58.8319403691538,5.,56.6291520296333));
#34263=CARTESIAN_POINT('Origin',(5.37767154318555,5.,-175.976317607651));
#34264=CARTESIAN_POINT('',(-58.8319403691538,-5.,56.6291520296333));
#34265=CARTESIAN_POINT('Ctrl Pts',(-58.8319403691537,5.,56.6291520296327));
#34266=CARTESIAN_POINT('Ctrl Pts',(-59.4371717203624,5.,56.462080850099));
#34267=CARTESIAN_POINT('Ctrl Pts',(-60.0820298794635,4.8745596841293,56.2812672524265));
#34268=CARTESIAN_POINT('Ctrl Pts',(-61.2669951292512,4.36431020272779,55.9440278549618));
#34269=CARTESIAN_POINT('Ctrl Pts',(-61.8071398573752,3.97949928040823,55.787736975236));
#34270=CARTESIAN_POINT('Ctrl Pts',(-62.6594830508905,3.09160718989329,55.538954977214));
#34271=CARTESIAN_POINT('Ctrl Pts',(-63.0285088739547,2.52936940640579,55.4299017162816));
#34272=CARTESIAN_POINT('Ctrl Pts',(-63.5176931208654,1.2974722333072,55.2847309692003));
#34273=CARTESIAN_POINT('Ctrl Pts',(-63.6378916523671,0.627812963559375,
55.2487476511034));
#34274=CARTESIAN_POINT('Ctrl Pts',(-63.6378916523671,0.,55.2487476511034));
#34275=CARTESIAN_POINT('Ctrl Pts',(-63.6378916523671,-0.627812963559374,
55.2487476511034));
#34276=CARTESIAN_POINT('Ctrl Pts',(-63.5176931208654,-1.29747223330721,
55.2847309692003));
#34277=CARTESIAN_POINT('Ctrl Pts',(-63.0285088739547,-2.52936940640579,
55.4299017162816));
#34278=CARTESIAN_POINT('Ctrl Pts',(-62.6594830508905,-3.09160718989328,
55.538954977214));
#34279=CARTESIAN_POINT('Ctrl Pts',(-61.8071398573752,-3.97949928040822,
55.787736975236));
#34280=CARTESIAN_POINT('Ctrl Pts',(-61.2669951292511,-4.36431020272779,
55.9440278549618));
#34281=CARTESIAN_POINT('Ctrl Pts',(-60.0820298794635,-4.8745596841293,56.2812672524264));
#34282=CARTESIAN_POINT('Ctrl Pts',(-59.4371717203624,-5.,56.462080850099));
#34283=CARTESIAN_POINT('Ctrl Pts',(-58.8319403691537,-5.,56.6291520296327));
#34284=CARTESIAN_POINT('',(-44.1089505723395,-5.,60.2));
#34285=CARTESIAN_POINT('Origin',(5.37767154318555,-5.,-175.976317607651));
#34286=CARTESIAN_POINT('Origin',(5.37767154318555,-5.,-175.976317607651));
#34287=CARTESIAN_POINT('Origin',(-57.5900824922669,0.,52.468515568381));
#34288=CARTESIAN_POINT('',(-57.973725345055,5.,53.7538465801794));
#34289=CARTESIAN_POINT('',(-57.973725345055,-5.,53.7538465801794));
#34290=CARTESIAN_POINT('Ctrl Pts',(-57.9737253450549,-5.,53.753846580179));
#34291=CARTESIAN_POINT('Ctrl Pts',(-58.5790016453339,-5.,53.5869329349396));
#34292=CARTESIAN_POINT('Ctrl Pts',(-59.2238994944327,-4.8745603906429,53.4062543439228));
#34293=CARTESIAN_POINT('Ctrl Pts',(-60.408922048283,-4.36431138570487,53.0692049403301));
#34294=CARTESIAN_POINT('Ctrl Pts',(-60.9490848335127,-3.97950018878322,
52.9129707557609));
#34295=CARTESIAN_POINT('Ctrl Pts',(-61.8014482334478,-3.09160726119939,
52.6642535292407));
#34296=CARTESIAN_POINT('Ctrl Pts',(-62.1704778415824,-2.52936950626686,
52.5552128954911));
#34297=CARTESIAN_POINT('Ctrl Pts',(-62.6596650198333,-1.2974723188127,52.4100518473254));
#34298=CARTESIAN_POINT('Ctrl Pts',(-62.7798632032036,-0.627813009191178,
52.3740672896673));
#34299=CARTESIAN_POINT('Ctrl Pts',(-62.7798632032036,0.,52.3740672896673));
#34300=CARTESIAN_POINT('Ctrl Pts',(-62.7798632032036,0.627813009191178,
52.3740672896673));
#34301=CARTESIAN_POINT('Ctrl Pts',(-62.6596650198333,1.2974723188127,52.4100518473254));
#34302=CARTESIAN_POINT('Ctrl Pts',(-62.1704778415824,2.52936950626686,52.5552128954911));
#34303=CARTESIAN_POINT('Ctrl Pts',(-61.8014482334478,3.09160726119939,52.6642535292407));
#34304=CARTESIAN_POINT('Ctrl Pts',(-60.9490848335127,3.97950018878322,52.9129707557609));
#34305=CARTESIAN_POINT('Ctrl Pts',(-60.4089220482829,4.36431138570488,53.0692049403301));
#34306=CARTESIAN_POINT('Ctrl Pts',(-59.2238994944327,4.8745603906429,53.4062543439228));
#34307=CARTESIAN_POINT('Ctrl Pts',(-58.5790016453339,5.,53.5869329349396));
#34308=CARTESIAN_POINT('Ctrl Pts',(-57.9737253450549,5.,53.753846580179));
#34309=CARTESIAN_POINT('',(-57.5900824922669,-5.,52.468515568381));
#34310=CARTESIAN_POINT('',(-57.5900824922669,5.,52.468515568381));
#34311=CARTESIAN_POINT('Origin',(5.37767154318555,0.,-175.976317607651));
#34312=CARTESIAN_POINT('',(-26.4043174875352,5.,60.2));
#34313=CARTESIAN_POINT('Origin',(5.37767154318555,5.,-175.976317607651));
#34314=CARTESIAN_POINT('Origin',(5.37767154318555,5.,-175.976317607651));
#34315=CARTESIAN_POINT('',(-26.4043174875352,-5.,60.2));
#34316=CARTESIAN_POINT('Origin',(5.37767154318555,-5.,-175.976317607651));
#34317=CARTESIAN_POINT('Origin',(5.37767154318555,-5.,-175.976317607651));
#34318=CARTESIAN_POINT('Origin',(-31.4035395649567,-5.,58.8300325492891));
#34319=CARTESIAN_POINT('',(-45.,-5.,60.2));
#34320=CARTESIAN_POINT('Origin',(-31.4035395649567,5.,58.8300325492891));
#34321=CARTESIAN_POINT('',(-15.,5.,60.2));
#34322=CARTESIAN_POINT('Origin',(-3.67394039744206E-16,5.,60.2));
#34323=CARTESIAN_POINT('',(-60.,5.,65.2));
#34324=CARTESIAN_POINT('',(-15.,5.,65.2));
#34325=CARTESIAN_POINT('',(-60.,5.,60.2));
#34326=CARTESIAN_POINT('',(-60.,5.,60.2));
#34327=CARTESIAN_POINT('',(-15.,5.,60.2));
#34328=CARTESIAN_POINT('Origin',(-30.,0.,65.2));
#34329=CARTESIAN_POINT('',(-60.,-5.,65.2));
#34330=CARTESIAN_POINT('',(-45.,-5.,65.2));
#34331=CARTESIAN_POINT('Origin',(-60.,0.,65.2));
#34332=CARTESIAN_POINT('Origin',(-60.,-5.,60.2));
#34333=CARTESIAN_POINT('',(0.,-5.,60.2));
#34334=CARTESIAN_POINT('',(0.,-5.,60.2));
#34335=CARTESIAN_POINT('',(-45.,-5.,60.2));
#34336=CARTESIAN_POINT('Origin',(-60.,-5.,60.2));
#34337=CARTESIAN_POINT('',(-60.,-5.,60.2));
#34338=CARTESIAN_POINT('',(-45.,-5.,60.2));
#34339=CARTESIAN_POINT('',(-60.,-5.,60.2));
#34340=CARTESIAN_POINT('Origin',(-60.,0.,60.2));
#34341=CARTESIAN_POINT('Origin',(-60.,0.,60.2));
#34342=CARTESIAN_POINT('Origin',(-3.67394039744206E-16,5.,60.2));
#34343=CARTESIAN_POINT('',(3.67394039744206E-16,5.,60.2));
#34344=CARTESIAN_POINT('',(-15.,5.,60.2));
#34345=CARTESIAN_POINT('',(7.34788079488412E-16,5.,60.2));
#34346=CARTESIAN_POINT('Origin',(0.,0.,60.2));
#34347=CARTESIAN_POINT('Origin',(0.,0.,60.2));
#34348=CARTESIAN_POINT('Origin',(0.,0.,65.2));
#34349=CARTESIAN_POINT('Origin',(-30.,0.,65.2));
#34350=CARTESIAN_POINT('Origin',(-60.,-6.,60.2));
#34351=CARTESIAN_POINT('',(-60.,-6.,60.2));
#34352=CARTESIAN_POINT('',(0.,-6.,60.2));
#34353=CARTESIAN_POINT('',(-60.,-6.,60.2));
#34354=CARTESIAN_POINT('',(0.,-6.,66.2));
#34355=CARTESIAN_POINT('',(0.,-6.,60.2));
#34356=CARTESIAN_POINT('',(-60.,-6.,66.2));
#34357=CARTESIAN_POINT('',(-60.,-6.,66.2));
#34358=CARTESIAN_POINT('',(-60.,-6.,60.2));
#34359=CARTESIAN_POINT('Origin',(-60.,0.,60.2));
#34360=CARTESIAN_POINT('',(-60.,6.,60.2));
#34361=CARTESIAN_POINT('Origin',(-60.,0.,60.2));
#34362=CARTESIAN_POINT('',(-60.,6.,66.2));
#34363=CARTESIAN_POINT('Origin',(-60.,0.,66.2));
#34364=CARTESIAN_POINT('',(-60.,6.,60.2));
#34365=CARTESIAN_POINT('Origin',(-3.67394039744206E-16,6.,60.2));
#34366=CARTESIAN_POINT('',(7.34788079488412E-16,6.,60.2));
#34367=CARTESIAN_POINT('',(-3.67394039744206E-16,6.,60.2));
#34368=CARTESIAN_POINT('',(7.34788079488412E-16,6.,66.2));
#34369=CARTESIAN_POINT('',(-3.67394039744206E-16,6.,66.2));
#34370=CARTESIAN_POINT('',(7.34788079488412E-16,6.,60.2));
#34371=CARTESIAN_POINT('Origin',(0.,0.,60.2));
#34372=CARTESIAN_POINT('Origin',(0.,0.,60.2));
#34373=CARTESIAN_POINT('Origin',(0.,0.,66.2));
#34374=CARTESIAN_POINT('Origin',(-30.,0.,66.2));
#34375=CARTESIAN_POINT('Origin',(-30.,0.,60.2));
#34376=CARTESIAN_POINT('',(0.,0.,0.));
#34377=CARTESIAN_POINT('',(0.,0.,0.));
#34378=CARTESIAN_POINT('',(0.,0.,0.));
#34379=CARTESIAN_POINT('',(0.,0.,0.));
#34380=CARTESIAN_POINT('',(0.,0.,0.));
#34381=CARTESIAN_POINT('',(0.,0.,0.));
#34382=CARTESIAN_POINT('',(0.,0.,0.));
#34383=CARTESIAN_POINT('',(0.,0.,0.));
#34384=UNCERTAINTY_MEASURE_WITH_UNIT(LENGTH_MEASURE(0.01),#34404,
'DISTANCE_ACCURACY_VALUE',
'Maximum model space distance between geometric entities at asserted c
onnectivities');
#34385=UNCERTAINTY_MEASURE_WITH_UNIT(LENGTH_MEASURE(0.01),#34404,
'DISTANCE_ACCURACY_VALUE',
'Maximum model space distance between geometric entities at asserted c
onnectivities');
#34386=UNCERTAINTY_MEASURE_WITH_UNIT(LENGTH_MEASURE(0.01),#34404,
'DISTANCE_ACCURACY_VALUE',
'Maximum model space distance between geometric entities at asserted c
onnectivities');
#34387=UNCERTAINTY_MEASURE_WITH_UNIT(LENGTH_MEASURE(0.01),#34404,
'DISTANCE_ACCURACY_VALUE',
'Maximum model space distance between geometric entities at asserted c
onnectivities');
#34388=UNCERTAINTY_MEASURE_WITH_UNIT(LENGTH_MEASURE(0.01),#34404,
'DISTANCE_ACCURACY_VALUE',
'Maximum model space distance between geometric entities at asserted c
onnectivities');
#34389=UNCERTAINTY_MEASURE_WITH_UNIT(LENGTH_MEASURE(0.01),#34404,
'DISTANCE_ACCURACY_VALUE',
'Maximum model space distance between geometric entities at asserted c
onnectivities');
#34390=UNCERTAINTY_MEASURE_WITH_UNIT(LENGTH_MEASURE(0.01),#34404,
'DISTANCE_ACCURACY_VALUE',
'Maximum model space distance between geometric entities at asserted c
onnectivities');
#34391=UNCERTAINTY_MEASURE_WITH_UNIT(LENGTH_MEASURE(0.01),#34404,
'DISTANCE_ACCURACY_VALUE',
'Maximum model space distance between geometric entities at asserted c
onnectivities');
#34392=UNCERTAINTY_MEASURE_WITH_UNIT(LENGTH_MEASURE(0.01),#34404,
'DISTANCE_ACCURACY_VALUE',
'Maximum model space distance between geometric entities at asserted c
onnectivities');
#34393=UNCERTAINTY_MEASURE_WITH_UNIT(LENGTH_MEASURE(0.01),#34404,
'DISTANCE_ACCURACY_VALUE',
'Maximum model space distance between geometric entities at asserted c
onnectivities');
#34394=(
GEOMETRIC_REPRESENTATION_CONTEXT(3)
GLOBAL_UNCERTAINTY_ASSIGNED_CONTEXT((#34384))
GLOBAL_UNIT_ASSIGNED_CONTEXT((#34404,#34406,#34407))
REPRESENTATION_CONTEXT('','3D')
);
#34395=(
GEOMETRIC_REPRESENTATION_CONTEXT(3)
GLOBAL_UNCERTAINTY_ASSIGNED_CONTEXT((#34385))
GLOBAL_UNIT_ASSIGNED_CONTEXT((#34404,#34406,#34407))
REPRESENTATION_CONTEXT('','3D')
);
#34396=(
GEOMETRIC_REPRESENTATION_CONTEXT(3)
GLOBAL_UNCERTAINTY_ASSIGNED_CONTEXT((#34386))
GLOBAL_UNIT_ASSIGNED_CONTEXT((#34404,#34406,#34407))
REPRESENTATION_CONTEXT('','3D')
);
#34397=(
GEOMETRIC_REPRESENTATION_CONTEXT(3)
GLOBAL_UNCERTAINTY_ASSIGNED_CONTEXT((#34387))
GLOBAL_UNIT_ASSIGNED_CONTEXT((#34404,#34406,#34407))
REPRESENTATION_CONTEXT('','3D')
);
#34398=(
GEOMETRIC_REPRESENTATION_CONTEXT(3)
GLOBAL_UNCERTAINTY_ASSIGNED_CONTEXT((#34388))
GLOBAL_UNIT_ASSIGNED_CONTEXT((#34404,#34406,#34407))
REPRESENTATION_CONTEXT('','3D')
);
#34399=(
GEOMETRIC_REPRESENTATION_CONTEXT(3)
GLOBAL_UNCERTAINTY_ASSIGNED_CONTEXT((#34389))
GLOBAL_UNIT_ASSIGNED_CONTEXT((#34404,#34406,#34407))
REPRESENTATION_CONTEXT('','3D')
);
#34400=(
GEOMETRIC_REPRESENTATION_CONTEXT(3)
GLOBAL_UNCERTAINTY_ASSIGNED_CONTEXT((#34390))
GLOBAL_UNIT_ASSIGNED_CONTEXT((#34404,#34406,#34407))
REPRESENTATION_CONTEXT('','3D')
);
#34401=(
GEOMETRIC_REPRESENTATION_CONTEXT(3)
GLOBAL_UNCERTAINTY_ASSIGNED_CONTEXT((#34391))
GLOBAL_UNIT_ASSIGNED_CONTEXT((#34404,#34406,#34407))
REPRESENTATION_CONTEXT('','3D')
);
#34402=(
GEOMETRIC_REPRESENTATION_CONTEXT(3)
GLOBAL_UNCERTAINTY_ASSIGNED_CONTEXT((#34392))
GLOBAL_UNIT_ASSIGNED_CONTEXT((#34404,#34406,#34407))
REPRESENTATION_CONTEXT('','3D')
);
#34403=(
GEOMETRIC_REPRESENTATION_CONTEXT(3)
GLOBAL_UNCERTAINTY_ASSIGNED_CONTEXT((#34393))
GLOBAL_UNIT_ASSIGNED_CONTEXT((#34404,#34406,#34407))
REPRESENTATION_CONTEXT('','3D')
);
#34404=(
LENGTH_UNIT()
NAMED_UNIT(*)
SI_UNIT(.MILLI.,.METRE.)
);
#34405=(
LENGTH_UNIT()
NAMED_UNIT(*)
SI_UNIT($,.METRE.)
);
#34406=(
NAMED_UNIT(*)
PLANE_ANGLE_UNIT()
SI_UNIT($,.RADIAN.)
);
#34407=(
NAMED_UNIT(*)
SI_UNIT($,.STERADIAN.)
SOLID_ANGLE_UNIT()
);
#34408=SHAPE_DEFINITION_REPRESENTATION(#34417,#34434);
#34409=SHAPE_DEFINITION_REPRESENTATION(#34418,#34435);
#34410=SHAPE_DEFINITION_REPRESENTATION(#34419,#34436);
#34411=SHAPE_DEFINITION_REPRESENTATION(#34420,#34437);
#34412=SHAPE_DEFINITION_REPRESENTATION(#34421,#34438);
#34413=SHAPE_DEFINITION_REPRESENTATION(#34422,#34439);
#34414=SHAPE_DEFINITION_REPRESENTATION(#34423,#34440);
#34415=SHAPE_DEFINITION_REPRESENTATION(#34424,#34441);
#34416=SHAPE_DEFINITION_REPRESENTATION(#34425,#34442);
#34417=PRODUCT_DEFINITION_SHAPE('',$,#34444);
#34418=PRODUCT_DEFINITION_SHAPE('',$,#34445);
#34419=PRODUCT_DEFINITION_SHAPE('',$,#34446);
#34420=PRODUCT_DEFINITION_SHAPE('',$,#34447);
#34421=PRODUCT_DEFINITION_SHAPE('',$,#34448);
#34422=PRODUCT_DEFINITION_SHAPE('',$,#34449);
#34423=PRODUCT_DEFINITION_SHAPE('',$,#34450);
#34424=PRODUCT_DEFINITION_SHAPE('',$,#34451);
#34425=PRODUCT_DEFINITION_SHAPE('',$,#34452);
#34426=PRODUCT_DEFINITION_SHAPE($,$,#35);
#34427=PRODUCT_DEFINITION_SHAPE($,$,#36);
#34428=PRODUCT_DEFINITION_SHAPE($,$,#37);
#34429=PRODUCT_DEFINITION_SHAPE($,$,#38);
#34430=PRODUCT_DEFINITION_SHAPE($,$,#39);
#34431=PRODUCT_DEFINITION_SHAPE($,$,#40);
#34432=PRODUCT_DEFINITION_SHAPE($,$,#41);
#34433=PRODUCT_DEFINITION_SHAPE($,$,#42);
#34434=SHAPE_REPRESENTATION('',(#4479,#4995,#4996,#4997,#4998,#4999,#5000,
#5001,#5002),#34394);
#34435=SHAPE_REPRESENTATION('',(#4480),#34395);
#34436=SHAPE_REPRESENTATION('',(#4507),#34396);
#34437=SHAPE_REPRESENTATION('',(#4513),#34397);
#34438=SHAPE_REPRESENTATION('',(#4522),#34398);
#34439=SHAPE_REPRESENTATION('',(#4557),#34399);
#34440=SHAPE_REPRESENTATION('',(#4579),#34400);
#34441=SHAPE_REPRESENTATION('',(#4604),#34401);
#34442=SHAPE_REPRESENTATION('',(#4956),#34402);
#34443=PRODUCT_DEFINITION_CONTEXT('part definition',#34472,'design');
#34444=PRODUCT_DEFINITION('BR-303','BR-303',#34453,#34443);
#34445=PRODUCT_DEFINITION('Ring','Ring',#34454,#34443);
#34446=PRODUCT_DEFINITION('Disc','Disc',#34455,#34443);
#34447=PRODUCT_DEFINITION('Retainer_Ring','Retainer_Ring',#34456,#34443);
#34448=PRODUCT_DEFINITION('Extended_Neck','Extended_Neck',#34457,#34443);
#34449=PRODUCT_DEFINITION('Bushing_01','Bushing_01',#34458,#34443);
#34450=PRODUCT_DEFINITION('Bushing_02','Bushing_02',#34459,#34443);
#34451=PRODUCT_DEFINITION('Steel_Body','Steel_Body',#34460,#34443);
#34452=PRODUCT_DEFINITION('Handle','Handle',#34461,#34443);
#34453=PRODUCT_DEFINITION_FORMATION('',$,#34474);
#34454=PRODUCT_DEFINITION_FORMATION('',$,#34475);
#34455=PRODUCT_DEFINITION_FORMATION('',$,#34476);
#34456=PRODUCT_DEFINITION_FORMATION('',$,#34477);
#34457=PRODUCT_DEFINITION_FORMATION('',$,#34478);
#34458=PRODUCT_DEFINITION_FORMATION('',$,#34479);
#34459=PRODUCT_DEFINITION_FORMATION('',$,#34480);
#34460=PRODUCT_DEFINITION_FORMATION('',$,#34481);
#34461=PRODUCT_DEFINITION_FORMATION('',$,#34482);
#34462=PRODUCT_RELATED_PRODUCT_CATEGORY('BR-303','BR-303',(#34474));
#34463=PRODUCT_RELATED_PRODUCT_CATEGORY('Ring','Ring',(#34475));
#34464=PRODUCT_RELATED_PRODUCT_CATEGORY('Disc','Disc',(#34476));
#34465=PRODUCT_RELATED_PRODUCT_CATEGORY('Retainer_Ring','Retainer_Ring',
(#34477));
#34466=PRODUCT_RELATED_PRODUCT_CATEGORY('Extended_Neck','Extended_Neck',
(#34478));
#34467=PRODUCT_RELATED_PRODUCT_CATEGORY('Bushing_01','Bushing_01',(#34479));
#34468=PRODUCT_RELATED_PRODUCT_CATEGORY('Bushing_02','Bushing_02',(#34480));
#34469=PRODUCT_RELATED_PRODUCT_CATEGORY('Steel_Body','Steel_Body',(#34481));
#34470=PRODUCT_RELATED_PRODUCT_CATEGORY('Handle','Handle',(#34482));
#34471=APPLICATION_PROTOCOL_DEFINITION('international standard',
'automotive_design',2009,#34472);
#34472=APPLICATION_CONTEXT(
'Core Data for Automotive Mechanical Design Process');
#34473=PRODUCT_CONTEXT('part definition',#34472,'mechanical');
#34474=PRODUCT('BR-303','BR-303',$,(#34473));
#34475=PRODUCT('Ring','Ring',$,(#34473));
#34476=PRODUCT('Disc','Disc',$,(#34473));
#34477=PRODUCT('Retainer_Ring','Retainer_Ring',$,(#34473));
#34478=PRODUCT('Extended_Neck','Extended_Neck',$,(#34473));
#34479=PRODUCT('Bushing_01','Bushing_01',$,(#34473));
#34480=PRODUCT('Bushing_02','Bushing_02',$,(#34473));
#34481=PRODUCT('Steel_Body','Steel_Body',$,(#34473));
#34482=PRODUCT('Handle','Handle',$,(#34473));
#34483=PRESENTATION_STYLE_ASSIGNMENT((#34485));
#34484=PRESENTATION_STYLE_ASSIGNMENT((#34486));
#34485=SURFACE_STYLE_USAGE(.BOTH.,#34487);
#34486=SURFACE_STYLE_USAGE(.BOTH.,#34488);
#34487=SURFACE_SIDE_STYLE('',(#34489));
#34488=SURFACE_SIDE_STYLE('',(#34490));
#34489=SURFACE_STYLE_FILL_AREA(#34491);
#34490=SURFACE_STYLE_FILL_AREA(#34492);
#34491=FILL_AREA_STYLE('Steel - Satin',(#34493));
#34492=FILL_AREA_STYLE('Opaque(160,160,160)',(#34494));
#34493=FILL_AREA_STYLE_COLOUR('Steel - Satin',#34495);
#34494=FILL_AREA_STYLE_COLOUR('Opaque(160,160,160)',#34496);
#34495=COLOUR_RGB('Steel - Satin', 0.09019608, 0.27058824, 0.51372549);
#34496=COLOUR_RGB('Opaque(160,160,160)', 0.09019608, 0.27058824, 0.51372549);
ENDSEC;
END-ISO-10303-21;
